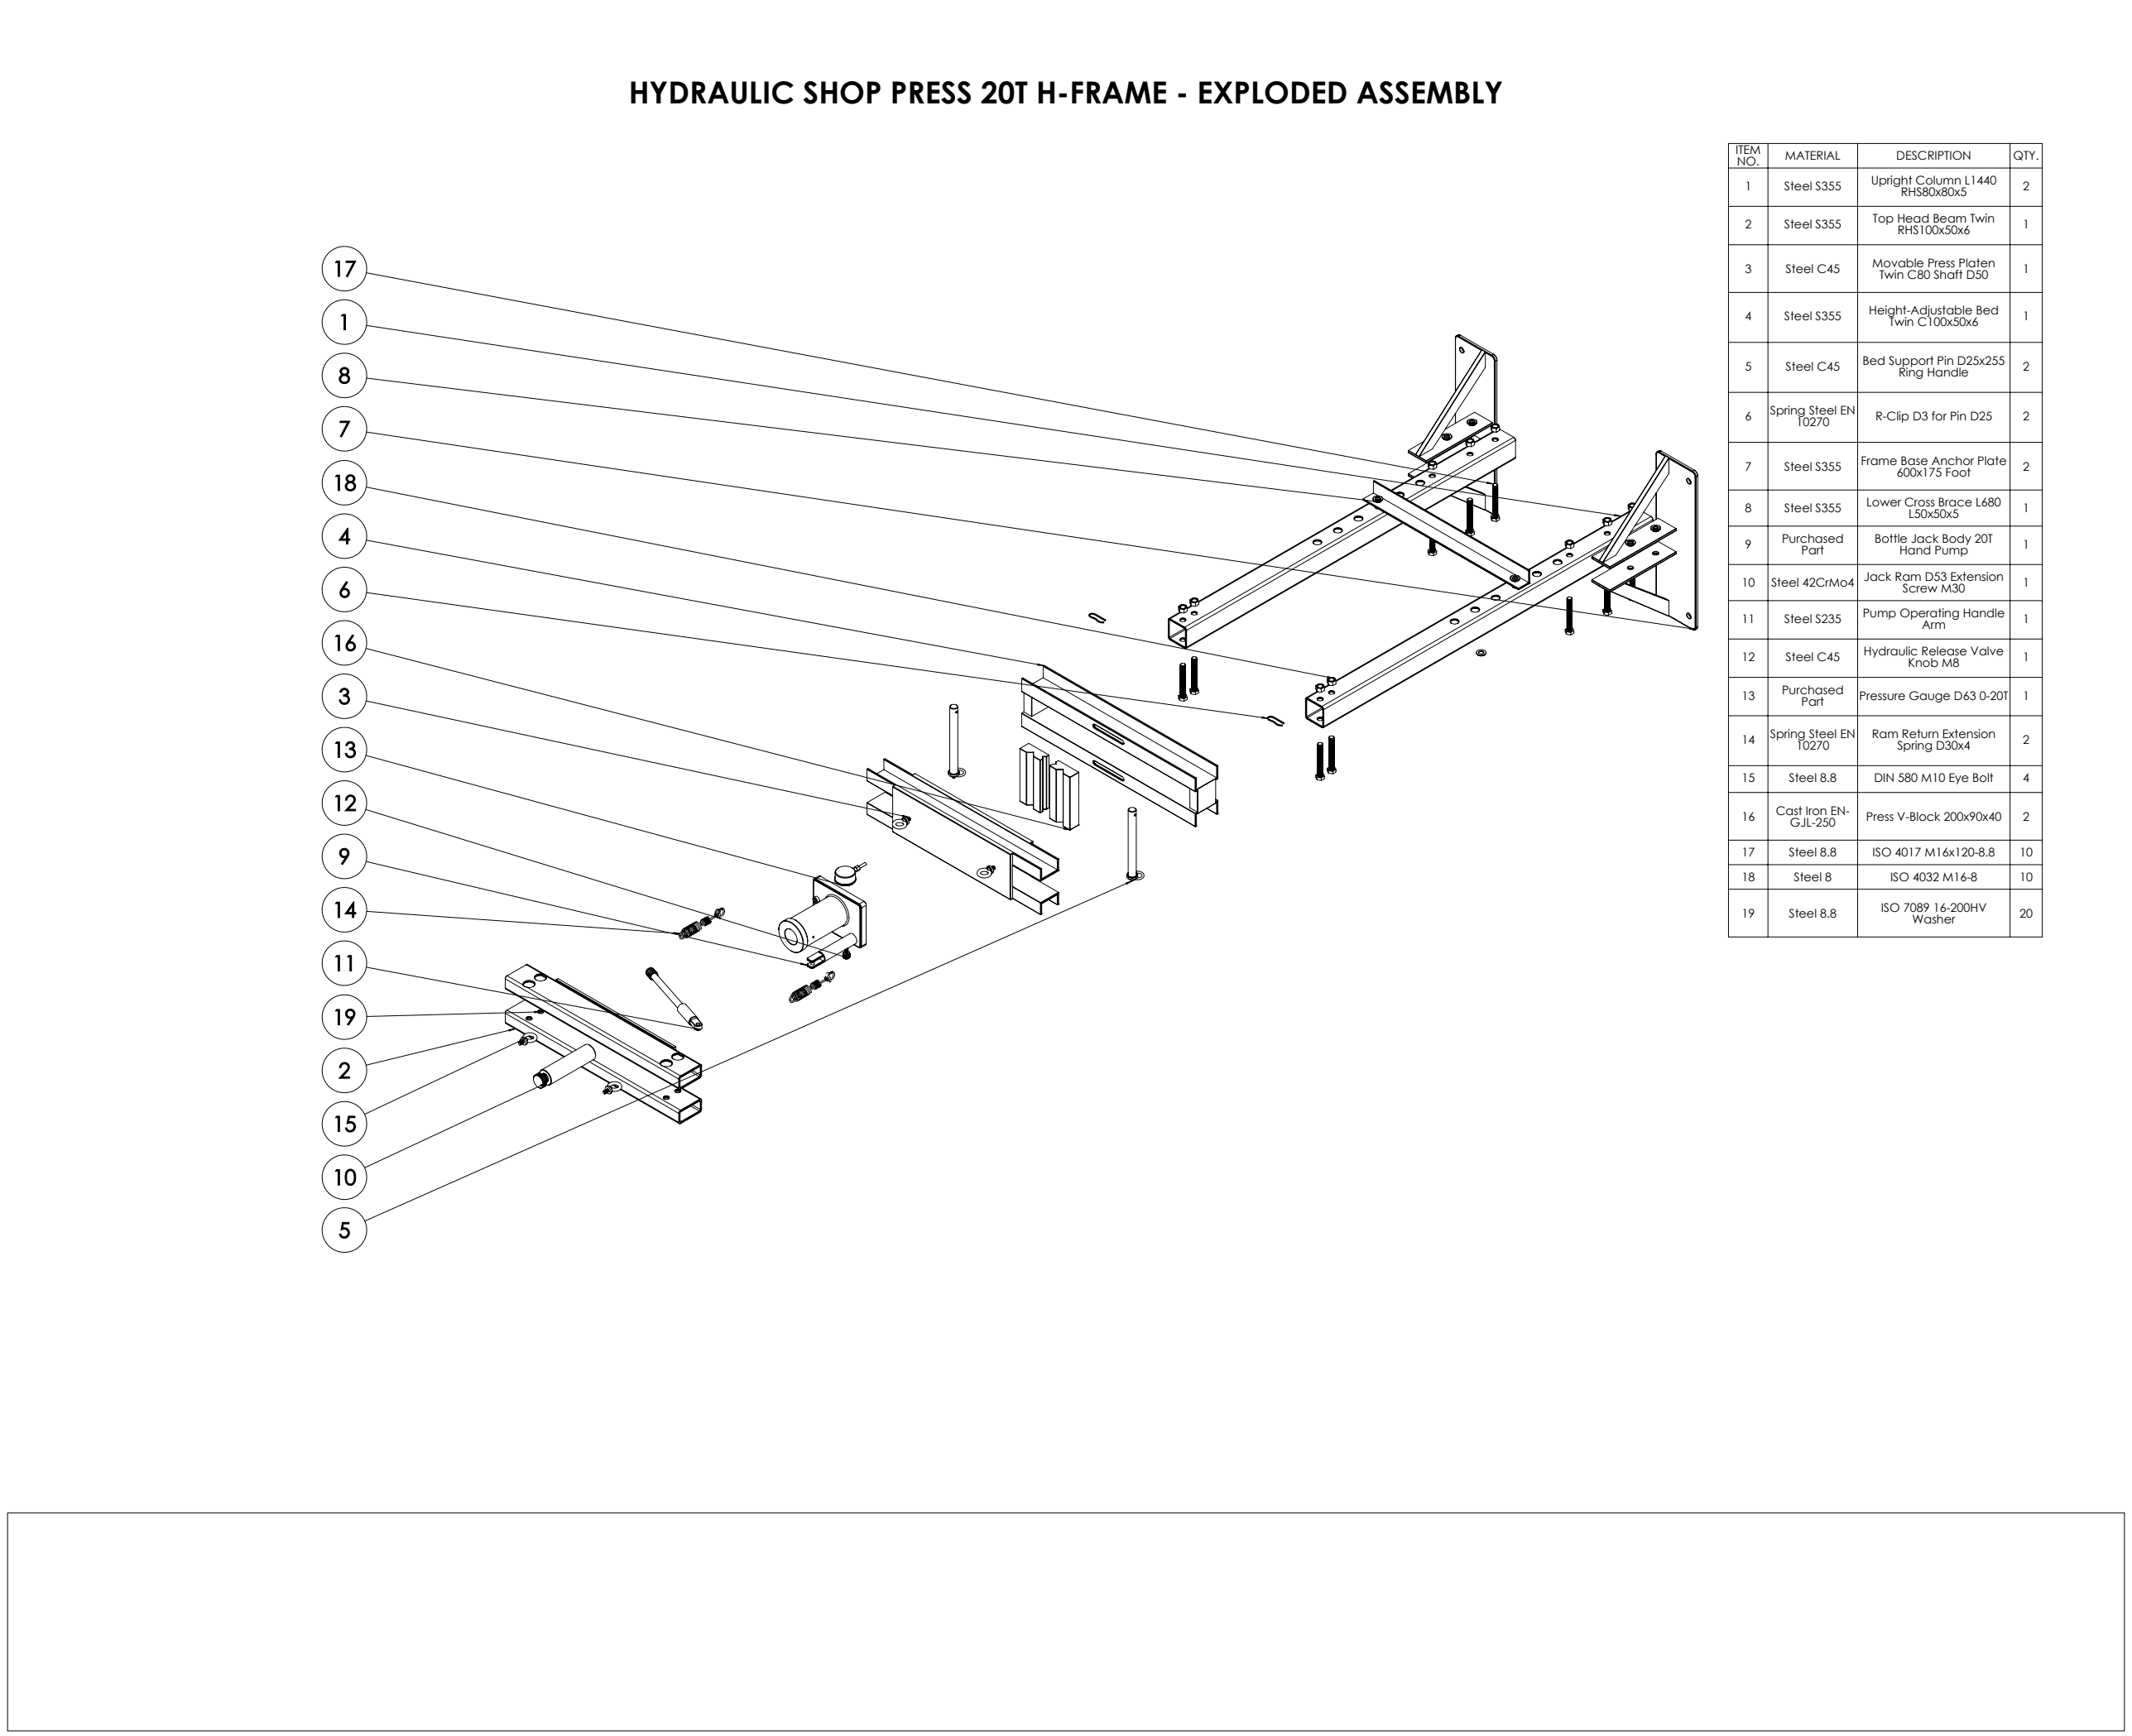
ISO-10303-21;
HEADER;
/* Generated by software containing ST-Developer
 * from STEP Tools, Inc. (www.steptools.com) 
 */

FILE_DESCRIPTION(
/* description */ (''),
/* implementation_level */ '2;1');

FILE_NAME(
/* name */ 'MAS-306',
/* time_stamp */ '2026-10-20T10:03:03-07:00',
/* author */ (''),
/* organization */ (''),
/* preprocessor_version */ 'ST-DEVELOPER v20.2',
/* originating_system */ 'Autodesk Translation Framework v15.15.0.0',
/* authorisation */ '');

FILE_SCHEMA (('AUTOMOTIVE_DESIGN { 1 0 10303 214 3 1 1 }'));
ENDSEC;

DATA;
#10=MECHANICAL_DESIGN_GEOMETRIC_PRESENTATION_REPRESENTATION('',(#439,#440,
#441,#442,#443,#444,#445,#446,#447,#448,#449,#450,#451,#452,#453,#454,#455,
#456,#457,#458,#459,#460,#461,#462,#463,#464,#465,#466,#467,#468,#469,#470,
#471,#472,#473,#474,#475,#476,#477,#478,#479,#480,#481,#482,#483,#484,#485,
#486,#487,#488,#489,#490,#491,#492,#493,#494,#495,#496,#497,#498,#499,#500,
#501,#502,#503,#504,#505,#506,#507,#508,#509,#510,#511,#512,#513,#514,#515,
#516,#517,#518,#519,#520,#521,#522,#523,#524,#525,#526,#527,#528,#529,#530,
#531,#532,#533,#534,#535,#536,#537,#538,#539,#540,#541,#542,#543,#544,#545,
#546,#547,#548,#549,#550),#71492);
#11=ITEM_DEFINED_TRANSFORMATION($,$,#30553,#30790);
#12=ITEM_DEFINED_TRANSFORMATION($,$,#28689,#30791);
#13=ITEM_DEFINED_TRANSFORMATION($,$,#29045,#30792);
#14=ITEM_DEFINED_TRANSFORMATION($,$,#29181,#30793);
#15=ITEM_DEFINED_TRANSFORMATION($,$,#29982,#30794);
#16=ITEM_DEFINED_TRANSFORMATION($,$,#30008,#30795);
#17=ITEM_DEFINED_TRANSFORMATION($,$,#30013,#30796);
#18=ITEM_DEFINED_TRANSFORMATION($,$,#29306,#30797);
#19=ITEM_DEFINED_TRANSFORMATION($,$,#29346,#30798);
#20=ITEM_DEFINED_TRANSFORMATION($,$,#29535,#30799);
#21=ITEM_DEFINED_TRANSFORMATION($,$,#29736,#30800);
#22=ITEM_DEFINED_TRANSFORMATION($,$,#29878,#30801);
#23=ITEM_DEFINED_TRANSFORMATION($,$,#30164,#30802);
#24=ITEM_DEFINED_TRANSFORMATION($,$,#30184,#30803);
#25=ITEM_DEFINED_TRANSFORMATION($,$,#30238,#30804);
#26=ITEM_DEFINED_TRANSFORMATION($,$,#30284,#30805);
#27=ITEM_DEFINED_TRANSFORMATION($,$,#30444,#30806);
#28=ITEM_DEFINED_TRANSFORMATION($,$,#30464,#30807);
#29=ITEM_DEFINED_TRANSFORMATION($,$,#29982,#30808);
#30=ITEM_DEFINED_TRANSFORMATION($,$,#30008,#30809);
#31=ITEM_DEFINED_TRANSFORMATION($,$,#30013,#30810);
#32=ITEM_DEFINED_TRANSFORMATION($,$,#30164,#30811);
#33=ITEM_DEFINED_TRANSFORMATION($,$,#30184,#30812);
#34=ITEM_DEFINED_TRANSFORMATION($,$,#30184,#30813);
#35=ITEM_DEFINED_TRANSFORMATION($,$,#30184,#30814);
#36=ITEM_DEFINED_TRANSFORMATION($,$,#30238,#30815);
#37=ITEM_DEFINED_TRANSFORMATION($,$,#30284,#30816);
#38=ITEM_DEFINED_TRANSFORMATION($,$,#30284,#30817);
#39=ITEM_DEFINED_TRANSFORMATION($,$,#30284,#30818);
#40=ITEM_DEFINED_TRANSFORMATION($,$,#30284,#30819);
#41=ITEM_DEFINED_TRANSFORMATION($,$,#30284,#30820);
#42=ITEM_DEFINED_TRANSFORMATION($,$,#30284,#30821);
#43=ITEM_DEFINED_TRANSFORMATION($,$,#30284,#30822);
#44=ITEM_DEFINED_TRANSFORMATION($,$,#30284,#30823);
#45=ITEM_DEFINED_TRANSFORMATION($,$,#30284,#30824);
#46=ITEM_DEFINED_TRANSFORMATION($,$,#30444,#30825);
#47=ITEM_DEFINED_TRANSFORMATION($,$,#30444,#30826);
#48=ITEM_DEFINED_TRANSFORMATION($,$,#30444,#30827);
#49=ITEM_DEFINED_TRANSFORMATION($,$,#30444,#30828);
#50=ITEM_DEFINED_TRANSFORMATION($,$,#30444,#30829);
#51=ITEM_DEFINED_TRANSFORMATION($,$,#30444,#30830);
#52=ITEM_DEFINED_TRANSFORMATION($,$,#30444,#30831);
#53=ITEM_DEFINED_TRANSFORMATION($,$,#30444,#30832);
#54=ITEM_DEFINED_TRANSFORMATION($,$,#30444,#30833);
#55=ITEM_DEFINED_TRANSFORMATION($,$,#30464,#30834);
#56=ITEM_DEFINED_TRANSFORMATION($,$,#30464,#30835);
#57=ITEM_DEFINED_TRANSFORMATION($,$,#30464,#30836);
#58=ITEM_DEFINED_TRANSFORMATION($,$,#30464,#30837);
#59=ITEM_DEFINED_TRANSFORMATION($,$,#30464,#30838);
#60=ITEM_DEFINED_TRANSFORMATION($,$,#30464,#30839);
#61=ITEM_DEFINED_TRANSFORMATION($,$,#30464,#30840);
#62=ITEM_DEFINED_TRANSFORMATION($,$,#30464,#30841);
#63=ITEM_DEFINED_TRANSFORMATION($,$,#30464,#30842);
#64=ITEM_DEFINED_TRANSFORMATION($,$,#30464,#30843);
#65=ITEM_DEFINED_TRANSFORMATION($,$,#30464,#30844);
#66=ITEM_DEFINED_TRANSFORMATION($,$,#30464,#30845);
#67=ITEM_DEFINED_TRANSFORMATION($,$,#30464,#30846);
#68=ITEM_DEFINED_TRANSFORMATION($,$,#30464,#30847);
#69=ITEM_DEFINED_TRANSFORMATION($,$,#30464,#30848);
#70=ITEM_DEFINED_TRANSFORMATION($,$,#30464,#30849);
#71=ITEM_DEFINED_TRANSFORMATION($,$,#30464,#30850);
#72=ITEM_DEFINED_TRANSFORMATION($,$,#30464,#30851);
#73=ITEM_DEFINED_TRANSFORMATION($,$,#30464,#30852);
#74=ITEM_DEFINED_TRANSFORMATION($,$,#30477,#30853);
#75=ITEM_DEFINED_TRANSFORMATION($,$,#30553,#30854);
#76=(
REPRESENTATION_RELATIONSHIP($,$,#71621,#71602)
REPRESENTATION_RELATIONSHIP_WITH_TRANSFORMATION(#11)
SHAPE_REPRESENTATION_RELATIONSHIP()
);
#77=(
REPRESENTATION_RELATIONSHIP($,$,#71603,#71602)
REPRESENTATION_RELATIONSHIP_WITH_TRANSFORMATION(#12)
SHAPE_REPRESENTATION_RELATIONSHIP()
);
#78=(
REPRESENTATION_RELATIONSHIP($,$,#71604,#71602)
REPRESENTATION_RELATIONSHIP_WITH_TRANSFORMATION(#13)
SHAPE_REPRESENTATION_RELATIONSHIP()
);
#79=(
REPRESENTATION_RELATIONSHIP($,$,#71605,#71602)
REPRESENTATION_RELATIONSHIP_WITH_TRANSFORMATION(#14)
SHAPE_REPRESENTATION_RELATIONSHIP()
);
#80=(
REPRESENTATION_RELATIONSHIP($,$,#71611,#71602)
REPRESENTATION_RELATIONSHIP_WITH_TRANSFORMATION(#15)
SHAPE_REPRESENTATION_RELATIONSHIP()
);
#81=(
REPRESENTATION_RELATIONSHIP($,$,#71612,#71602)
REPRESENTATION_RELATIONSHIP_WITH_TRANSFORMATION(#16)
SHAPE_REPRESENTATION_RELATIONSHIP()
);
#82=(
REPRESENTATION_RELATIONSHIP($,$,#71613,#71602)
REPRESENTATION_RELATIONSHIP_WITH_TRANSFORMATION(#17)
SHAPE_REPRESENTATION_RELATIONSHIP()
);
#83=(
REPRESENTATION_RELATIONSHIP($,$,#71606,#71602)
REPRESENTATION_RELATIONSHIP_WITH_TRANSFORMATION(#18)
SHAPE_REPRESENTATION_RELATIONSHIP()
);
#84=(
REPRESENTATION_RELATIONSHIP($,$,#71607,#71602)
REPRESENTATION_RELATIONSHIP_WITH_TRANSFORMATION(#19)
SHAPE_REPRESENTATION_RELATIONSHIP()
);
#85=(
REPRESENTATION_RELATIONSHIP($,$,#71608,#71602)
REPRESENTATION_RELATIONSHIP_WITH_TRANSFORMATION(#20)
SHAPE_REPRESENTATION_RELATIONSHIP()
);
#86=(
REPRESENTATION_RELATIONSHIP($,$,#71609,#71602)
REPRESENTATION_RELATIONSHIP_WITH_TRANSFORMATION(#21)
SHAPE_REPRESENTATION_RELATIONSHIP()
);
#87=(
REPRESENTATION_RELATIONSHIP($,$,#71610,#71602)
REPRESENTATION_RELATIONSHIP_WITH_TRANSFORMATION(#22)
SHAPE_REPRESENTATION_RELATIONSHIP()
);
#88=(
REPRESENTATION_RELATIONSHIP($,$,#71614,#71602)
REPRESENTATION_RELATIONSHIP_WITH_TRANSFORMATION(#23)
SHAPE_REPRESENTATION_RELATIONSHIP()
);
#89=(
REPRESENTATION_RELATIONSHIP($,$,#71615,#71602)
REPRESENTATION_RELATIONSHIP_WITH_TRANSFORMATION(#24)
SHAPE_REPRESENTATION_RELATIONSHIP()
);
#90=(
REPRESENTATION_RELATIONSHIP($,$,#71616,#71602)
REPRESENTATION_RELATIONSHIP_WITH_TRANSFORMATION(#25)
SHAPE_REPRESENTATION_RELATIONSHIP()
);
#91=(
REPRESENTATION_RELATIONSHIP($,$,#71617,#71602)
REPRESENTATION_RELATIONSHIP_WITH_TRANSFORMATION(#26)
SHAPE_REPRESENTATION_RELATIONSHIP()
);
#92=(
REPRESENTATION_RELATIONSHIP($,$,#71618,#71602)
REPRESENTATION_RELATIONSHIP_WITH_TRANSFORMATION(#27)
SHAPE_REPRESENTATION_RELATIONSHIP()
);
#93=(
REPRESENTATION_RELATIONSHIP($,$,#71619,#71602)
REPRESENTATION_RELATIONSHIP_WITH_TRANSFORMATION(#28)
SHAPE_REPRESENTATION_RELATIONSHIP()
);
#94=(
REPRESENTATION_RELATIONSHIP($,$,#71611,#71602)
REPRESENTATION_RELATIONSHIP_WITH_TRANSFORMATION(#29)
SHAPE_REPRESENTATION_RELATIONSHIP()
);
#95=(
REPRESENTATION_RELATIONSHIP($,$,#71612,#71602)
REPRESENTATION_RELATIONSHIP_WITH_TRANSFORMATION(#30)
SHAPE_REPRESENTATION_RELATIONSHIP()
);
#96=(
REPRESENTATION_RELATIONSHIP($,$,#71613,#71602)
REPRESENTATION_RELATIONSHIP_WITH_TRANSFORMATION(#31)
SHAPE_REPRESENTATION_RELATIONSHIP()
);
#97=(
REPRESENTATION_RELATIONSHIP($,$,#71614,#71602)
REPRESENTATION_RELATIONSHIP_WITH_TRANSFORMATION(#32)
SHAPE_REPRESENTATION_RELATIONSHIP()
);
#98=(
REPRESENTATION_RELATIONSHIP($,$,#71615,#71602)
REPRESENTATION_RELATIONSHIP_WITH_TRANSFORMATION(#33)
SHAPE_REPRESENTATION_RELATIONSHIP()
);
#99=(
REPRESENTATION_RELATIONSHIP($,$,#71615,#71602)
REPRESENTATION_RELATIONSHIP_WITH_TRANSFORMATION(#34)
SHAPE_REPRESENTATION_RELATIONSHIP()
);
#100=(
REPRESENTATION_RELATIONSHIP($,$,#71615,#71602)
REPRESENTATION_RELATIONSHIP_WITH_TRANSFORMATION(#35)
SHAPE_REPRESENTATION_RELATIONSHIP()
);
#101=(
REPRESENTATION_RELATIONSHIP($,$,#71616,#71602)
REPRESENTATION_RELATIONSHIP_WITH_TRANSFORMATION(#36)
SHAPE_REPRESENTATION_RELATIONSHIP()
);
#102=(
REPRESENTATION_RELATIONSHIP($,$,#71617,#71602)
REPRESENTATION_RELATIONSHIP_WITH_TRANSFORMATION(#37)
SHAPE_REPRESENTATION_RELATIONSHIP()
);
#103=(
REPRESENTATION_RELATIONSHIP($,$,#71617,#71602)
REPRESENTATION_RELATIONSHIP_WITH_TRANSFORMATION(#38)
SHAPE_REPRESENTATION_RELATIONSHIP()
);
#104=(
REPRESENTATION_RELATIONSHIP($,$,#71617,#71602)
REPRESENTATION_RELATIONSHIP_WITH_TRANSFORMATION(#39)
SHAPE_REPRESENTATION_RELATIONSHIP()
);
#105=(
REPRESENTATION_RELATIONSHIP($,$,#71617,#71602)
REPRESENTATION_RELATIONSHIP_WITH_TRANSFORMATION(#40)
SHAPE_REPRESENTATION_RELATIONSHIP()
);
#106=(
REPRESENTATION_RELATIONSHIP($,$,#71617,#71602)
REPRESENTATION_RELATIONSHIP_WITH_TRANSFORMATION(#41)
SHAPE_REPRESENTATION_RELATIONSHIP()
);
#107=(
REPRESENTATION_RELATIONSHIP($,$,#71617,#71602)
REPRESENTATION_RELATIONSHIP_WITH_TRANSFORMATION(#42)
SHAPE_REPRESENTATION_RELATIONSHIP()
);
#108=(
REPRESENTATION_RELATIONSHIP($,$,#71617,#71602)
REPRESENTATION_RELATIONSHIP_WITH_TRANSFORMATION(#43)
SHAPE_REPRESENTATION_RELATIONSHIP()
);
#109=(
REPRESENTATION_RELATIONSHIP($,$,#71617,#71602)
REPRESENTATION_RELATIONSHIP_WITH_TRANSFORMATION(#44)
SHAPE_REPRESENTATION_RELATIONSHIP()
);
#110=(
REPRESENTATION_RELATIONSHIP($,$,#71617,#71602)
REPRESENTATION_RELATIONSHIP_WITH_TRANSFORMATION(#45)
SHAPE_REPRESENTATION_RELATIONSHIP()
);
#111=(
REPRESENTATION_RELATIONSHIP($,$,#71618,#71602)
REPRESENTATION_RELATIONSHIP_WITH_TRANSFORMATION(#46)
SHAPE_REPRESENTATION_RELATIONSHIP()
);
#112=(
REPRESENTATION_RELATIONSHIP($,$,#71618,#71602)
REPRESENTATION_RELATIONSHIP_WITH_TRANSFORMATION(#47)
SHAPE_REPRESENTATION_RELATIONSHIP()
);
#113=(
REPRESENTATION_RELATIONSHIP($,$,#71618,#71602)
REPRESENTATION_RELATIONSHIP_WITH_TRANSFORMATION(#48)
SHAPE_REPRESENTATION_RELATIONSHIP()
);
#114=(
REPRESENTATION_RELATIONSHIP($,$,#71618,#71602)
REPRESENTATION_RELATIONSHIP_WITH_TRANSFORMATION(#49)
SHAPE_REPRESENTATION_RELATIONSHIP()
);
#115=(
REPRESENTATION_RELATIONSHIP($,$,#71618,#71602)
REPRESENTATION_RELATIONSHIP_WITH_TRANSFORMATION(#50)
SHAPE_REPRESENTATION_RELATIONSHIP()
);
#116=(
REPRESENTATION_RELATIONSHIP($,$,#71618,#71602)
REPRESENTATION_RELATIONSHIP_WITH_TRANSFORMATION(#51)
SHAPE_REPRESENTATION_RELATIONSHIP()
);
#117=(
REPRESENTATION_RELATIONSHIP($,$,#71618,#71602)
REPRESENTATION_RELATIONSHIP_WITH_TRANSFORMATION(#52)
SHAPE_REPRESENTATION_RELATIONSHIP()
);
#118=(
REPRESENTATION_RELATIONSHIP($,$,#71618,#71602)
REPRESENTATION_RELATIONSHIP_WITH_TRANSFORMATION(#53)
SHAPE_REPRESENTATION_RELATIONSHIP()
);
#119=(
REPRESENTATION_RELATIONSHIP($,$,#71618,#71602)
REPRESENTATION_RELATIONSHIP_WITH_TRANSFORMATION(#54)
SHAPE_REPRESENTATION_RELATIONSHIP()
);
#120=(
REPRESENTATION_RELATIONSHIP($,$,#71619,#71602)
REPRESENTATION_RELATIONSHIP_WITH_TRANSFORMATION(#55)
SHAPE_REPRESENTATION_RELATIONSHIP()
);
#121=(
REPRESENTATION_RELATIONSHIP($,$,#71619,#71602)
REPRESENTATION_RELATIONSHIP_WITH_TRANSFORMATION(#56)
SHAPE_REPRESENTATION_RELATIONSHIP()
);
#122=(
REPRESENTATION_RELATIONSHIP($,$,#71619,#71602)
REPRESENTATION_RELATIONSHIP_WITH_TRANSFORMATION(#57)
SHAPE_REPRESENTATION_RELATIONSHIP()
);
#123=(
REPRESENTATION_RELATIONSHIP($,$,#71619,#71602)
REPRESENTATION_RELATIONSHIP_WITH_TRANSFORMATION(#58)
SHAPE_REPRESENTATION_RELATIONSHIP()
);
#124=(
REPRESENTATION_RELATIONSHIP($,$,#71619,#71602)
REPRESENTATION_RELATIONSHIP_WITH_TRANSFORMATION(#59)
SHAPE_REPRESENTATION_RELATIONSHIP()
);
#125=(
REPRESENTATION_RELATIONSHIP($,$,#71619,#71602)
REPRESENTATION_RELATIONSHIP_WITH_TRANSFORMATION(#60)
SHAPE_REPRESENTATION_RELATIONSHIP()
);
#126=(
REPRESENTATION_RELATIONSHIP($,$,#71619,#71602)
REPRESENTATION_RELATIONSHIP_WITH_TRANSFORMATION(#61)
SHAPE_REPRESENTATION_RELATIONSHIP()
);
#127=(
REPRESENTATION_RELATIONSHIP($,$,#71619,#71602)
REPRESENTATION_RELATIONSHIP_WITH_TRANSFORMATION(#62)
SHAPE_REPRESENTATION_RELATIONSHIP()
);
#128=(
REPRESENTATION_RELATIONSHIP($,$,#71619,#71602)
REPRESENTATION_RELATIONSHIP_WITH_TRANSFORMATION(#63)
SHAPE_REPRESENTATION_RELATIONSHIP()
);
#129=(
REPRESENTATION_RELATIONSHIP($,$,#71619,#71602)
REPRESENTATION_RELATIONSHIP_WITH_TRANSFORMATION(#64)
SHAPE_REPRESENTATION_RELATIONSHIP()
);
#130=(
REPRESENTATION_RELATIONSHIP($,$,#71619,#71602)
REPRESENTATION_RELATIONSHIP_WITH_TRANSFORMATION(#65)
SHAPE_REPRESENTATION_RELATIONSHIP()
);
#131=(
REPRESENTATION_RELATIONSHIP($,$,#71619,#71602)
REPRESENTATION_RELATIONSHIP_WITH_TRANSFORMATION(#66)
SHAPE_REPRESENTATION_RELATIONSHIP()
);
#132=(
REPRESENTATION_RELATIONSHIP($,$,#71619,#71602)
REPRESENTATION_RELATIONSHIP_WITH_TRANSFORMATION(#67)
SHAPE_REPRESENTATION_RELATIONSHIP()
);
#133=(
REPRESENTATION_RELATIONSHIP($,$,#71619,#71602)
REPRESENTATION_RELATIONSHIP_WITH_TRANSFORMATION(#68)
SHAPE_REPRESENTATION_RELATIONSHIP()
);
#134=(
REPRESENTATION_RELATIONSHIP($,$,#71619,#71602)
REPRESENTATION_RELATIONSHIP_WITH_TRANSFORMATION(#69)
SHAPE_REPRESENTATION_RELATIONSHIP()
);
#135=(
REPRESENTATION_RELATIONSHIP($,$,#71619,#71602)
REPRESENTATION_RELATIONSHIP_WITH_TRANSFORMATION(#70)
SHAPE_REPRESENTATION_RELATIONSHIP()
);
#136=(
REPRESENTATION_RELATIONSHIP($,$,#71619,#71602)
REPRESENTATION_RELATIONSHIP_WITH_TRANSFORMATION(#71)
SHAPE_REPRESENTATION_RELATIONSHIP()
);
#137=(
REPRESENTATION_RELATIONSHIP($,$,#71619,#71602)
REPRESENTATION_RELATIONSHIP_WITH_TRANSFORMATION(#72)
SHAPE_REPRESENTATION_RELATIONSHIP()
);
#138=(
REPRESENTATION_RELATIONSHIP($,$,#71619,#71602)
REPRESENTATION_RELATIONSHIP_WITH_TRANSFORMATION(#73)
SHAPE_REPRESENTATION_RELATIONSHIP()
);
#139=(
REPRESENTATION_RELATIONSHIP($,$,#71620,#71602)
REPRESENTATION_RELATIONSHIP_WITH_TRANSFORMATION(#74)
SHAPE_REPRESENTATION_RELATIONSHIP()
);
#140=(
REPRESENTATION_RELATIONSHIP($,$,#71621,#71602)
REPRESENTATION_RELATIONSHIP_WITH_TRANSFORMATION(#75)
SHAPE_REPRESENTATION_RELATIONSHIP()
);
#141=CONTEXT_DEPENDENT_SHAPE_REPRESENTATION(#76,#71537);
#142=CONTEXT_DEPENDENT_SHAPE_REPRESENTATION(#77,#71538);
#143=CONTEXT_DEPENDENT_SHAPE_REPRESENTATION(#78,#71539);
#144=CONTEXT_DEPENDENT_SHAPE_REPRESENTATION(#79,#71540);
#145=CONTEXT_DEPENDENT_SHAPE_REPRESENTATION(#80,#71541);
#146=CONTEXT_DEPENDENT_SHAPE_REPRESENTATION(#81,#71542);
#147=CONTEXT_DEPENDENT_SHAPE_REPRESENTATION(#82,#71543);
#148=CONTEXT_DEPENDENT_SHAPE_REPRESENTATION(#83,#71544);
#149=CONTEXT_DEPENDENT_SHAPE_REPRESENTATION(#84,#71545);
#150=CONTEXT_DEPENDENT_SHAPE_REPRESENTATION(#85,#71546);
#151=CONTEXT_DEPENDENT_SHAPE_REPRESENTATION(#86,#71547);
#152=CONTEXT_DEPENDENT_SHAPE_REPRESENTATION(#87,#71548);
#153=CONTEXT_DEPENDENT_SHAPE_REPRESENTATION(#88,#71549);
#154=CONTEXT_DEPENDENT_SHAPE_REPRESENTATION(#89,#71550);
#155=CONTEXT_DEPENDENT_SHAPE_REPRESENTATION(#90,#71551);
#156=CONTEXT_DEPENDENT_SHAPE_REPRESENTATION(#91,#71552);
#157=CONTEXT_DEPENDENT_SHAPE_REPRESENTATION(#92,#71553);
#158=CONTEXT_DEPENDENT_SHAPE_REPRESENTATION(#93,#71554);
#159=CONTEXT_DEPENDENT_SHAPE_REPRESENTATION(#94,#71555);
#160=CONTEXT_DEPENDENT_SHAPE_REPRESENTATION(#95,#71556);
#161=CONTEXT_DEPENDENT_SHAPE_REPRESENTATION(#96,#71557);
#162=CONTEXT_DEPENDENT_SHAPE_REPRESENTATION(#97,#71558);
#163=CONTEXT_DEPENDENT_SHAPE_REPRESENTATION(#98,#71559);
#164=CONTEXT_DEPENDENT_SHAPE_REPRESENTATION(#99,#71560);
#165=CONTEXT_DEPENDENT_SHAPE_REPRESENTATION(#100,#71561);
#166=CONTEXT_DEPENDENT_SHAPE_REPRESENTATION(#101,#71562);
#167=CONTEXT_DEPENDENT_SHAPE_REPRESENTATION(#102,#71563);
#168=CONTEXT_DEPENDENT_SHAPE_REPRESENTATION(#103,#71564);
#169=CONTEXT_DEPENDENT_SHAPE_REPRESENTATION(#104,#71565);
#170=CONTEXT_DEPENDENT_SHAPE_REPRESENTATION(#105,#71566);
#171=CONTEXT_DEPENDENT_SHAPE_REPRESENTATION(#106,#71567);
#172=CONTEXT_DEPENDENT_SHAPE_REPRESENTATION(#107,#71568);
#173=CONTEXT_DEPENDENT_SHAPE_REPRESENTATION(#108,#71569);
#174=CONTEXT_DEPENDENT_SHAPE_REPRESENTATION(#109,#71570);
#175=CONTEXT_DEPENDENT_SHAPE_REPRESENTATION(#110,#71571);
#176=CONTEXT_DEPENDENT_SHAPE_REPRESENTATION(#111,#71572);
#177=CONTEXT_DEPENDENT_SHAPE_REPRESENTATION(#112,#71573);
#178=CONTEXT_DEPENDENT_SHAPE_REPRESENTATION(#113,#71574);
#179=CONTEXT_DEPENDENT_SHAPE_REPRESENTATION(#114,#71575);
#180=CONTEXT_DEPENDENT_SHAPE_REPRESENTATION(#115,#71576);
#181=CONTEXT_DEPENDENT_SHAPE_REPRESENTATION(#116,#71577);
#182=CONTEXT_DEPENDENT_SHAPE_REPRESENTATION(#117,#71578);
#183=CONTEXT_DEPENDENT_SHAPE_REPRESENTATION(#118,#71579);
#184=CONTEXT_DEPENDENT_SHAPE_REPRESENTATION(#119,#71580);
#185=CONTEXT_DEPENDENT_SHAPE_REPRESENTATION(#120,#71581);
#186=CONTEXT_DEPENDENT_SHAPE_REPRESENTATION(#121,#71582);
#187=CONTEXT_DEPENDENT_SHAPE_REPRESENTATION(#122,#71583);
#188=CONTEXT_DEPENDENT_SHAPE_REPRESENTATION(#123,#71584);
#189=CONTEXT_DEPENDENT_SHAPE_REPRESENTATION(#124,#71585);
#190=CONTEXT_DEPENDENT_SHAPE_REPRESENTATION(#125,#71586);
#191=CONTEXT_DEPENDENT_SHAPE_REPRESENTATION(#126,#71587);
#192=CONTEXT_DEPENDENT_SHAPE_REPRESENTATION(#127,#71588);
#193=CONTEXT_DEPENDENT_SHAPE_REPRESENTATION(#128,#71589);
#194=CONTEXT_DEPENDENT_SHAPE_REPRESENTATION(#129,#71590);
#195=CONTEXT_DEPENDENT_SHAPE_REPRESENTATION(#130,#71591);
#196=CONTEXT_DEPENDENT_SHAPE_REPRESENTATION(#131,#71592);
#197=CONTEXT_DEPENDENT_SHAPE_REPRESENTATION(#132,#71593);
#198=CONTEXT_DEPENDENT_SHAPE_REPRESENTATION(#133,#71594);
#199=CONTEXT_DEPENDENT_SHAPE_REPRESENTATION(#134,#71595);
#200=CONTEXT_DEPENDENT_SHAPE_REPRESENTATION(#135,#71596);
#201=CONTEXT_DEPENDENT_SHAPE_REPRESENTATION(#136,#71597);
#202=CONTEXT_DEPENDENT_SHAPE_REPRESENTATION(#137,#71598);
#203=CONTEXT_DEPENDENT_SHAPE_REPRESENTATION(#138,#71599);
#204=CONTEXT_DEPENDENT_SHAPE_REPRESENTATION(#139,#71600);
#205=CONTEXT_DEPENDENT_SHAPE_REPRESENTATION(#140,#71601);
#206=NEXT_ASSEMBLY_USAGE_OCCURRENCE(
'01_Upright_Column_L1440_RHS80x80x5:1',
'01_Upright_Column_L1440_RHS80x80x5:1',
'01_Upright_Column_L1440_RHS80x80x5:1',#71623,#71642,
'01_Upright_Column_L1440_RHS80x80x5:1');
#207=NEXT_ASSEMBLY_USAGE_OCCURRENCE(
'02_Top_Head_Beam_Twin_RHS100x50x6:1',
'02_Top_Head_Beam_Twin_RHS100x50x6:1',
'02_Top_Head_Beam_Twin_RHS100x50x6:1',#71623,#71624,
'02_Top_Head_Beam_Twin_RHS100x50x6:1');
#208=NEXT_ASSEMBLY_USAGE_OCCURRENCE(
'03_Movable_Press_Platen_Twin_C80_Shaft_D50:1',
'03_Movable_Press_Platen_Twin_C80_Shaft_D50:1',
'03_Movable_Press_Platen_Twin_C80_Shaft_D50:1',#71623,#71625,
'03_Movable_Press_Platen_Twin_C80_Shaft_D50:1');
#209=NEXT_ASSEMBLY_USAGE_OCCURRENCE(
'04_Height-Adjustable_Bed_Twin_C100x50x6:1',
'04_Height-Adjustable_Bed_Twin_C100x50x6:1',
'04_Height-Adjustable_Bed_Twin_C100x50x6:1',#71623,#71626,
'04_Height-Adjustable_Bed_Twin_C100x50x6:1');
#210=NEXT_ASSEMBLY_USAGE_OCCURRENCE(
'05_Bed_Support_Pin_D25x255_Ring_Handle:1',
'05_Bed_Support_Pin_D25x255_Ring_Handle:1',
'05_Bed_Support_Pin_D25x255_Ring_Handle:1',#71623,#71632,
'05_Bed_Support_Pin_D25x255_Ring_Handle:1');
#211=NEXT_ASSEMBLY_USAGE_OCCURRENCE('06_R-Clip_D3_for_Pin_D25:1',
'06_R-Clip_D3_for_Pin_D25:1','06_R-Clip_D3_for_Pin_D25:1',#71623,#71633,
'06_R-Clip_D3_for_Pin_D25:1');
#212=NEXT_ASSEMBLY_USAGE_OCCURRENCE(
'07_Frame_Base_Anchor_Plate_600x175_Foot:1',
'07_Frame_Base_Anchor_Plate_600x175_Foot:1',
'07_Frame_Base_Anchor_Plate_600x175_Foot:1',#71623,#71634,
'07_Frame_Base_Anchor_Plate_600x175_Foot:1');
#213=NEXT_ASSEMBLY_USAGE_OCCURRENCE(
'08_Lower_Cross_Brace_L680_L50x50x5:1',
'08_Lower_Cross_Brace_L680_L50x50x5:1',
'08_Lower_Cross_Brace_L680_L50x50x5:1',#71623,#71627,
'08_Lower_Cross_Brace_L680_L50x50x5:1');
#214=NEXT_ASSEMBLY_USAGE_OCCURRENCE(
'09_Bottle_Jack_Body_20T_Hand_Pump:1',
'09_Bottle_Jack_Body_20T_Hand_Pump:1',
'09_Bottle_Jack_Body_20T_Hand_Pump:1',#71623,#71628,
'09_Bottle_Jack_Body_20T_Hand_Pump:1');
#215=NEXT_ASSEMBLY_USAGE_OCCURRENCE(
'10_Jack_Ram_D53_Extension_Screw_M30:1',
'10_Jack_Ram_D53_Extension_Screw_M30:1',
'10_Jack_Ram_D53_Extension_Screw_M30:1',#71623,#71629,
'10_Jack_Ram_D53_Extension_Screw_M30:1');
#216=NEXT_ASSEMBLY_USAGE_OCCURRENCE(
'12_Hydraulic_Release_Valve_Knob_M8:1',
'12_Hydraulic_Release_Valve_Knob_M8:1',
'12_Hydraulic_Release_Valve_Knob_M8:1',#71623,#71630,
'12_Hydraulic_Release_Valve_Knob_M8:1');
#217=NEXT_ASSEMBLY_USAGE_OCCURRENCE('13_Pressure_Gauge_D63_0-20T:1',
'13_Pressure_Gauge_D63_0-20T:1','13_Pressure_Gauge_D63_0-20T:1',#71623,
#71631,'13_Pressure_Gauge_D63_0-20T:1');
#218=NEXT_ASSEMBLY_USAGE_OCCURRENCE(
'14_Ram_Return_Extension_Spring_D30x4:1',
'14_Ram_Return_Extension_Spring_D30x4:1',
'14_Ram_Return_Extension_Spring_D30x4:1',#71623,#71635,
'14_Ram_Return_Extension_Spring_D30x4:1');
#219=NEXT_ASSEMBLY_USAGE_OCCURRENCE('15_DIN_580_M10_Eye_Bolt:1',
'15_DIN_580_M10_Eye_Bolt:1','15_DIN_580_M10_Eye_Bolt:1',#71623,#71636,
'15_DIN_580_M10_Eye_Bolt:1');
#220=NEXT_ASSEMBLY_USAGE_OCCURRENCE('16_Press_V-Block_200x90x40:1',
'16_Press_V-Block_200x90x40:1','16_Press_V-Block_200x90x40:1',#71623,#71637,
'16_Press_V-Block_200x90x40:1');
#221=NEXT_ASSEMBLY_USAGE_OCCURRENCE('17_ISO_4017_M16x120-8.8:1',
'17_ISO_4017_M16x120-8.8:1','17_ISO_4017_M16x120-8.8:1',#71623,#71638,
'17_ISO_4017_M16x120-8.8:1');
#222=NEXT_ASSEMBLY_USAGE_OCCURRENCE('18_ISO_4032_M16-8:1',
'18_ISO_4032_M16-8:1','18_ISO_4032_M16-8:1',#71623,#71639,
'18_ISO_4032_M16-8:1');
#223=NEXT_ASSEMBLY_USAGE_OCCURRENCE('19_ISO_7089_16-200HV_Washer:1',
'19_ISO_7089_16-200HV_Washer:1','19_ISO_7089_16-200HV_Washer:1',#71623,
#71640,'19_ISO_7089_16-200HV_Washer:1');
#224=NEXT_ASSEMBLY_USAGE_OCCURRENCE(
'05_Bed_Support_Pin_D25x255_Ring_Handle:2',
'05_Bed_Support_Pin_D25x255_Ring_Handle:2',
'05_Bed_Support_Pin_D25x255_Ring_Handle:2',#71623,#71632,
'05_Bed_Support_Pin_D25x255_Ring_Handle:2');
#225=NEXT_ASSEMBLY_USAGE_OCCURRENCE('06_R-Clip_D3_for_Pin_D25:2',
'06_R-Clip_D3_for_Pin_D25:2','06_R-Clip_D3_for_Pin_D25:2',#71623,#71633,
'06_R-Clip_D3_for_Pin_D25:2');
#226=NEXT_ASSEMBLY_USAGE_OCCURRENCE(
'07_Frame_Base_Anchor_Plate_600x175_Foot:2',
'07_Frame_Base_Anchor_Plate_600x175_Foot:2',
'07_Frame_Base_Anchor_Plate_600x175_Foot:2',#71623,#71634,
'07_Frame_Base_Anchor_Plate_600x175_Foot:2');
#227=NEXT_ASSEMBLY_USAGE_OCCURRENCE(
'14_Ram_Return_Extension_Spring_D30x4:2',
'14_Ram_Return_Extension_Spring_D30x4:2',
'14_Ram_Return_Extension_Spring_D30x4:2',#71623,#71635,
'14_Ram_Return_Extension_Spring_D30x4:2');
#228=NEXT_ASSEMBLY_USAGE_OCCURRENCE('15_DIN_580_M10_Eye_Bolt:2',
'15_DIN_580_M10_Eye_Bolt:2','15_DIN_580_M10_Eye_Bolt:2',#71623,#71636,
'15_DIN_580_M10_Eye_Bolt:2');
#229=NEXT_ASSEMBLY_USAGE_OCCURRENCE('15_DIN_580_M10_Eye_Bolt:3',
'15_DIN_580_M10_Eye_Bolt:3','15_DIN_580_M10_Eye_Bolt:3',#71623,#71636,
'15_DIN_580_M10_Eye_Bolt:3');
#230=NEXT_ASSEMBLY_USAGE_OCCURRENCE('15_DIN_580_M10_Eye_Bolt:4',
'15_DIN_580_M10_Eye_Bolt:4','15_DIN_580_M10_Eye_Bolt:4',#71623,#71636,
'15_DIN_580_M10_Eye_Bolt:4');
#231=NEXT_ASSEMBLY_USAGE_OCCURRENCE('16_Press_V-Block_200x90x40:2',
'16_Press_V-Block_200x90x40:2','16_Press_V-Block_200x90x40:2',#71623,#71637,
'16_Press_V-Block_200x90x40:2');
#232=NEXT_ASSEMBLY_USAGE_OCCURRENCE('17_ISO_4017_M16x120-8.8:2',
'17_ISO_4017_M16x120-8.8:2','17_ISO_4017_M16x120-8.8:2',#71623,#71638,
'17_ISO_4017_M16x120-8.8:2');
#233=NEXT_ASSEMBLY_USAGE_OCCURRENCE('17_ISO_4017_M16x120-8.8:3',
'17_ISO_4017_M16x120-8.8:3','17_ISO_4017_M16x120-8.8:3',#71623,#71638,
'17_ISO_4017_M16x120-8.8:3');
#234=NEXT_ASSEMBLY_USAGE_OCCURRENCE('17_ISO_4017_M16x120-8.8:4',
'17_ISO_4017_M16x120-8.8:4','17_ISO_4017_M16x120-8.8:4',#71623,#71638,
'17_ISO_4017_M16x120-8.8:4');
#235=NEXT_ASSEMBLY_USAGE_OCCURRENCE('17_ISO_4017_M16x120-8.8:5',
'17_ISO_4017_M16x120-8.8:5','17_ISO_4017_M16x120-8.8:5',#71623,#71638,
'17_ISO_4017_M16x120-8.8:5');
#236=NEXT_ASSEMBLY_USAGE_OCCURRENCE('17_ISO_4017_M16x120-8.8:6',
'17_ISO_4017_M16x120-8.8:6','17_ISO_4017_M16x120-8.8:6',#71623,#71638,
'17_ISO_4017_M16x120-8.8:6');
#237=NEXT_ASSEMBLY_USAGE_OCCURRENCE('17_ISO_4017_M16x120-8.8:7',
'17_ISO_4017_M16x120-8.8:7','17_ISO_4017_M16x120-8.8:7',#71623,#71638,
'17_ISO_4017_M16x120-8.8:7');
#238=NEXT_ASSEMBLY_USAGE_OCCURRENCE('17_ISO_4017_M16x120-8.8:8',
'17_ISO_4017_M16x120-8.8:8','17_ISO_4017_M16x120-8.8:8',#71623,#71638,
'17_ISO_4017_M16x120-8.8:8');
#239=NEXT_ASSEMBLY_USAGE_OCCURRENCE('17_ISO_4017_M16x120-8.8:9',
'17_ISO_4017_M16x120-8.8:9','17_ISO_4017_M16x120-8.8:9',#71623,#71638,
'17_ISO_4017_M16x120-8.8:9');
#240=NEXT_ASSEMBLY_USAGE_OCCURRENCE('17_ISO_4017_M16x120-8.8:10',
'17_ISO_4017_M16x120-8.8:10','17_ISO_4017_M16x120-8.8:10',#71623,#71638,
'17_ISO_4017_M16x120-8.8:10');
#241=NEXT_ASSEMBLY_USAGE_OCCURRENCE('18_ISO_4032_M16-8:2',
'18_ISO_4032_M16-8:2','18_ISO_4032_M16-8:2',#71623,#71639,
'18_ISO_4032_M16-8:2');
#242=NEXT_ASSEMBLY_USAGE_OCCURRENCE('18_ISO_4032_M16-8:3',
'18_ISO_4032_M16-8:3','18_ISO_4032_M16-8:3',#71623,#71639,
'18_ISO_4032_M16-8:3');
#243=NEXT_ASSEMBLY_USAGE_OCCURRENCE('18_ISO_4032_M16-8:4',
'18_ISO_4032_M16-8:4','18_ISO_4032_M16-8:4',#71623,#71639,
'18_ISO_4032_M16-8:4');
#244=NEXT_ASSEMBLY_USAGE_OCCURRENCE('18_ISO_4032_M16-8:5',
'18_ISO_4032_M16-8:5','18_ISO_4032_M16-8:5',#71623,#71639,
'18_ISO_4032_M16-8:5');
#245=NEXT_ASSEMBLY_USAGE_OCCURRENCE('18_ISO_4032_M16-8:6',
'18_ISO_4032_M16-8:6','18_ISO_4032_M16-8:6',#71623,#71639,
'18_ISO_4032_M16-8:6');
#246=NEXT_ASSEMBLY_USAGE_OCCURRENCE('18_ISO_4032_M16-8:7',
'18_ISO_4032_M16-8:7','18_ISO_4032_M16-8:7',#71623,#71639,
'18_ISO_4032_M16-8:7');
#247=NEXT_ASSEMBLY_USAGE_OCCURRENCE('18_ISO_4032_M16-8:8',
'18_ISO_4032_M16-8:8','18_ISO_4032_M16-8:8',#71623,#71639,
'18_ISO_4032_M16-8:8');
#248=NEXT_ASSEMBLY_USAGE_OCCURRENCE('18_ISO_4032_M16-8:9',
'18_ISO_4032_M16-8:9','18_ISO_4032_M16-8:9',#71623,#71639,
'18_ISO_4032_M16-8:9');
#249=NEXT_ASSEMBLY_USAGE_OCCURRENCE('18_ISO_4032_M16-8:10',
'18_ISO_4032_M16-8:10','18_ISO_4032_M16-8:10',#71623,#71639,
'18_ISO_4032_M16-8:10');
#250=NEXT_ASSEMBLY_USAGE_OCCURRENCE('19_ISO_7089_16-200HV_Washer:2',
'19_ISO_7089_16-200HV_Washer:2','19_ISO_7089_16-200HV_Washer:2',#71623,
#71640,'19_ISO_7089_16-200HV_Washer:2');
#251=NEXT_ASSEMBLY_USAGE_OCCURRENCE('19_ISO_7089_16-200HV_Washer:3',
'19_ISO_7089_16-200HV_Washer:3','19_ISO_7089_16-200HV_Washer:3',#71623,
#71640,'19_ISO_7089_16-200HV_Washer:3');
#252=NEXT_ASSEMBLY_USAGE_OCCURRENCE('19_ISO_7089_16-200HV_Washer:4',
'19_ISO_7089_16-200HV_Washer:4','19_ISO_7089_16-200HV_Washer:4',#71623,
#71640,'19_ISO_7089_16-200HV_Washer:4');
#253=NEXT_ASSEMBLY_USAGE_OCCURRENCE('19_ISO_7089_16-200HV_Washer:5',
'19_ISO_7089_16-200HV_Washer:5','19_ISO_7089_16-200HV_Washer:5',#71623,
#71640,'19_ISO_7089_16-200HV_Washer:5');
#254=NEXT_ASSEMBLY_USAGE_OCCURRENCE('19_ISO_7089_16-200HV_Washer:6',
'19_ISO_7089_16-200HV_Washer:6','19_ISO_7089_16-200HV_Washer:6',#71623,
#71640,'19_ISO_7089_16-200HV_Washer:6');
#255=NEXT_ASSEMBLY_USAGE_OCCURRENCE('19_ISO_7089_16-200HV_Washer:7',
'19_ISO_7089_16-200HV_Washer:7','19_ISO_7089_16-200HV_Washer:7',#71623,
#71640,'19_ISO_7089_16-200HV_Washer:7');
#256=NEXT_ASSEMBLY_USAGE_OCCURRENCE('19_ISO_7089_16-200HV_Washer:8',
'19_ISO_7089_16-200HV_Washer:8','19_ISO_7089_16-200HV_Washer:8',#71623,
#71640,'19_ISO_7089_16-200HV_Washer:8');
#257=NEXT_ASSEMBLY_USAGE_OCCURRENCE('19_ISO_7089_16-200HV_Washer:9',
'19_ISO_7089_16-200HV_Washer:9','19_ISO_7089_16-200HV_Washer:9',#71623,
#71640,'19_ISO_7089_16-200HV_Washer:9');
#258=NEXT_ASSEMBLY_USAGE_OCCURRENCE('19_ISO_7089_16-200HV_Washer:10',
'19_ISO_7089_16-200HV_Washer:10','19_ISO_7089_16-200HV_Washer:10',#71623,
#71640,'19_ISO_7089_16-200HV_Washer:10');
#259=NEXT_ASSEMBLY_USAGE_OCCURRENCE('19_ISO_7089_16-200HV_Washer:11',
'19_ISO_7089_16-200HV_Washer:11','19_ISO_7089_16-200HV_Washer:11',#71623,
#71640,'19_ISO_7089_16-200HV_Washer:11');
#260=NEXT_ASSEMBLY_USAGE_OCCURRENCE('19_ISO_7089_16-200HV_Washer:12',
'19_ISO_7089_16-200HV_Washer:12','19_ISO_7089_16-200HV_Washer:12',#71623,
#71640,'19_ISO_7089_16-200HV_Washer:12');
#261=NEXT_ASSEMBLY_USAGE_OCCURRENCE('19_ISO_7089_16-200HV_Washer:13',
'19_ISO_7089_16-200HV_Washer:13','19_ISO_7089_16-200HV_Washer:13',#71623,
#71640,'19_ISO_7089_16-200HV_Washer:13');
#262=NEXT_ASSEMBLY_USAGE_OCCURRENCE('19_ISO_7089_16-200HV_Washer:14',
'19_ISO_7089_16-200HV_Washer:14','19_ISO_7089_16-200HV_Washer:14',#71623,
#71640,'19_ISO_7089_16-200HV_Washer:14');
#263=NEXT_ASSEMBLY_USAGE_OCCURRENCE('19_ISO_7089_16-200HV_Washer:15',
'19_ISO_7089_16-200HV_Washer:15','19_ISO_7089_16-200HV_Washer:15',#71623,
#71640,'19_ISO_7089_16-200HV_Washer:15');
#264=NEXT_ASSEMBLY_USAGE_OCCURRENCE('19_ISO_7089_16-200HV_Washer:16',
'19_ISO_7089_16-200HV_Washer:16','19_ISO_7089_16-200HV_Washer:16',#71623,
#71640,'19_ISO_7089_16-200HV_Washer:16');
#265=NEXT_ASSEMBLY_USAGE_OCCURRENCE('19_ISO_7089_16-200HV_Washer:17',
'19_ISO_7089_16-200HV_Washer:17','19_ISO_7089_16-200HV_Washer:17',#71623,
#71640,'19_ISO_7089_16-200HV_Washer:17');
#266=NEXT_ASSEMBLY_USAGE_OCCURRENCE('19_ISO_7089_16-200HV_Washer:18',
'19_ISO_7089_16-200HV_Washer:18','19_ISO_7089_16-200HV_Washer:18',#71623,
#71640,'19_ISO_7089_16-200HV_Washer:18');
#267=NEXT_ASSEMBLY_USAGE_OCCURRENCE('19_ISO_7089_16-200HV_Washer:19',
'19_ISO_7089_16-200HV_Washer:19','19_ISO_7089_16-200HV_Washer:19',#71623,
#71640,'19_ISO_7089_16-200HV_Washer:19');
#268=NEXT_ASSEMBLY_USAGE_OCCURRENCE('19_ISO_7089_16-200HV_Washer:20',
'19_ISO_7089_16-200HV_Washer:20','19_ISO_7089_16-200HV_Washer:20',#71623,
#71640,'19_ISO_7089_16-200HV_Washer:20');
#269=NEXT_ASSEMBLY_USAGE_OCCURRENCE('11_Pump_Operating_Handle_Arm:1',
'11_Pump_Operating_Handle_Arm:1','11_Pump_Operating_Handle_Arm:1',#71623,
#71641,'11_Pump_Operating_Handle_Arm:1');
#270=NEXT_ASSEMBLY_USAGE_OCCURRENCE(
'01_Upright_Column_L1440_RHS80x80x5:3',
'01_Upright_Column_L1440_RHS80x80x5:3',
'01_Upright_Column_L1440_RHS80x80x5:3',#71623,#71642,
'01_Upright_Column_L1440_RHS80x80x5:3');
#271=(
BOUNDED_CURVE()
B_SPLINE_CURVE(2,(#44561,#44562,#44563),.UNSPECIFIED.,.F.,.F.)
B_SPLINE_CURVE_WITH_KNOTS((3,3),(0.,0.186897942309885),.UNSPECIFIED.)
CURVE()
GEOMETRIC_REPRESENTATION_ITEM()
RATIONAL_B_SPLINE_CURVE((1.,1.00104922243968,1.00074449035823))
REPRESENTATION_ITEM('')
);
#272=(
BOUNDED_CURVE()
B_SPLINE_CURVE(2,(#44566,#44567,#44568),.UNSPECIFIED.,.F.,.F.)
B_SPLINE_CURVE_WITH_KNOTS((3,3),(0.102768382432289,0.289666324741965),
 .UNSPECIFIED.)
CURVE()
GEOMETRIC_REPRESENTATION_ITEM()
RATIONAL_B_SPLINE_CURVE((1.00074449035274,1.00104922243194,1.))
REPRESENTATION_ITEM('')
);
#273=(
BOUNDED_CURVE()
B_SPLINE_CURVE(2,(#44582,#44583,#44584),.UNSPECIFIED.,.F.,.F.)
B_SPLINE_CURVE_WITH_KNOTS((3,3),(0.,0.186897942309674),.UNSPECIFIED.)
CURVE()
GEOMETRIC_REPRESENTATION_ITEM()
RATIONAL_B_SPLINE_CURVE((1.,1.00104922243196,1.00074449035276))
REPRESENTATION_ITEM('')
);
#274=(
BOUNDED_CURVE()
B_SPLINE_CURVE(2,(#44587,#44588,#44589),.UNSPECIFIED.,.F.,.F.)
B_SPLINE_CURVE_WITH_KNOTS((3,3),(0.102768382432294,0.289666324741965),
 .UNSPECIFIED.)
CURVE()
GEOMETRIC_REPRESENTATION_ITEM()
RATIONAL_B_SPLINE_CURVE((1.00074449035267,1.00104922243184,1.))
REPRESENTATION_ITEM('')
);
#275=(
BOUNDED_CURVE()
B_SPLINE_CURVE(2,(#44603,#44604,#44605),.UNSPECIFIED.,.F.,.F.)
B_SPLINE_CURVE_WITH_KNOTS((3,3),(0.,0.186897942309901),.UNSPECIFIED.)
CURVE()
GEOMETRIC_REPRESENTATION_ITEM()
RATIONAL_B_SPLINE_CURVE((1.,1.00104922243998,1.00074449035845))
REPRESENTATION_ITEM('')
);
#276=(
BOUNDED_CURVE()
B_SPLINE_CURVE(2,(#44608,#44609,#44610),.UNSPECIFIED.,.F.,.F.)
B_SPLINE_CURVE_WITH_KNOTS((3,3),(0.102768382432298,0.289666324741965),
 .UNSPECIFIED.)
CURVE()
GEOMETRIC_REPRESENTATION_ITEM()
RATIONAL_B_SPLINE_CURVE((1.00074449035256,1.00104922243169,1.))
REPRESENTATION_ITEM('')
);
#277=(
BOUNDED_CURVE()
B_SPLINE_CURVE(2,(#44624,#44625,#44626),.UNSPECIFIED.,.F.,.F.)
B_SPLINE_CURVE_WITH_KNOTS((3,3),(0.,0.186897942309885),.UNSPECIFIED.)
CURVE()
GEOMETRIC_REPRESENTATION_ITEM()
RATIONAL_B_SPLINE_CURVE((1.,1.00104922243968,1.00074449035823))
REPRESENTATION_ITEM('')
);
#278=(
BOUNDED_CURVE()
B_SPLINE_CURVE(2,(#44629,#44630,#44631),.UNSPECIFIED.,.F.,.F.)
B_SPLINE_CURVE_WITH_KNOTS((3,3),(0.102768382432289,0.289666324741965),
 .UNSPECIFIED.)
CURVE()
GEOMETRIC_REPRESENTATION_ITEM()
RATIONAL_B_SPLINE_CURVE((1.00074449035274,1.00104922243194,1.))
REPRESENTATION_ITEM('')
);
#279=(
BOUNDED_CURVE()
B_SPLINE_CURVE(2,(#44645,#44646,#44647),.UNSPECIFIED.,.F.,.F.)
B_SPLINE_CURVE_WITH_KNOTS((3,3),(0.,0.186897942309671),.UNSPECIFIED.)
CURVE()
GEOMETRIC_REPRESENTATION_ITEM()
RATIONAL_B_SPLINE_CURVE((1.,1.00104922243187,1.00074449035269))
REPRESENTATION_ITEM('')
);
#280=(
BOUNDED_CURVE()
B_SPLINE_CURVE(2,(#44650,#44651,#44652),.UNSPECIFIED.,.F.,.F.)
B_SPLINE_CURVE_WITH_KNOTS((3,3),(0.102768382432295,0.289666324741964),
 .UNSPECIFIED.)
CURVE()
GEOMETRIC_REPRESENTATION_ITEM()
RATIONAL_B_SPLINE_CURVE((1.00074449035266,1.00104922243182,1.))
REPRESENTATION_ITEM('')
);
#281=(
BOUNDED_CURVE()
B_SPLINE_CURVE(2,(#44666,#44667,#44668),.UNSPECIFIED.,.F.,.F.)
B_SPLINE_CURVE_WITH_KNOTS((3,3),(0.,0.186897942309672),.UNSPECIFIED.)
CURVE()
GEOMETRIC_REPRESENTATION_ITEM()
RATIONAL_B_SPLINE_CURVE((1.,1.00104922243174,1.0007444903526))
REPRESENTATION_ITEM('')
);
#282=(
BOUNDED_CURVE()
B_SPLINE_CURVE(2,(#44671,#44672,#44673),.UNSPECIFIED.,.F.,.F.)
B_SPLINE_CURVE_WITH_KNOTS((3,3),(0.102768382432307,0.289666324741965),
 .UNSPECIFIED.)
CURVE()
GEOMETRIC_REPRESENTATION_ITEM()
RATIONAL_B_SPLINE_CURVE((1.00074449035222,1.00104922243121,1.))
REPRESENTATION_ITEM('')
);
#283=(
BOUNDED_CURVE()
B_SPLINE_CURVE(2,(#44689,#44690,#44691),.UNSPECIFIED.,.F.,.F.)
B_SPLINE_CURVE_WITH_KNOTS((3,3),(0.,0.186897942309665),.UNSPECIFIED.)
CURVE()
GEOMETRIC_REPRESENTATION_ITEM()
RATIONAL_B_SPLINE_CURVE((1.,1.00104922243153,1.00074449035245))
REPRESENTATION_ITEM('')
);
#284=(
BOUNDED_CURVE()
B_SPLINE_CURVE(2,(#44694,#44695,#44696),.UNSPECIFIED.,.F.,.F.)
B_SPLINE_CURVE_WITH_KNOTS((3,3),(0.102768382432301,0.289666324741966),
 .UNSPECIFIED.)
CURVE()
GEOMETRIC_REPRESENTATION_ITEM()
RATIONAL_B_SPLINE_CURVE((1.00074449035228,1.00104922243129,1.))
REPRESENTATION_ITEM('')
);
#285=(
BOUNDED_CURVE()
B_SPLINE_CURVE(2,(#44710,#44711,#44712),.UNSPECIFIED.,.F.,.F.)
B_SPLINE_CURVE_WITH_KNOTS((3,3),(0.,0.18689794230967),.UNSPECIFIED.)
CURVE()
GEOMETRIC_REPRESENTATION_ITEM()
RATIONAL_B_SPLINE_CURVE((1.,1.00104922243168,1.00074449035256))
REPRESENTATION_ITEM('')
);
#286=(
BOUNDED_CURVE()
B_SPLINE_CURVE(2,(#44715,#44716,#44717),.UNSPECIFIED.,.F.,.F.)
B_SPLINE_CURVE_WITH_KNOTS((3,3),(0.10276838243214,0.289666324741965),
 .UNSPECIFIED.)
CURVE()
GEOMETRIC_REPRESENTATION_ITEM()
RATIONAL_B_SPLINE_CURVE((1.00074449035625,1.00104922243688,1.))
REPRESENTATION_ITEM('')
);
#287=(
BOUNDED_CURVE()
B_SPLINE_CURVE(2,(#44731,#44732,#44733),.UNSPECIFIED.,.F.,.F.)
B_SPLINE_CURVE_WITH_KNOTS((3,3),(0.,0.186897942309663),.UNSPECIFIED.)
CURVE()
GEOMETRIC_REPRESENTATION_ITEM()
RATIONAL_B_SPLINE_CURVE((1.,1.00104922243133,1.00074449035231))
REPRESENTATION_ITEM('')
);
#288=(
BOUNDED_CURVE()
B_SPLINE_CURVE(2,(#44736,#44737,#44738),.UNSPECIFIED.,.F.,.F.)
B_SPLINE_CURVE_WITH_KNOTS((3,3),(0.102768382432299,0.289666324741965),
 .UNSPECIFIED.)
CURVE()
GEOMETRIC_REPRESENTATION_ITEM()
RATIONAL_B_SPLINE_CURVE((1.00074449035251,1.00104922243162,1.))
REPRESENTATION_ITEM('')
);
#289=(
BOUNDED_CURVE()
B_SPLINE_CURVE(2,(#44752,#44753,#44754),.UNSPECIFIED.,.F.,.F.)
B_SPLINE_CURVE_WITH_KNOTS((3,3),(0.,0.186897942309671),.UNSPECIFIED.)
CURVE()
GEOMETRIC_REPRESENTATION_ITEM()
RATIONAL_B_SPLINE_CURVE((1.,1.00104922243163,1.00074449035252))
REPRESENTATION_ITEM('')
);
#290=(
BOUNDED_CURVE()
B_SPLINE_CURVE(2,(#44757,#44758,#44759),.UNSPECIFIED.,.F.,.F.)
B_SPLINE_CURVE_WITH_KNOTS((3,3),(0.102768382432291,0.289666324741964),
 .UNSPECIFIED.)
CURVE()
GEOMETRIC_REPRESENTATION_ITEM()
RATIONAL_B_SPLINE_CURVE((1.00074449035272,1.00104922243191,1.))
REPRESENTATION_ITEM('')
);
#291=(
BOUNDED_CURVE()
B_SPLINE_CURVE(2,(#44773,#44774,#44775),.UNSPECIFIED.,.F.,.F.)
B_SPLINE_CURVE_WITH_KNOTS((3,3),(0.,0.186897942309668),.UNSPECIFIED.)
CURVE()
GEOMETRIC_REPRESENTATION_ITEM()
RATIONAL_B_SPLINE_CURVE((1.,1.00104922243145,1.00074449035239))
REPRESENTATION_ITEM('')
);
#292=(
BOUNDED_CURVE()
B_SPLINE_CURVE(2,(#44778,#44779,#44780),.UNSPECIFIED.,.F.,.F.)
B_SPLINE_CURVE_WITH_KNOTS((3,3),(0.102768382432079,0.289666324741965),
 .UNSPECIFIED.)
CURVE()
GEOMETRIC_REPRESENTATION_ITEM()
RATIONAL_B_SPLINE_CURVE((1.00074449035827,1.00104922243974,1.))
REPRESENTATION_ITEM('')
);
#293=(
BOUNDED_CURVE()
B_SPLINE_CURVE(2,(#44794,#44795,#44796),.UNSPECIFIED.,.F.,.F.)
B_SPLINE_CURVE_WITH_KNOTS((3,3),(0.,0.186897942309668),.UNSPECIFIED.)
CURVE()
GEOMETRIC_REPRESENTATION_ITEM()
RATIONAL_B_SPLINE_CURVE((1.,1.00104922243171,1.00074449035258))
REPRESENTATION_ITEM('')
);
#294=(
BOUNDED_CURVE()
B_SPLINE_CURVE(2,(#44799,#44800,#44801),.UNSPECIFIED.,.F.,.F.)
B_SPLINE_CURVE_WITH_KNOTS((3,3),(0.102768382432086,0.289666324741965),
 .UNSPECIFIED.)
CURVE()
GEOMETRIC_REPRESENTATION_ITEM()
RATIONAL_B_SPLINE_CURVE((1.00074449035837,1.00104922243988,1.))
REPRESENTATION_ITEM('')
);
#295=(
BOUNDED_CURVE()
B_SPLINE_CURVE(2,(#44815,#44816,#44817),.UNSPECIFIED.,.F.,.F.)
B_SPLINE_CURVE_WITH_KNOTS((3,3),(0.,0.186897942309671),.UNSPECIFIED.)
CURVE()
GEOMETRIC_REPRESENTATION_ITEM()
RATIONAL_B_SPLINE_CURVE((1.,1.00104922243187,1.00074449035269))
REPRESENTATION_ITEM('')
);
#296=(
BOUNDED_CURVE()
B_SPLINE_CURVE(2,(#44820,#44821,#44822),.UNSPECIFIED.,.F.,.F.)
B_SPLINE_CURVE_WITH_KNOTS((3,3),(0.102768382432293,0.289666324741965),
 .UNSPECIFIED.)
CURVE()
GEOMETRIC_REPRESENTATION_ITEM()
RATIONAL_B_SPLINE_CURVE((1.0007444903527,1.00104922243188,1.))
REPRESENTATION_ITEM('')
);
#297=(
BOUNDED_CURVE()
B_SPLINE_CURVE(2,(#44836,#44837,#44838),.UNSPECIFIED.,.F.,.F.)
B_SPLINE_CURVE_WITH_KNOTS((3,3),(0.,0.186897942309669),.UNSPECIFIED.)
CURVE()
GEOMETRIC_REPRESENTATION_ITEM()
RATIONAL_B_SPLINE_CURVE((1.,1.00104922243157,1.00074449035248))
REPRESENTATION_ITEM('')
);
#298=(
BOUNDED_CURVE()
B_SPLINE_CURVE(2,(#44841,#44842,#44843),.UNSPECIFIED.,.F.,.F.)
B_SPLINE_CURVE_WITH_KNOTS((3,3),(0.102768382432292,0.289666324741965),
 .UNSPECIFIED.)
CURVE()
GEOMETRIC_REPRESENTATION_ITEM()
RATIONAL_B_SPLINE_CURVE((1.00074449035271,1.00104922243189,1.))
REPRESENTATION_ITEM('')
);
#299=(
BOUNDED_CURVE()
B_SPLINE_CURVE(2,(#44857,#44858,#44859),.UNSPECIFIED.,.F.,.F.)
B_SPLINE_CURVE_WITH_KNOTS((3,3),(0.,0.186897942309658),.UNSPECIFIED.)
CURVE()
GEOMETRIC_REPRESENTATION_ITEM()
RATIONAL_B_SPLINE_CURVE((1.,1.00104922243123,1.00074449035224))
REPRESENTATION_ITEM('')
);
#300=(
BOUNDED_CURVE()
B_SPLINE_CURVE(2,(#44862,#44863,#44864),.UNSPECIFIED.,.F.,.F.)
B_SPLINE_CURVE_WITH_KNOTS((3,3),(0.102768382432307,0.289666324741965),
 .UNSPECIFIED.)
CURVE()
GEOMETRIC_REPRESENTATION_ITEM()
RATIONAL_B_SPLINE_CURVE((1.00074449035222,1.00104922243121,1.))
REPRESENTATION_ITEM('')
);
#301=(
BOUNDED_CURVE()
B_SPLINE_CURVE(2,(#44878,#44879,#44880),.UNSPECIFIED.,.F.,.F.)
B_SPLINE_CURVE_WITH_KNOTS((3,3),(0.,0.186897942309668),.UNSPECIFIED.)
CURVE()
GEOMETRIC_REPRESENTATION_ITEM()
RATIONAL_B_SPLINE_CURVE((1.,1.00104922243153,1.00074449035245))
REPRESENTATION_ITEM('')
);
#302=(
BOUNDED_CURVE()
B_SPLINE_CURVE(2,(#44883,#44884,#44885),.UNSPECIFIED.,.F.,.F.)
B_SPLINE_CURVE_WITH_KNOTS((3,3),(0.102768382432315,0.289666324741965),
 .UNSPECIFIED.)
CURVE()
GEOMETRIC_REPRESENTATION_ITEM()
RATIONAL_B_SPLINE_CURVE((1.00074449035217,1.00104922243113,1.))
REPRESENTATION_ITEM('')
);
#303=(
BOUNDED_CURVE()
B_SPLINE_CURVE(2,(#44899,#44900,#44901),.UNSPECIFIED.,.F.,.F.)
B_SPLINE_CURVE_WITH_KNOTS((3,3),(0.,0.186897942309684),.UNSPECIFIED.)
CURVE()
GEOMETRIC_REPRESENTATION_ITEM()
RATIONAL_B_SPLINE_CURVE((1.,1.00104922243195,1.00074449035275))
REPRESENTATION_ITEM('')
);
#304=(
BOUNDED_CURVE()
B_SPLINE_CURVE(2,(#44904,#44905,#44906),.UNSPECIFIED.,.F.,.F.)
B_SPLINE_CURVE_WITH_KNOTS((3,3),(0.102768382432288,0.289666324741966),
 .UNSPECIFIED.)
CURVE()
GEOMETRIC_REPRESENTATION_ITEM()
RATIONAL_B_SPLINE_CURVE((1.00074449035274,1.00104922243194,1.))
REPRESENTATION_ITEM('')
);
#305=(
BOUNDED_CURVE()
B_SPLINE_CURVE(2,(#44920,#44921,#44922),.UNSPECIFIED.,.F.,.F.)
B_SPLINE_CURVE_WITH_KNOTS((3,3),(0.,0.186897942309664),.UNSPECIFIED.)
CURVE()
GEOMETRIC_REPRESENTATION_ITEM()
RATIONAL_B_SPLINE_CURVE((1.,1.00104922243129,1.00074449035228))
REPRESENTATION_ITEM('')
);
#306=(
BOUNDED_CURVE()
B_SPLINE_CURVE(2,(#44925,#44926,#44927),.UNSPECIFIED.,.F.,.F.)
B_SPLINE_CURVE_WITH_KNOTS((3,3),(0.102768382432294,0.289666324741965),
 .UNSPECIFIED.)
CURVE()
GEOMETRIC_REPRESENTATION_ITEM()
RATIONAL_B_SPLINE_CURVE((1.00074449035262,1.00104922243177,1.))
REPRESENTATION_ITEM('')
);
#307=(
BOUNDED_CURVE()
B_SPLINE_CURVE(2,(#44941,#44942,#44943),.UNSPECIFIED.,.F.,.F.)
B_SPLINE_CURVE_WITH_KNOTS((3,3),(0.,0.186897942309668),.UNSPECIFIED.)
CURVE()
GEOMETRIC_REPRESENTATION_ITEM()
RATIONAL_B_SPLINE_CURVE((1.,1.00104922243147,1.00074449035241))
REPRESENTATION_ITEM('')
);
#308=(
BOUNDED_CURVE()
B_SPLINE_CURVE(2,(#44946,#44947,#44948),.UNSPECIFIED.,.F.,.F.)
B_SPLINE_CURVE_WITH_KNOTS((3,3),(0.102768382432086,0.289666324741965),
 .UNSPECIFIED.)
CURVE()
GEOMETRIC_REPRESENTATION_ITEM()
RATIONAL_B_SPLINE_CURVE((1.00074449035837,1.00104922243988,1.))
REPRESENTATION_ITEM('')
);
#309=(
BOUNDED_CURVE()
B_SPLINE_CURVE(2,(#44962,#44963,#44964),.UNSPECIFIED.,.F.,.F.)
B_SPLINE_CURVE_WITH_KNOTS((3,3),(0.,0.186897942309669),.UNSPECIFIED.)
CURVE()
GEOMETRIC_REPRESENTATION_ITEM()
RATIONAL_B_SPLINE_CURVE((1.,1.00104922243168,1.00074449035256))
REPRESENTATION_ITEM('')
);
#310=(
BOUNDED_CURVE()
B_SPLINE_CURVE(2,(#44967,#44968,#44969),.UNSPECIFIED.,.F.,.F.)
B_SPLINE_CURVE_WITH_KNOTS((3,3),(0.102768382432305,0.289666324741966),
 .UNSPECIFIED.)
CURVE()
GEOMETRIC_REPRESENTATION_ITEM()
RATIONAL_B_SPLINE_CURVE((1.0007444903522,1.00104922243117,1.))
REPRESENTATION_ITEM('')
);
#311=(
BOUNDED_CURVE()
B_SPLINE_CURVE(2,(#44983,#44984,#44985),.UNSPECIFIED.,.F.,.F.)
B_SPLINE_CURVE_WITH_KNOTS((3,3),(0.,0.186897942309671),.UNSPECIFIED.)
CURVE()
GEOMETRIC_REPRESENTATION_ITEM()
RATIONAL_B_SPLINE_CURVE((1.,1.00104922243178,1.00074449035262))
REPRESENTATION_ITEM('')
);
#312=(
BOUNDED_CURVE()
B_SPLINE_CURVE(2,(#44988,#44989,#44990),.UNSPECIFIED.,.F.,.F.)
B_SPLINE_CURVE_WITH_KNOTS((3,3),(0.102768382432293,0.289666324741965),
 .UNSPECIFIED.)
CURVE()
GEOMETRIC_REPRESENTATION_ITEM()
RATIONAL_B_SPLINE_CURVE((1.00074449035232,1.00104922243135,1.))
REPRESENTATION_ITEM('')
);
#313=(
BOUNDED_CURVE()
B_SPLINE_CURVE(2,(#45004,#45005,#45006),.UNSPECIFIED.,.F.,.F.)
B_SPLINE_CURVE_WITH_KNOTS((3,3),(0.,0.186897942309666),.UNSPECIFIED.)
CURVE()
GEOMETRIC_REPRESENTATION_ITEM()
RATIONAL_B_SPLINE_CURVE((1.,1.00104922243158,1.00074449035248))
REPRESENTATION_ITEM('')
);
#314=(
BOUNDED_CURVE()
B_SPLINE_CURVE(2,(#45009,#45010,#45011),.UNSPECIFIED.,.F.,.F.)
B_SPLINE_CURVE_WITH_KNOTS((3,3),(0.102768382432303,0.289666324741966),
 .UNSPECIFIED.)
CURVE()
GEOMETRIC_REPRESENTATION_ITEM()
RATIONAL_B_SPLINE_CURVE((1.00074449035238,1.00104922243143,1.))
REPRESENTATION_ITEM('')
);
#315=(
BOUNDED_CURVE()
B_SPLINE_CURVE(2,(#45025,#45026,#45027),.UNSPECIFIED.,.F.,.F.)
B_SPLINE_CURVE_WITH_KNOTS((3,3),(0.,0.186897942309666),.UNSPECIFIED.)
CURVE()
GEOMETRIC_REPRESENTATION_ITEM()
RATIONAL_B_SPLINE_CURVE((1.,1.00104922243159,1.00074449035249))
REPRESENTATION_ITEM('')
);
#316=(
BOUNDED_CURVE()
B_SPLINE_CURVE(2,(#45030,#45031,#45032),.UNSPECIFIED.,.F.,.F.)
B_SPLINE_CURVE_WITH_KNOTS((3,3),(0.102768382432302,0.289666324741967),
 .UNSPECIFIED.)
CURVE()
GEOMETRIC_REPRESENTATION_ITEM()
RATIONAL_B_SPLINE_CURVE((1.00074449035229,1.0010492224313,1.))
REPRESENTATION_ITEM('')
);
#317=(
BOUNDED_CURVE()
B_SPLINE_CURVE(2,(#45046,#45047,#45048),.UNSPECIFIED.,.F.,.F.)
B_SPLINE_CURVE_WITH_KNOTS((3,3),(0.,0.186897942309671),.UNSPECIFIED.)
CURVE()
GEOMETRIC_REPRESENTATION_ITEM()
RATIONAL_B_SPLINE_CURVE((1.,1.00104922243168,1.00074449035256))
REPRESENTATION_ITEM('')
);
#318=(
BOUNDED_CURVE()
B_SPLINE_CURVE(2,(#45051,#45052,#45053),.UNSPECIFIED.,.F.,.F.)
B_SPLINE_CURVE_WITH_KNOTS((3,3),(0.102768382432289,0.289666324741963),
 .UNSPECIFIED.)
CURVE()
GEOMETRIC_REPRESENTATION_ITEM()
RATIONAL_B_SPLINE_CURVE((1.00074449035275,1.00104922243195,1.))
REPRESENTATION_ITEM('')
);
#319=(
BOUNDED_CURVE()
B_SPLINE_CURVE(2,(#47148,#47149,#47150),.UNSPECIFIED.,.F.,.F.)
B_SPLINE_CURVE_WITH_KNOTS((3,3),(0.0512618960218088,0.239747982802954),
 .UNSPECIFIED.)
CURVE()
GEOMETRIC_REPRESENTATION_ITEM()
RATIONAL_B_SPLINE_CURVE((1.0006680999084,1.00156232618943,1.))
REPRESENTATION_ITEM('')
);
#320=(
BOUNDED_CURVE()
B_SPLINE_CURVE(2,(#47162,#47163,#47164),.UNSPECIFIED.,.F.,.F.)
B_SPLINE_CURVE_WITH_KNOTS((3,3),(0.,0.18848608678106),.UNSPECIFIED.)
CURVE()
GEOMETRIC_REPRESENTATION_ITEM()
RATIONAL_B_SPLINE_CURVE((1.,1.0015623261938,1.00066809991027))
REPRESENTATION_ITEM('')
);
#321=(
BOUNDED_CURVE()
B_SPLINE_CURVE(2,(#47169,#47170,#47171),.UNSPECIFIED.,.F.,.F.)
B_SPLINE_CURVE_WITH_KNOTS((3,3),(0.0512618960217405,0.239747982802953),
 .UNSPECIFIED.)
CURVE()
GEOMETRIC_REPRESENTATION_ITEM()
RATIONAL_B_SPLINE_CURVE((1.00066809990968,1.00156232619242,1.))
REPRESENTATION_ITEM('')
);
#322=(
BOUNDED_CURVE()
B_SPLINE_CURVE(2,(#47183,#47184,#47185),.UNSPECIFIED.,.F.,.F.)
B_SPLINE_CURVE_WITH_KNOTS((3,3),(0.,0.188486086781626),.UNSPECIFIED.)
CURVE()
GEOMETRIC_REPRESENTATION_ITEM()
RATIONAL_B_SPLINE_CURVE((1.,1.00156232620375,1.00066809991451))
REPRESENTATION_ITEM('')
);
#323=(
BOUNDED_CURVE()
B_SPLINE_CURVE(2,(#47190,#47191,#47192),.UNSPECIFIED.,.F.,.F.)
B_SPLINE_CURVE_WITH_KNOTS((3,3),(0.051261896021783,0.239747982802949),
 .UNSPECIFIED.)
CURVE()
GEOMETRIC_REPRESENTATION_ITEM()
RATIONAL_B_SPLINE_CURVE((1.0006680999091,1.00156232619108,1.))
REPRESENTATION_ITEM('')
);
#324=(
BOUNDED_CURVE()
B_SPLINE_CURVE(2,(#47204,#47205,#47206),.UNSPECIFIED.,.F.,.F.)
B_SPLINE_CURVE_WITH_KNOTS((3,3),(0.,0.188486086780641),.UNSPECIFIED.)
CURVE()
GEOMETRIC_REPRESENTATION_ITEM()
RATIONAL_B_SPLINE_CURVE((1.,1.00156232617076,1.00066809990042))
REPRESENTATION_ITEM('')
);
#325=(
BOUNDED_CURVE()
B_SPLINE_CURVE(2,(#47211,#47212,#47213),.UNSPECIFIED.,.F.,.F.)
B_SPLINE_CURVE_WITH_KNOTS((3,3),(0.0512618960212928,0.239747982802966),
 .UNSPECIFIED.)
CURVE()
GEOMETRIC_REPRESENTATION_ITEM()
RATIONAL_B_SPLINE_CURVE((1.00066809991313,1.0015623262005,1.))
REPRESENTATION_ITEM('')
);
#326=(
BOUNDED_CURVE()
B_SPLINE_CURVE(2,(#47225,#47226,#47227),.UNSPECIFIED.,.F.,.F.)
B_SPLINE_CURVE_WITH_KNOTS((3,3),(0.,0.18848608678103),.UNSPECIFIED.)
CURVE()
GEOMETRIC_REPRESENTATION_ITEM()
RATIONAL_B_SPLINE_CURVE((1.,1.00156232618489,1.00066809990646))
REPRESENTATION_ITEM('')
);
#327=(
BOUNDED_CURVE()
B_SPLINE_CURVE(2,(#47232,#47233,#47234),.UNSPECIFIED.,.F.,.F.)
B_SPLINE_CURVE_WITH_KNOTS((3,3),(0.0512618960214512,0.239747982802948),
 .UNSPECIFIED.)
CURVE()
GEOMETRIC_REPRESENTATION_ITEM()
RATIONAL_B_SPLINE_CURVE((1.00066809991422,1.00156232620306,1.))
REPRESENTATION_ITEM('')
);
#328=(
BOUNDED_CURVE()
B_SPLINE_CURVE(2,(#47246,#47247,#47248),.UNSPECIFIED.,.F.,.F.)
B_SPLINE_CURVE_WITH_KNOTS((3,3),(0.,0.188486086781497),.UNSPECIFIED.)
CURVE()
GEOMETRIC_REPRESENTATION_ITEM()
RATIONAL_B_SPLINE_CURVE((1.,1.00156232620306,1.00066809991422))
REPRESENTATION_ITEM('')
);
#329=(
BOUNDED_CURVE()
B_SPLINE_CURVE(2,(#47253,#47254,#47255),.UNSPECIFIED.,.F.,.F.)
B_SPLINE_CURVE_WITH_KNOTS((3,3),(0.0512618960218087,0.239747982802954),
 .UNSPECIFIED.)
CURVE()
GEOMETRIC_REPRESENTATION_ITEM()
RATIONAL_B_SPLINE_CURVE((1.0006680999084,1.00156232618943,1.))
REPRESENTATION_ITEM('')
);
#330=(
BOUNDED_CURVE()
B_SPLINE_CURVE(2,(#47267,#47268,#47269),.UNSPECIFIED.,.F.,.F.)
B_SPLINE_CURVE_WITH_KNOTS((3,3),(0.,0.188486086780909),.UNSPECIFIED.)
CURVE()
GEOMETRIC_REPRESENTATION_ITEM()
RATIONAL_B_SPLINE_CURVE((1.,1.00156232618876,1.00066809990812))
REPRESENTATION_ITEM('')
);
#331=(
BOUNDED_CURVE()
B_SPLINE_CURVE(2,(#47274,#47275,#47276),.UNSPECIFIED.,.F.,.F.)
B_SPLINE_CURVE_WITH_KNOTS((3,3),(0.0512618960214397,0.239747982802953),
 .UNSPECIFIED.)
CURVE()
GEOMETRIC_REPRESENTATION_ITEM()
RATIONAL_B_SPLINE_CURVE((1.00066809991433,1.00156232620331,1.))
REPRESENTATION_ITEM('')
);
#332=(
BOUNDED_CURVE()
B_SPLINE_CURVE(2,(#47288,#47289,#47290),.UNSPECIFIED.,.F.,.F.)
B_SPLINE_CURVE_WITH_KNOTS((3,3),(0.,0.188486086781649),.UNSPECIFIED.)
CURVE()
GEOMETRIC_REPRESENTATION_ITEM()
RATIONAL_B_SPLINE_CURVE((1.,1.00156232620001,1.00066809991291))
REPRESENTATION_ITEM('')
);
#333=(
BOUNDED_CURVE()
B_SPLINE_CURVE(2,(#47295,#47296,#47297),.UNSPECIFIED.,.F.,.F.)
B_SPLINE_CURVE_WITH_KNOTS((3,3),(0.0512618960219227,0.239747982802949),
 .UNSPECIFIED.)
CURVE()
GEOMETRIC_REPRESENTATION_ITEM()
RATIONAL_B_SPLINE_CURVE((1.00066809990695,1.00156232618604,1.))
REPRESENTATION_ITEM('')
);
#334=(
BOUNDED_CURVE()
B_SPLINE_CURVE(2,(#47309,#47310,#47311),.UNSPECIFIED.,.F.,.F.)
B_SPLINE_CURVE_WITH_KNOTS((3,3),(0.,0.188486086780641),.UNSPECIFIED.)
CURVE()
GEOMETRIC_REPRESENTATION_ITEM()
RATIONAL_B_SPLINE_CURVE((1.,1.00156232617076,1.00066809990042))
REPRESENTATION_ITEM('')
);
#335=(
BOUNDED_CURVE()
B_SPLINE_CURVE(2,(#47316,#47317,#47318),.UNSPECIFIED.,.F.,.F.)
B_SPLINE_CURVE_WITH_KNOTS((3,3),(0.0512618960215005,0.239747982802966),
 .UNSPECIFIED.)
CURVE()
GEOMETRIC_REPRESENTATION_ITEM()
RATIONAL_B_SPLINE_CURVE((1.00066809990987,1.00156232619288,1.))
REPRESENTATION_ITEM('')
);
#336=(
BOUNDED_CURVE()
B_SPLINE_CURVE(2,(#47330,#47331,#47332),.UNSPECIFIED.,.F.,.F.)
B_SPLINE_CURVE_WITH_KNOTS((3,3),(0.,0.188486086781019),.UNSPECIFIED.)
CURVE()
GEOMETRIC_REPRESENTATION_ITEM()
RATIONAL_B_SPLINE_CURVE((1.,1.00156232618454,1.00066809990631))
REPRESENTATION_ITEM('')
);
#337=(
BOUNDED_CURVE()
B_SPLINE_CURVE(2,(#47337,#47338,#47339),.UNSPECIFIED.,.F.,.F.)
B_SPLINE_CURVE_WITH_KNOTS((3,3),(0.0512618960218745,0.239747982802939),
 .UNSPECIFIED.)
CURVE()
GEOMETRIC_REPRESENTATION_ITEM()
RATIONAL_B_SPLINE_CURVE((1.00066809991027,1.0015623261938,1.))
REPRESENTATION_ITEM('')
);
#338=(
BOUNDED_CURVE()
B_SPLINE_CURVE(2,(#47351,#47352,#47353),.UNSPECIFIED.,.F.,.F.)
B_SPLINE_CURVE_WITH_KNOTS((3,3),(0.,0.188486086781156),.UNSPECIFIED.)
CURVE()
GEOMETRIC_REPRESENTATION_ITEM()
RATIONAL_B_SPLINE_CURVE((1.,1.00156232618832,1.00066809990792))
REPRESENTATION_ITEM('')
);
#339=(
BOUNDED_CURVE()
B_SPLINE_CURVE(2,(#47358,#47359,#47360),.UNSPECIFIED.,.F.,.F.)
B_SPLINE_CURVE_WITH_KNOTS((3,3),(0.0512618960213807,0.239747982802952),
 .UNSPECIFIED.)
CURVE()
GEOMETRIC_REPRESENTATION_ITEM()
RATIONAL_B_SPLINE_CURVE((1.00066809991545,1.00156232620592,1.))
REPRESENTATION_ITEM('')
);
#340=(
BOUNDED_CURVE()
B_SPLINE_CURVE(2,(#47372,#47373,#47374),.UNSPECIFIED.,.F.,.F.)
B_SPLINE_CURVE_WITH_KNOTS((3,3),(0.,0.188486086781477),.UNSPECIFIED.)
CURVE()
GEOMETRIC_REPRESENTATION_ITEM()
RATIONAL_B_SPLINE_CURVE((1.,1.0015623262088,1.00066809991668))
REPRESENTATION_ITEM('')
);
#341=(
BOUNDED_CURVE()
B_SPLINE_CURVE(2,(#47379,#47380,#47381),.UNSPECIFIED.,.F.,.F.)
B_SPLINE_CURVE_WITH_KNOTS((3,3),(0.0512618960223282,0.239747982802951),
 .UNSPECIFIED.)
CURVE()
GEOMETRIC_REPRESENTATION_ITEM()
RATIONAL_B_SPLINE_CURVE((1.00066809990016,1.00156232617014,1.))
REPRESENTATION_ITEM('')
);
#342=(
BOUNDED_CURVE()
B_SPLINE_CURVE(2,(#47393,#47394,#47395),.UNSPECIFIED.,.F.,.F.)
B_SPLINE_CURVE_WITH_KNOTS((3,3),(0.,0.188486086781308),.UNSPECIFIED.)
CURVE()
GEOMETRIC_REPRESENTATION_ITEM()
RATIONAL_B_SPLINE_CURVE((1.,1.00156232619586,1.00066809991115))
REPRESENTATION_ITEM('')
);
#343=(
BOUNDED_CURVE()
B_SPLINE_CURVE(2,(#47400,#47401,#47402),.UNSPECIFIED.,.F.,.F.)
B_SPLINE_CURVE_WITH_KNOTS((3,3),(0.051261896021939,0.239747982802949),
 .UNSPECIFIED.)
CURVE()
GEOMETRIC_REPRESENTATION_ITEM()
RATIONAL_B_SPLINE_CURVE((1.00066809990618,1.00156232618425,1.))
REPRESENTATION_ITEM('')
);
#344=(
BOUNDED_CURVE()
B_SPLINE_CURVE(2,(#47414,#47415,#47416),.UNSPECIFIED.,.F.,.F.)
B_SPLINE_CURVE_WITH_KNOTS((3,3),(0.,0.188486086781416),.UNSPECIFIED.)
CURVE()
GEOMETRIC_REPRESENTATION_ITEM()
RATIONAL_B_SPLINE_CURVE((1.,1.0015623261913,1.0006680999092))
REPRESENTATION_ITEM('')
);
#345=(
BOUNDED_CURVE()
B_SPLINE_CURVE(2,(#47421,#47422,#47423),.UNSPECIFIED.,.F.,.F.)
B_SPLINE_CURVE_WITH_KNOTS((3,3),(0.0512618960214561,0.239747982802948),
 .UNSPECIFIED.)
CURVE()
GEOMETRIC_REPRESENTATION_ITEM()
RATIONAL_B_SPLINE_CURVE((1.00066809991424,1.00156232620311,1.))
REPRESENTATION_ITEM('')
);
#346=(
BOUNDED_CURVE()
B_SPLINE_CURVE(2,(#47437,#47438,#47439),.UNSPECIFIED.,.F.,.F.)
B_SPLINE_CURVE_WITH_KNOTS((3,3),(0.,0.188486086781106),.UNSPECIFIED.)
CURVE()
GEOMETRIC_REPRESENTATION_ITEM()
RATIONAL_B_SPLINE_CURVE((1.,1.00156232618923,1.00066809990831))
REPRESENTATION_ITEM('')
);
#347=(
BOUNDED_CURVE()
B_SPLINE_CURVE(2,(#47444,#47445,#47446),.UNSPECIFIED.,.F.,.F.)
B_SPLINE_CURVE_WITH_KNOTS((3,3),(0.0512618960218789,0.239747982802938),
 .UNSPECIFIED.)
CURVE()
GEOMETRIC_REPRESENTATION_ITEM()
RATIONAL_B_SPLINE_CURVE((1.00066809991027,1.0015623261938,1.))
REPRESENTATION_ITEM('')
);
#348=(
BOUNDED_CURVE()
B_SPLINE_CURVE(2,(#47458,#47459,#47460),.UNSPECIFIED.,.F.,.F.)
B_SPLINE_CURVE_WITH_KNOTS((3,3),(0.,0.188486086781156),.UNSPECIFIED.)
CURVE()
GEOMETRIC_REPRESENTATION_ITEM()
RATIONAL_B_SPLINE_CURVE((1.,1.00156232618832,1.00066809990792))
REPRESENTATION_ITEM('')
);
#349=(
BOUNDED_CURVE()
B_SPLINE_CURVE(2,(#47465,#47466,#47467),.UNSPECIFIED.,.F.,.F.)
B_SPLINE_CURVE_WITH_KNOTS((3,3),(0.0512618960211266,0.239747982802957),
 .UNSPECIFIED.)
CURVE()
GEOMETRIC_REPRESENTATION_ITEM()
RATIONAL_B_SPLINE_CURVE((1.00066809991756,1.00156232621087,1.))
REPRESENTATION_ITEM('')
);
#350=(
BOUNDED_CURVE()
B_SPLINE_CURVE(2,(#47479,#47480,#47481),.UNSPECIFIED.,.F.,.F.)
B_SPLINE_CURVE_WITH_KNOTS((3,3),(0.,0.188486086781475),.UNSPECIFIED.)
CURVE()
GEOMETRIC_REPRESENTATION_ITEM()
RATIONAL_B_SPLINE_CURVE((1.,1.0015623262088,1.00066809991668))
REPRESENTATION_ITEM('')
);
#351=(
BOUNDED_CURVE()
B_SPLINE_CURVE(2,(#47486,#47487,#47488),.UNSPECIFIED.,.F.,.F.)
B_SPLINE_CURVE_WITH_KNOTS((3,3),(0.0512618960222505,0.239747982802951),
 .UNSPECIFIED.)
CURVE()
GEOMETRIC_REPRESENTATION_ITEM()
RATIONAL_B_SPLINE_CURVE((1.00066809990131,1.00156232617284,1.))
REPRESENTATION_ITEM('')
);
#352=(
BOUNDED_CURVE()
B_SPLINE_CURVE(2,(#47500,#47501,#47502),.UNSPECIFIED.,.F.,.F.)
B_SPLINE_CURVE_WITH_KNOTS((3,3),(0.,0.188486086781171),.UNSPECIFIED.)
CURVE()
GEOMETRIC_REPRESENTATION_ITEM()
RATIONAL_B_SPLINE_CURVE((1.,1.00156232619143,1.00066809990925))
REPRESENTATION_ITEM('')
);
#353=(
BOUNDED_CURVE()
B_SPLINE_CURVE(2,(#47507,#47508,#47509),.UNSPECIFIED.,.F.,.F.)
B_SPLINE_CURVE_WITH_KNOTS((3,3),(0.0512618960219306,0.239747982802949),
 .UNSPECIFIED.)
CURVE()
GEOMETRIC_REPRESENTATION_ITEM()
RATIONAL_B_SPLINE_CURVE((1.00066809990631,1.00156232618454,1.))
REPRESENTATION_ITEM('')
);
#354=(
BOUNDED_CURVE()
B_SPLINE_CURVE(2,(#47521,#47522,#47523),.UNSPECIFIED.,.F.,.F.)
B_SPLINE_CURVE_WITH_KNOTS((3,3),(0.,0.188486086781674),.UNSPECIFIED.)
CURVE()
GEOMETRIC_REPRESENTATION_ITEM()
RATIONAL_B_SPLINE_CURVE((1.,1.0015623262005,1.00066809991312))
REPRESENTATION_ITEM('')
);
#355=(
BOUNDED_CURVE()
B_SPLINE_CURVE(2,(#70524,#70525,#70526),.UNSPECIFIED.,.F.,.F.)
B_SPLINE_CURVE_WITH_KNOTS((3,3),(0.0830692064483412,1.5163968327409),
 .UNSPECIFIED.)
CURVE()
GEOMETRIC_REPRESENTATION_ITEM()
RATIONAL_B_SPLINE_CURVE((1.01933756729741,1.17702963774851,1.01933756729741))
REPRESENTATION_ITEM('')
);
#356=(
BOUNDED_CURVE()
B_SPLINE_CURVE(2,(#70528,#70529,#70530),.UNSPECIFIED.,.F.,.F.)
B_SPLINE_CURVE_WITH_KNOTS((3,3),(0.0830692064483407,1.5163968327409),
 .UNSPECIFIED.)
CURVE()
GEOMETRIC_REPRESENTATION_ITEM()
RATIONAL_B_SPLINE_CURVE((1.01933756729741,1.17702963774851,1.01933756729741))
REPRESENTATION_ITEM('')
);
#357=(
BOUNDED_CURVE()
B_SPLINE_CURVE(2,(#70532,#70533,#70534),.UNSPECIFIED.,.F.,.F.)
B_SPLINE_CURVE_WITH_KNOTS((3,3),(0.0830692064483414,1.5163968327409),
 .UNSPECIFIED.)
CURVE()
GEOMETRIC_REPRESENTATION_ITEM()
RATIONAL_B_SPLINE_CURVE((1.01933756729741,1.17702963774851,1.01933756729741))
REPRESENTATION_ITEM('')
);
#358=(
BOUNDED_CURVE()
B_SPLINE_CURVE(2,(#70536,#70537,#70538),.UNSPECIFIED.,.F.,.F.)
B_SPLINE_CURVE_WITH_KNOTS((3,3),(0.0830692064483412,1.5163968327409),
 .UNSPECIFIED.)
CURVE()
GEOMETRIC_REPRESENTATION_ITEM()
RATIONAL_B_SPLINE_CURVE((1.01933756729741,1.17702963774851,1.01933756729741))
REPRESENTATION_ITEM('')
);
#359=(
BOUNDED_CURVE()
B_SPLINE_CURVE(2,(#70540,#70541,#70542),.UNSPECIFIED.,.F.,.F.)
B_SPLINE_CURVE_WITH_KNOTS((3,3),(0.799733019594622,1.5163968327409),
 .UNSPECIFIED.)
CURVE()
GEOMETRIC_REPRESENTATION_ITEM()
RATIONAL_B_SPLINE_CURVE((1.09818360252296,1.09818360252296,1.01933756729741))
REPRESENTATION_ITEM('')
);
#360=(
BOUNDED_CURVE()
B_SPLINE_CURVE(2,(#70547,#70548,#70549),.UNSPECIFIED.,.F.,.F.)
B_SPLINE_CURVE_WITH_KNOTS((3,3),(0.083069206448341,0.799733019594622),
 .UNSPECIFIED.)
CURVE()
GEOMETRIC_REPRESENTATION_ITEM()
RATIONAL_B_SPLINE_CURVE((1.01933756729741,1.09818360252296,1.09818360252296))
REPRESENTATION_ITEM('')
);
#361=(
BOUNDED_CURVE()
B_SPLINE_CURVE(2,(#70550,#70551,#70552),.UNSPECIFIED.,.F.,.F.)
B_SPLINE_CURVE_WITH_KNOTS((3,3),(0.0830692064483408,1.5163968327409),
 .UNSPECIFIED.)
CURVE()
GEOMETRIC_REPRESENTATION_ITEM()
RATIONAL_B_SPLINE_CURVE((1.01933756729741,1.17702963774851,1.01933756729741))
REPRESENTATION_ITEM('')
);
#362=(
BOUNDED_CURVE()
B_SPLINE_CURVE(2,(#70596,#70597,#70598),.UNSPECIFIED.,.F.,.F.)
B_SPLINE_CURVE_WITH_KNOTS((3,3),(0.083069206448341,0.799733019594622),
 .UNSPECIFIED.)
CURVE()
GEOMETRIC_REPRESENTATION_ITEM()
RATIONAL_B_SPLINE_CURVE((1.01933756729741,1.09818360252296,1.09818360252296))
REPRESENTATION_ITEM('')
);
#363=(
BOUNDED_CURVE()
B_SPLINE_CURVE(2,(#70600,#70601,#70602),.UNSPECIFIED.,.F.,.F.)
B_SPLINE_CURVE_WITH_KNOTS((3,3),(0.0830692064483412,1.5163968327409),
 .UNSPECIFIED.)
CURVE()
GEOMETRIC_REPRESENTATION_ITEM()
RATIONAL_B_SPLINE_CURVE((1.01933756729741,1.17702963774851,1.01933756729741))
REPRESENTATION_ITEM('')
);
#364=(
BOUNDED_CURVE()
B_SPLINE_CURVE(2,(#70604,#70605,#70606),.UNSPECIFIED.,.F.,.F.)
B_SPLINE_CURVE_WITH_KNOTS((3,3),(0.0830692064483411,1.5163968327409),
 .UNSPECIFIED.)
CURVE()
GEOMETRIC_REPRESENTATION_ITEM()
RATIONAL_B_SPLINE_CURVE((1.01933756729741,1.17702963774851,1.01933756729741))
REPRESENTATION_ITEM('')
);
#365=(
BOUNDED_CURVE()
B_SPLINE_CURVE(2,(#70608,#70609,#70610),.UNSPECIFIED.,.F.,.F.)
B_SPLINE_CURVE_WITH_KNOTS((3,3),(0.0830692064483411,1.5163968327409),
 .UNSPECIFIED.)
CURVE()
GEOMETRIC_REPRESENTATION_ITEM()
RATIONAL_B_SPLINE_CURVE((1.01933756729741,1.17702963774851,1.01933756729741))
REPRESENTATION_ITEM('')
);
#366=(
BOUNDED_CURVE()
B_SPLINE_CURVE(2,(#70612,#70613,#70614),.UNSPECIFIED.,.F.,.F.)
B_SPLINE_CURVE_WITH_KNOTS((3,3),(0.083069206448341,1.5163968327409),
 .UNSPECIFIED.)
CURVE()
GEOMETRIC_REPRESENTATION_ITEM()
RATIONAL_B_SPLINE_CURVE((1.01933756729741,1.17702963774852,1.01933756729741))
REPRESENTATION_ITEM('')
);
#367=(
BOUNDED_CURVE()
B_SPLINE_CURVE(2,(#70616,#70617,#70618),.UNSPECIFIED.,.F.,.F.)
B_SPLINE_CURVE_WITH_KNOTS((3,3),(0.0830692064483414,1.5163968327409),
 .UNSPECIFIED.)
CURVE()
GEOMETRIC_REPRESENTATION_ITEM()
RATIONAL_B_SPLINE_CURVE((1.01933756729741,1.17702963774851,1.01933756729741))
REPRESENTATION_ITEM('')
);
#368=(
BOUNDED_CURVE()
B_SPLINE_CURVE(2,(#70619,#70620,#70621),.UNSPECIFIED.,.F.,.F.)
B_SPLINE_CURVE_WITH_KNOTS((3,3),(0.799733019594622,1.5163968327409),
 .UNSPECIFIED.)
CURVE()
GEOMETRIC_REPRESENTATION_ITEM()
RATIONAL_B_SPLINE_CURVE((1.09818360252296,1.09818360252296,1.01933756729741))
REPRESENTATION_ITEM('')
);
#369=(
BOUNDED_CURVE()
B_SPLINE_CURVE(2,(#70626,#70627,#70628),.UNSPECIFIED.,.F.,.F.)
B_SPLINE_CURVE_WITH_KNOTS((3,3),(0.0830692064483413,1.5163968327409),
 .UNSPECIFIED.)
CURVE()
GEOMETRIC_REPRESENTATION_ITEM()
RATIONAL_B_SPLINE_CURVE((1.01933756729741,1.17702963774851,1.01933756729741))
REPRESENTATION_ITEM('')
);
#370=(
BOUNDED_CURVE()
B_SPLINE_CURVE(2,(#70633,#70634,#70635),.UNSPECIFIED.,.F.,.F.)
B_SPLINE_CURVE_WITH_KNOTS((3,3),(0.0830692064483417,1.5163968327409),
 .UNSPECIFIED.)
CURVE()
GEOMETRIC_REPRESENTATION_ITEM()
RATIONAL_B_SPLINE_CURVE((1.01933756729741,1.17702963774851,1.01933756729741))
REPRESENTATION_ITEM('')
);
#371=(
BOUNDED_CURVE()
B_SPLINE_CURVE(2,(#70639,#70640,#70641),.UNSPECIFIED.,.F.,.F.)
B_SPLINE_CURVE_WITH_KNOTS((3,3),(0.0830692064483414,1.5163968327409),
 .UNSPECIFIED.)
CURVE()
GEOMETRIC_REPRESENTATION_ITEM()
RATIONAL_B_SPLINE_CURVE((1.01933756729741,1.17702963774851,1.01933756729741))
REPRESENTATION_ITEM('')
);
#372=(
BOUNDED_CURVE()
B_SPLINE_CURVE(2,(#70644,#70645,#70646),.UNSPECIFIED.,.F.,.F.)
B_SPLINE_CURVE_WITH_KNOTS((3,3),(0.0830692064483411,1.5163968327409),
 .UNSPECIFIED.)
CURVE()
GEOMETRIC_REPRESENTATION_ITEM()
RATIONAL_B_SPLINE_CURVE((1.01933756729741,1.17702963774851,1.01933756729741))
REPRESENTATION_ITEM('')
);
#373=(
BOUNDED_CURVE()
B_SPLINE_CURVE(2,(#70648,#70649,#70650),.UNSPECIFIED.,.F.,.F.)
B_SPLINE_CURVE_WITH_KNOTS((3,3),(0.799733019594622,1.5163968327409),
 .UNSPECIFIED.)
CURVE()
GEOMETRIC_REPRESENTATION_ITEM()
RATIONAL_B_SPLINE_CURVE((1.09818360252296,1.09818360252296,1.01933756729741))
REPRESENTATION_ITEM('')
);
#374=(
BOUNDED_CURVE()
B_SPLINE_CURVE(2,(#70653,#70654,#70655),.UNSPECIFIED.,.F.,.F.)
B_SPLINE_CURVE_WITH_KNOTS((3,3),(0.0830692064483414,0.799733019594622),
 .UNSPECIFIED.)
CURVE()
GEOMETRIC_REPRESENTATION_ITEM()
RATIONAL_B_SPLINE_CURVE((1.01933756729741,1.09818360252296,1.09818360252296))
REPRESENTATION_ITEM('')
);
#375=(
BOUNDED_CURVE()
B_SPLINE_CURVE(2,(#70656,#70657,#70658),.UNSPECIFIED.,.F.,.F.)
B_SPLINE_CURVE_WITH_KNOTS((3,3),(0.0830692064483413,1.5163968327409),
 .UNSPECIFIED.)
CURVE()
GEOMETRIC_REPRESENTATION_ITEM()
RATIONAL_B_SPLINE_CURVE((1.01933756729741,1.17702963774851,1.01933756729741))
REPRESENTATION_ITEM('')
);
#376=TOROIDAL_SURFACE('',#29501,5.4,0.4);
#377=TOROIDAL_SURFACE('',#29987,1.8,0.299999999999997);
#378=TOROIDAL_SURFACE('',#30165,1.30000000000001,0.199999999999999);
#379=TOROIDAL_SURFACE('',#30175,1.29999999999998,0.199999999999999);
#380=TOROIDAL_SURFACE('',#30209,1.75,0.5);
#381=TOROIDAL_SURFACE('',#30426,0.8511,0.06);
#382=SHAPE_REPRESENTATION_RELATIONSHIP('SRR','None',#71603,#401);
#383=SHAPE_REPRESENTATION_RELATIONSHIP('SRR','None',#71604,#402);
#384=SHAPE_REPRESENTATION_RELATIONSHIP('SRR','None',#71605,#403);
#385=SHAPE_REPRESENTATION_RELATIONSHIP('SRR','None',#71606,#404);
#386=SHAPE_REPRESENTATION_RELATIONSHIP('SRR','None',#71607,#405);
#387=SHAPE_REPRESENTATION_RELATIONSHIP('SRR','None',#71608,#406);
#388=SHAPE_REPRESENTATION_RELATIONSHIP('SRR','None',#71609,#407);
#389=SHAPE_REPRESENTATION_RELATIONSHIP('SRR','None',#71610,#408);
#390=SHAPE_REPRESENTATION_RELATIONSHIP('SRR','None',#71611,#409);
#391=SHAPE_REPRESENTATION_RELATIONSHIP('SRR','None',#71612,#410);
#392=SHAPE_REPRESENTATION_RELATIONSHIP('SRR','None',#71613,#411);
#393=SHAPE_REPRESENTATION_RELATIONSHIP('SRR','None',#71614,#412);
#394=SHAPE_REPRESENTATION_RELATIONSHIP('SRR','None',#71615,#413);
#395=SHAPE_REPRESENTATION_RELATIONSHIP('SRR','None',#71616,#414);
#396=SHAPE_REPRESENTATION_RELATIONSHIP('SRR','None',#71617,#415);
#397=SHAPE_REPRESENTATION_RELATIONSHIP('SRR','None',#71618,#416);
#398=SHAPE_REPRESENTATION_RELATIONSHIP('SRR','None',#71619,#417);
#399=SHAPE_REPRESENTATION_RELATIONSHIP('SRR','None',#71620,#418);
#400=SHAPE_REPRESENTATION_RELATIONSHIP('SRR','None',#71621,#419);
#401=ADVANCED_BREP_SHAPE_REPRESENTATION('',(#420),#71473);
#402=ADVANCED_BREP_SHAPE_REPRESENTATION('',(#421),#71474);
#403=ADVANCED_BREP_SHAPE_REPRESENTATION('',(#422),#71475);
#404=ADVANCED_BREP_SHAPE_REPRESENTATION('',(#423),#71476);
#405=ADVANCED_BREP_SHAPE_REPRESENTATION('',(#424),#71477);
#406=ADVANCED_BREP_SHAPE_REPRESENTATION('',(#425),#71478);
#407=ADVANCED_BREP_SHAPE_REPRESENTATION('',(#426),#71479);
#408=ADVANCED_BREP_SHAPE_REPRESENTATION('',(#427),#71480);
#409=ADVANCED_BREP_SHAPE_REPRESENTATION('',(#428),#71481);
#410=ADVANCED_BREP_SHAPE_REPRESENTATION('',(#429),#71482);
#411=ADVANCED_BREP_SHAPE_REPRESENTATION('',(#430),#71483);
#412=ADVANCED_BREP_SHAPE_REPRESENTATION('',(#431),#71484);
#413=ADVANCED_BREP_SHAPE_REPRESENTATION('',(#432),#71485);
#414=ADVANCED_BREP_SHAPE_REPRESENTATION('',(#433),#71486);
#415=ADVANCED_BREP_SHAPE_REPRESENTATION('',(#434),#71487);
#416=ADVANCED_BREP_SHAPE_REPRESENTATION('',(#435),#71488);
#417=ADVANCED_BREP_SHAPE_REPRESENTATION('',(#436),#71489);
#418=ADVANCED_BREP_SHAPE_REPRESENTATION('',(#437),#71490);
#419=ADVANCED_BREP_SHAPE_REPRESENTATION('',(#438),#71491);
#420=MANIFOLD_SOLID_BREP('Top beam',#28459);
#421=MANIFOLD_SOLID_BREP('Platen',#28460);
#422=MANIFOLD_SOLID_BREP('Bed',#28461);
#423=MANIFOLD_SOLID_BREP('Brace',#28462);
#424=MANIFOLD_SOLID_BREP('Jack body',#28463);
#425=MANIFOLD_SOLID_BREP('Ram',#28464);
#426=MANIFOLD_SOLID_BREP('Release knob',#28465);
#427=MANIFOLD_SOLID_BREP('Gauge',#28466);
#428=MANIFOLD_SOLID_BREP('Pin',#28467);
#429=MANIFOLD_SOLID_BREP('R-clip',#28468);
#430=MANIFOLD_SOLID_BREP('Foot',#28469);
#431=MANIFOLD_SOLID_BREP('Spring',#28470);
#432=MANIFOLD_SOLID_BREP('Eye bolt',#28471);
#433=MANIFOLD_SOLID_BREP('V-block',#28472);
#434=MANIFOLD_SOLID_BREP('Bolt',#28473);
#435=MANIFOLD_SOLID_BREP('Nut',#28474);
#436=MANIFOLD_SOLID_BREP('Washer',#28475);
#437=MANIFOLD_SOLID_BREP('Handle',#28476);
#438=MANIFOLD_SOLID_BREP('Upright',#28477);
#439=STYLED_ITEM('',(#71873),#27095);
#440=STYLED_ITEM('',(#71873),#27096);
#441=STYLED_ITEM('',(#71873),#27097);
#442=STYLED_ITEM('',(#71873),#27098);
#443=STYLED_ITEM('',(#71873),#27099);
#444=STYLED_ITEM('',(#71873),#27100);
#445=STYLED_ITEM('',(#71873),#27101);
#446=STYLED_ITEM('',(#71873),#27102);
#447=STYLED_ITEM('',(#71873),#27103);
#448=STYLED_ITEM('',(#71873),#27104);
#449=STYLED_ITEM('',(#71873),#27105);
#450=STYLED_ITEM('',(#71873),#27106);
#451=STYLED_ITEM('',(#71873),#27107);
#452=STYLED_ITEM('',(#71873),#27108);
#453=STYLED_ITEM('',(#71873),#27109);
#454=STYLED_ITEM('',(#71873),#27110);
#455=STYLED_ITEM('',(#71873),#27111);
#456=STYLED_ITEM('',(#71873),#27112);
#457=STYLED_ITEM('',(#71873),#27113);
#458=STYLED_ITEM('',(#71873),#27114);
#459=STYLED_ITEM('',(#71873),#27115);
#460=STYLED_ITEM('',(#71873),#27116);
#461=STYLED_ITEM('',(#71873),#27117);
#462=STYLED_ITEM('',(#71873),#27118);
#463=STYLED_ITEM('',(#71873),#27119);
#464=STYLED_ITEM('',(#71873),#27120);
#465=STYLED_ITEM('',(#71873),#27121);
#466=STYLED_ITEM('',(#71873),#27122);
#467=STYLED_ITEM('',(#71873),#27123);
#468=STYLED_ITEM('',(#71873),#27124);
#469=STYLED_ITEM('',(#71873),#27125);
#470=STYLED_ITEM('',(#71873),#27126);
#471=STYLED_ITEM('',(#71873),#27127);
#472=STYLED_ITEM('',(#71873),#27128);
#473=STYLED_ITEM('',(#71873),#27129);
#474=STYLED_ITEM('',(#71873),#27130);
#475=STYLED_ITEM('',(#71873),#27131);
#476=STYLED_ITEM('',(#71873),#27132);
#477=STYLED_ITEM('',(#71873),#27133);
#478=STYLED_ITEM('',(#71873),#27134);
#479=STYLED_ITEM('',(#71873),#27135);
#480=STYLED_ITEM('',(#71873),#27136);
#481=STYLED_ITEM('',(#71873),#27137);
#482=STYLED_ITEM('',(#71873),#27138);
#483=STYLED_ITEM('',(#71873),#27139);
#484=STYLED_ITEM('',(#71873),#27140);
#485=STYLED_ITEM('',(#71873),#27141);
#486=STYLED_ITEM('',(#71873),#27142);
#487=STYLED_ITEM('',(#71873),#27143);
#488=STYLED_ITEM('',(#71873),#27144);
#489=STYLED_ITEM('',(#71873),#27145);
#490=STYLED_ITEM('',(#71873),#27146);
#491=STYLED_ITEM('',(#71873),#27147);
#492=STYLED_ITEM('',(#71873),#27148);
#493=STYLED_ITEM('',(#71873),#27149);
#494=STYLED_ITEM('',(#71873),#27150);
#495=STYLED_ITEM('',(#71873),#27151);
#496=STYLED_ITEM('',(#71873),#27152);
#497=STYLED_ITEM('',(#71873),#27153);
#498=STYLED_ITEM('',(#71873),#27154);
#499=STYLED_ITEM('',(#71873),#27155);
#500=STYLED_ITEM('',(#71873),#27156);
#501=STYLED_ITEM('',(#71873),#27157);
#502=STYLED_ITEM('',(#71873),#27158);
#503=STYLED_ITEM('',(#71873),#27159);
#504=STYLED_ITEM('',(#71873),#27160);
#505=STYLED_ITEM('',(#71873),#27161);
#506=STYLED_ITEM('',(#71873),#27162);
#507=STYLED_ITEM('',(#71873),#27163);
#508=STYLED_ITEM('',(#71873),#27164);
#509=STYLED_ITEM('',(#71873),#27165);
#510=STYLED_ITEM('',(#71873),#27166);
#511=STYLED_ITEM('',(#71873),#27167);
#512=STYLED_ITEM('',(#71873),#27168);
#513=STYLED_ITEM('',(#71873),#27169);
#514=STYLED_ITEM('',(#71873),#27170);
#515=STYLED_ITEM('',(#71873),#27171);
#516=STYLED_ITEM('',(#71873),#27172);
#517=STYLED_ITEM('',(#71873),#27173);
#518=STYLED_ITEM('',(#71873),#27174);
#519=STYLED_ITEM('',(#71873),#27175);
#520=STYLED_ITEM('',(#71873),#27176);
#521=STYLED_ITEM('',(#71873),#27177);
#522=STYLED_ITEM('',(#71873),#27178);
#523=STYLED_ITEM('',(#71873),#27179);
#524=STYLED_ITEM('',(#71873),#420);
#525=STYLED_ITEM('',(#71887),#421);
#526=STYLED_ITEM('',(#71901),#422);
#527=STYLED_ITEM('',(#71873),#423);
#528=STYLED_ITEM('',(#71866),#424);
#529=STYLED_ITEM('',(#71894),#425);
#530=STYLED_ITEM('',(#71873),#426);
#531=STYLED_ITEM('',(#71901),#27845);
#532=STYLED_ITEM('',(#71901),#427);
#533=STYLED_ITEM('',(#71887),#428);
#534=STYLED_ITEM('',(#71887),#429);
#535=STYLED_ITEM('',(#71866),#430);
#536=STYLED_ITEM('',(#71887),#431);
#537=STYLED_ITEM('',(#71894),#432);
#538=STYLED_ITEM('',(#71866),#433);
#539=STYLED_ITEM('',(#71894),#434);
#540=STYLED_ITEM('',(#71894),#435);
#541=STYLED_ITEM('',(#71894),#436);
#542=STYLED_ITEM('',(#71880),#28308);
#543=STYLED_ITEM('',(#71880),#28315);
#544=STYLED_ITEM('',(#71880),#28318);
#545=STYLED_ITEM('',(#71880),#28320);
#546=STYLED_ITEM('',(#71880),#28322);
#547=STYLED_ITEM('',(#71880),#28324);
#548=STYLED_ITEM('',(#71880),#28326);
#549=STYLED_ITEM('',(#71880),#437);
#550=STYLED_ITEM('',(#71873),#438);
#551=B_SPLINE_CURVE_WITH_KNOTS('',3,(#37939,#37940,#37941,#37942,#37943,
#37944,#37945,#37946,#37947),.UNSPECIFIED.,.F.,.F.,(4,2,1,1,1,4),(-2.76222327472562,
-2.70245118401238,-2.26839934091757,-2.05137341937016,-1.83434749782276,
-1.61732157627536),.UNSPECIFIED.);
#552=B_SPLINE_CURVE_WITH_KNOTS('',3,(#37950,#37951,#37952,#37953,#37954,
#37955,#37956,#37957,#37958),.UNSPECIFIED.,.F.,.F.,(4,1,1,1,2,4),(1.61732157627536,
1.83434749782276,2.05137341937016,2.26839934091757,2.70245118401238,2.76222327472562),
 .UNSPECIFIED.);
#553=B_SPLINE_CURVE_WITH_KNOTS('',3,(#37975,#37976,#37977,#37978),
 .UNSPECIFIED.,.F.,.F.,(4,4),(1.90569248523429,2.03375105473527),
 .UNSPECIFIED.);
#554=B_SPLINE_CURVE_WITH_KNOTS('',3,(#37979,#37980,#37981,#37982),
 .UNSPECIFIED.,.F.,.F.,(4,4),(-2.03375105473527,-1.90569248523429),
 .UNSPECIFIED.);
#555=B_SPLINE_CURVE_WITH_KNOTS('',3,(#37999,#38000,#38001,#38002),
 .UNSPECIFIED.,.F.,.F.,(4,4),(1.10784159885376,1.2359001683555),
 .UNSPECIFIED.);
#556=B_SPLINE_CURVE_WITH_KNOTS('',3,(#38003,#38004,#38005,#38006),
 .UNSPECIFIED.,.F.,.F.,(4,4),(-1.2359001683555,-1.10784159885376),
 .UNSPECIFIED.);
#557=B_SPLINE_CURVE_WITH_KNOTS('',3,(#38019,#38020,#38021,#38022),
 .UNSPECIFIED.,.F.,.F.,(4,4),(1.90569248523429,2.03375105473527),
 .UNSPECIFIED.);
#558=B_SPLINE_CURVE_WITH_KNOTS('',3,(#38024,#38025,#38026,#38027,#38028,
#38029,#38030,#38031,#38032,#38033),.UNSPECIFIED.,.F.,.F.,(4,2,1,1,1,1,
4),(-2.76222327472564,-2.70245118401238,-2.48542526246498,-2.26839934091757,
-2.05137341937017,-1.83434749782276,-1.61732157627536),.UNSPECIFIED.);
#559=B_SPLINE_CURVE_WITH_KNOTS('',3,(#38035,#38036,#38037,#38038),
 .UNSPECIFIED.,.F.,.F.,(4,4),(1.10784159885378,1.2359001683555),
 .UNSPECIFIED.);
#560=B_SPLINE_CURVE_WITH_KNOTS('',3,(#38046,#38047,#38048,#38049),
 .UNSPECIFIED.,.F.,.F.,(4,4),(2.15648187025205,2.23164162261786),
 .UNSPECIFIED.);
#561=B_SPLINE_CURVE_WITH_KNOTS('',3,(#38051,#38052,#38053,#38054,#38055,
#38056,#38057,#38058,#38059,#38060,#38061,#38062,#38063,#38064,#38065,#38066,
#38067,#38068,#38069,#38070,#38071,#38072,#38073,#38074,#38075,#38076,#38077,
#38078,#38079,#38080,#38081,#38082,#38083,#38084,#38085,#38086,#38087),
 .UNSPECIFIED.,.F.,.F.,(4,3,3,3,3,3,3,3,3,3,3,3,4),(0.754355313185428,0.781440569694549,
0.818270933113804,1.2600819055102,1.70189287790659,1.71022064144053,1.73520393204235,
1.80478675064372,1.8743695692451,1.92549026456033,1.97661095987556,2.5752615771494,
2.77481178290734),.UNSPECIFIED.);
#562=B_SPLINE_CURVE_WITH_KNOTS('',3,(#38089,#38090,#38091,#38092),
 .UNSPECIFIED.,.F.,.F.,(4,4),(0.90995103097194,0.98511078333776),
 .UNSPECIFIED.);
#563=B_SPLINE_CURVE_WITH_KNOTS('',3,(#38174,#38175,#38176,#38177),
 .UNSPECIFIED.,.F.,.F.,(4,4),(-1.2359001683555,-1.10784159885453),
 .UNSPECIFIED.);
#564=B_SPLINE_CURVE_WITH_KNOTS('',3,(#38179,#38180,#38181,#38182,#38183,
#38184,#38185,#38186,#38187,#38188),.UNSPECIFIED.,.F.,.F.,(4,2,1,1,2,4),
(-2.76222327472564,-2.70245118401238,-2.29230817720287,-2.08723667379812,
-1.67709366698862,-1.61732157627537),.UNSPECIFIED.);
#565=B_SPLINE_CURVE_WITH_KNOTS('',3,(#38190,#38191,#38192,#38193),
 .UNSPECIFIED.,.F.,.F.,(4,4),(-2.03375105473602,-1.9056924852343),
 .UNSPECIFIED.);
#566=B_SPLINE_CURVE_WITH_KNOTS('',3,(#38197,#38198,#38199,#38200),
 .UNSPECIFIED.,.F.,.F.,(4,4),(-1.2359001683555,-1.10784159885453),
 .UNSPECIFIED.);
#567=B_SPLINE_CURVE_WITH_KNOTS('',3,(#38202,#38203,#38204,#38205,#38206,
#38207,#38208,#38209,#38210,#38211,#38212),.UNSPECIFIED.,.F.,.F.,(4,2,1,
1,1,2,4),(-2.76222327472563,-2.70245118401238,-2.49737968060763,-2.39484392890525,
-2.08723667379813,-1.67709366698862,-1.61732157627537),.UNSPECIFIED.);
#568=B_SPLINE_CURVE_WITH_KNOTS('',3,(#38214,#38215,#38216,#38217),
 .UNSPECIFIED.,.F.,.F.,(4,4),(-2.03375105473601,-1.9056924852343),
 .UNSPECIFIED.);
#569=B_SPLINE_CURVE_WITH_KNOTS('',2,(#38285,#38286,#38287),
 .UNSPECIFIED.,.F.,.F.,(3,3),(0.,1.),.UNSPECIFIED.);
#570=B_SPLINE_CURVE_WITH_KNOTS('',2,(#38289,#38290,#38291),
 .UNSPECIFIED.,.F.,.F.,(3,3),(0.,1.),.UNSPECIFIED.);
#571=B_SPLINE_CURVE_WITH_KNOTS('',2,(#38293,#38294,#38295),
 .UNSPECIFIED.,.F.,.F.,(3,3),(0.,1.),.UNSPECIFIED.);
#572=B_SPLINE_CURVE_WITH_KNOTS('',2,(#38297,#38298,#38299),
 .UNSPECIFIED.,.F.,.F.,(3,3),(0.,1.),.UNSPECIFIED.);
#573=B_SPLINE_CURVE_WITH_KNOTS('',2,(#38301,#38302,#38303),
 .UNSPECIFIED.,.F.,.F.,(3,3),(0.,1.),.UNSPECIFIED.);
#574=B_SPLINE_CURVE_WITH_KNOTS('',2,(#38305,#38306,#38307),
 .UNSPECIFIED.,.F.,.F.,(3,3),(0.,1.),.UNSPECIFIED.);
#575=B_SPLINE_CURVE_WITH_KNOTS('',2,(#38309,#38310,#38311),
 .UNSPECIFIED.,.F.,.F.,(3,3),(0.,1.),.UNSPECIFIED.);
#576=B_SPLINE_CURVE_WITH_KNOTS('',2,(#38313,#38314,#38315),
 .UNSPECIFIED.,.F.,.F.,(3,3),(0.,1.),.UNSPECIFIED.);
#577=B_SPLINE_CURVE_WITH_KNOTS('',2,(#38317,#38318,#38319),
 .UNSPECIFIED.,.F.,.F.,(3,3),(0.,1.),.UNSPECIFIED.);
#578=B_SPLINE_CURVE_WITH_KNOTS('',2,(#38320,#38321,#38322),
 .UNSPECIFIED.,.F.,.F.,(3,3),(0.,1.),.UNSPECIFIED.);
#579=B_SPLINE_CURVE_WITH_KNOTS('',2,(#38341,#38342,#38343),
 .UNSPECIFIED.,.F.,.F.,(3,3),(0.,1.),.UNSPECIFIED.);
#580=B_SPLINE_CURVE_WITH_KNOTS('',2,(#38345,#38346,#38347),
 .UNSPECIFIED.,.F.,.F.,(3,3),(0.,1.),.UNSPECIFIED.);
#581=B_SPLINE_CURVE_WITH_KNOTS('',2,(#38349,#38350,#38351),
 .UNSPECIFIED.,.F.,.F.,(3,3),(0.,1.),.UNSPECIFIED.);
#582=B_SPLINE_CURVE_WITH_KNOTS('',2,(#38353,#38354,#38355),
 .UNSPECIFIED.,.F.,.F.,(3,3),(0.,1.),.UNSPECIFIED.);
#583=B_SPLINE_CURVE_WITH_KNOTS('',2,(#38357,#38358,#38359),
 .UNSPECIFIED.,.F.,.F.,(3,3),(0.,1.),.UNSPECIFIED.);
#584=B_SPLINE_CURVE_WITH_KNOTS('',2,(#38361,#38362,#38363),
 .UNSPECIFIED.,.F.,.F.,(3,3),(0.,1.),.UNSPECIFIED.);
#585=B_SPLINE_CURVE_WITH_KNOTS('',2,(#38365,#38366,#38367),
 .UNSPECIFIED.,.F.,.F.,(3,3),(0.,1.),.UNSPECIFIED.);
#586=B_SPLINE_CURVE_WITH_KNOTS('',2,(#38369,#38370,#38371),
 .UNSPECIFIED.,.F.,.F.,(3,3),(0.,1.),.UNSPECIFIED.);
#587=B_SPLINE_CURVE_WITH_KNOTS('',2,(#38373,#38374,#38375),
 .UNSPECIFIED.,.F.,.F.,(3,3),(0.,1.),.UNSPECIFIED.);
#588=B_SPLINE_CURVE_WITH_KNOTS('',2,(#38377,#38378,#38379),
 .UNSPECIFIED.,.F.,.F.,(3,3),(0.,1.),.UNSPECIFIED.);
#589=B_SPLINE_CURVE_WITH_KNOTS('',2,(#38381,#38382,#38383),
 .UNSPECIFIED.,.F.,.F.,(3,3),(0.,1.),.UNSPECIFIED.);
#590=B_SPLINE_CURVE_WITH_KNOTS('',2,(#38385,#38386,#38387),
 .UNSPECIFIED.,.F.,.F.,(3,3),(0.,1.),.UNSPECIFIED.);
#591=B_SPLINE_CURVE_WITH_KNOTS('',2,(#38388,#38389,#38390),
 .UNSPECIFIED.,.F.,.F.,(3,3),(0.,1.),.UNSPECIFIED.);
#592=B_SPLINE_CURVE_WITH_KNOTS('',2,(#38399,#38400,#38401),
 .UNSPECIFIED.,.F.,.F.,(3,3),(0.,1.),.UNSPECIFIED.);
#593=B_SPLINE_CURVE_WITH_KNOTS('',2,(#38403,#38404,#38405),
 .UNSPECIFIED.,.F.,.F.,(3,3),(0.,1.),.UNSPECIFIED.);
#594=B_SPLINE_CURVE_WITH_KNOTS('',2,(#38407,#38408,#38409),
 .UNSPECIFIED.,.F.,.F.,(3,3),(0.,1.),.UNSPECIFIED.);
#595=B_SPLINE_CURVE_WITH_KNOTS('',2,(#38411,#38412,#38413),
 .UNSPECIFIED.,.F.,.F.,(3,3),(0.,1.),.UNSPECIFIED.);
#596=B_SPLINE_CURVE_WITH_KNOTS('',2,(#38415,#38416,#38417),
 .UNSPECIFIED.,.F.,.F.,(3,3),(0.,1.),.UNSPECIFIED.);
#597=B_SPLINE_CURVE_WITH_KNOTS('',2,(#38419,#38420,#38421),
 .UNSPECIFIED.,.F.,.F.,(3,3),(0.,1.),.UNSPECIFIED.);
#598=B_SPLINE_CURVE_WITH_KNOTS('',2,(#38423,#38424,#38425),
 .UNSPECIFIED.,.F.,.F.,(3,3),(0.,1.),.UNSPECIFIED.);
#599=B_SPLINE_CURVE_WITH_KNOTS('',2,(#38427,#38428,#38429),
 .UNSPECIFIED.,.F.,.F.,(3,3),(0.,1.),.UNSPECIFIED.);
#600=B_SPLINE_CURVE_WITH_KNOTS('',2,(#38433,#38434,#38435),
 .UNSPECIFIED.,.F.,.F.,(3,3),(0.,1.),.UNSPECIFIED.);
#601=B_SPLINE_CURVE_WITH_KNOTS('',2,(#38437,#38438,#38439),
 .UNSPECIFIED.,.F.,.F.,(3,3),(0.,1.),.UNSPECIFIED.);
#602=B_SPLINE_CURVE_WITH_KNOTS('',2,(#38441,#38442,#38443),
 .UNSPECIFIED.,.F.,.F.,(3,3),(0.,1.),.UNSPECIFIED.);
#603=B_SPLINE_CURVE_WITH_KNOTS('',2,(#38445,#38446,#38447),
 .UNSPECIFIED.,.F.,.F.,(3,3),(0.,1.),.UNSPECIFIED.);
#604=B_SPLINE_CURVE_WITH_KNOTS('',2,(#38449,#38450,#38451),
 .UNSPECIFIED.,.F.,.F.,(3,3),(0.,1.),.UNSPECIFIED.);
#605=B_SPLINE_CURVE_WITH_KNOTS('',2,(#38453,#38454,#38455),
 .UNSPECIFIED.,.F.,.F.,(3,3),(0.,1.),.UNSPECIFIED.);
#606=B_SPLINE_CURVE_WITH_KNOTS('',2,(#38457,#38458,#38459),
 .UNSPECIFIED.,.F.,.F.,(3,3),(0.,1.),.UNSPECIFIED.);
#607=B_SPLINE_CURVE_WITH_KNOTS('',2,(#38461,#38462,#38463),
 .UNSPECIFIED.,.F.,.F.,(3,3),(0.,1.),.UNSPECIFIED.);
#608=B_SPLINE_CURVE_WITH_KNOTS('',2,(#38465,#38466,#38467),
 .UNSPECIFIED.,.F.,.F.,(3,3),(0.,1.),.UNSPECIFIED.);
#609=B_SPLINE_CURVE_WITH_KNOTS('',2,(#38468,#38469,#38470),
 .UNSPECIFIED.,.F.,.F.,(3,3),(0.,1.),.UNSPECIFIED.);
#610=B_SPLINE_CURVE_WITH_KNOTS('',3,(#38564,#38565,#38566,#38567,#38568,
#38569,#38570,#38571,#38572,#38573,#38574),.UNSPECIFIED.,.F.,.F.,(4,2,1,
1,1,2,4),(1.61732157627537,1.67709366698862,2.08723667379813,2.39484392890525,
2.49737968060763,2.70245118401238,2.76222327472563),.UNSPECIFIED.);
#611=B_SPLINE_CURVE_WITH_KNOTS('',3,(#38591,#38592,#38593,#38594),
 .UNSPECIFIED.,.F.,.F.,(4,4),(1.10784159885453,1.2359001683555),
 .UNSPECIFIED.);
#612=B_SPLINE_CURVE_WITH_KNOTS('',3,(#38611,#38612,#38613,#38614),
 .UNSPECIFIED.,.F.,.F.,(4,4),(1.9056924852343,2.03375105473601),
 .UNSPECIFIED.);
#613=B_SPLINE_CURVE_WITH_KNOTS('',3,(#38621,#38622,#38623,#38624),
 .UNSPECIFIED.,.F.,.F.,(4,4),(-0.985110783337743,-0.909951030971934),
 .UNSPECIFIED.);
#614=B_SPLINE_CURVE_WITH_KNOTS('',3,(#38626,#38627,#38628,#38629,#38630,
#38631,#38632,#38633,#38634,#38635,#38636,#38637,#38638,#38639,#38640,#38641,
#38642,#38643,#38644,#38645,#38646,#38647,#38648,#38649,#38650,#38651,#38652,
#38653,#38654,#38655,#38656),.UNSPECIFIED.,.F.,.F.,(4,3,3,3,3,3,3,3,3,3,
4),(0.754355313185451,0.781440569694569,0.818270933113807,1.42914691644436,
1.63277224422121,1.70189287790658,1.73520393204232,1.87436956924877,1.97661095987549,
2.57526157714938,2.77481178290734),.UNSPECIFIED.);
#615=B_SPLINE_CURVE_WITH_KNOTS('',3,(#38658,#38659,#38660,#38661),
 .UNSPECIFIED.,.F.,.F.,(4,4),(-2.23164162261785,-2.15648187025204),
 .UNSPECIFIED.);
#616=B_SPLINE_CURVE_WITH_KNOTS('',3,(#38715,#38716,#38717,#38718,#38719,
#38720,#38721,#38722,#38723,#38724),.UNSPECIFIED.,.F.,.F.,(4,1,1,1,1,2,
4),(1.61732157627536,1.83434749782276,2.05137341937017,2.26839934091757,
2.48542526246498,2.70245118401238,2.76222327472564),.UNSPECIFIED.);
#617=B_SPLINE_CURVE_WITH_KNOTS('',3,(#38741,#38742,#38743,#38744),
 .UNSPECIFIED.,.F.,.F.,(4,4),(-2.03375105473527,-1.90569248523429),
 .UNSPECIFIED.);
#618=B_SPLINE_CURVE_WITH_KNOTS('',3,(#38761,#38762,#38763,#38764),
 .UNSPECIFIED.,.F.,.F.,(4,4),(-1.2359001683555,-1.10784159885378),
 .UNSPECIFIED.);
#619=B_SPLINE_CURVE_WITH_KNOTS('',3,(#38771,#38772,#38773,#38774),
 .UNSPECIFIED.,.F.,.F.,(4,4),(2.15648187025205,2.23164162261786),
 .UNSPECIFIED.);
#620=B_SPLINE_CURVE_WITH_KNOTS('',3,(#38776,#38777,#38778,#38779,#38780,
#38781,#38782,#38783,#38784,#38785,#38786,#38787,#38788,#38789,#38790,#38791,
#38792,#38793,#38794,#38795,#38796,#38797,#38798,#38799,#38800,#38801,#38802,
#38803,#38804,#38805,#38806,#38807,#38808,#38809,#38810,#38811,#38812),
 .UNSPECIFIED.,.F.,.F.,(4,3,3,3,3,3,3,3,3,3,3,3,4),(0.75435531318544,0.781440569694525,
0.818270933113715,1.47797557423085,1.63277224422101,1.70189287790658,1.73520393204241,
1.87436956924587,1.97661095987572,2.10085602838433,2.43783390564597,2.60632284427679,
2.77481178290761),.UNSPECIFIED.);
#621=B_SPLINE_CURVE_WITH_KNOTS('',3,(#38814,#38815,#38816,#38817),
 .UNSPECIFIED.,.F.,.F.,(4,4),(0.90995103097194,0.985110783337756),
 .UNSPECIFIED.);
#622=B_SPLINE_CURVE_WITH_KNOTS('',3,(#38860,#38861,#38862,#38863),
 .UNSPECIFIED.,.F.,.F.,(4,4),(2.15648187025204,2.23164162261785),
 .UNSPECIFIED.);
#623=B_SPLINE_CURVE_WITH_KNOTS('',3,(#38865,#38866,#38867,#38868,#38869,
#38870,#38871,#38872,#38873,#38874),.UNSPECIFIED.,.F.,.F.,(4,3,3,4),(-1.16153810946438,
-0.819783369909235,-0.782081488746963,-0.754355313185429),.UNSPECIFIED.);
#624=B_SPLINE_CURVE_WITH_KNOTS('',3,(#38876,#38877,#38878,#38879,#38880,
#38881,#38882,#38883,#38884,#38885,#38886,#38887,#38888,#38889,#38890),
 .UNSPECIFIED.,.F.,.F.,(4,2,2,2,2,2,1,4),(-2.39250890756734,-2.0015894299973,
-1.89936032175267,-1.76021140268278,-1.72690435024433,-1.6577920201044,
-1.45419115408482,-1.17754443036118),.UNSPECIFIED.);
#625=B_SPLINE_CURVE_WITH_KNOTS('',3,(#38892,#38893,#38894,#38895,#38896),
 .UNSPECIFIED.,.F.,.F.,(4,1,4),(-2.79969436419745,-2.60016813064741,-2.39250890756734),
 .UNSPECIFIED.);
#626=B_SPLINE_CURVE_WITH_KNOTS('',3,(#38898,#38899,#38900,#38901),
 .UNSPECIFIED.,.F.,.F.,(4,4),(0.969091106047996,0.985110783337743),
 .UNSPECIFIED.);
#627=B_SPLINE_CURVE_WITH_KNOTS('',3,(#38903,#38904,#38905,#38906),
 .UNSPECIFIED.,.F.,.F.,(4,4),(0.909951030971922,0.969091106047996),
 .UNSPECIFIED.);
#628=B_SPLINE_CURVE_WITH_KNOTS('',3,(#38910,#38911,#38912,#38913),
 .UNSPECIFIED.,.F.,.F.,(4,4),(2.15648187025204,2.23164162261785),
 .UNSPECIFIED.);
#629=B_SPLINE_CURVE_WITH_KNOTS('',3,(#38915,#38916,#38917,#38918,#38919,
#38920,#38921,#38922,#38923,#38924),.UNSPECIFIED.,.F.,.F.,(4,3,3,4),(-1.16153810946442,
-0.8197833699093,-0.782081488746932,-0.754355313185416),.UNSPECIFIED.);
#630=B_SPLINE_CURVE_WITH_KNOTS('',3,(#38926,#38927,#38928,#38929,#38930,
#38931,#38932,#38933,#38934,#38935,#38936,#38937),.UNSPECIFIED.,.F.,.F.,
(4,2,2,2,1,1,4),(-2.39249743427155,-1.89936032175298,-1.76021140268327,
-1.72690435024575,-1.50602540169085,-1.28514645313595,-1.17750891267616),
 .UNSPECIFIED.);
#631=B_SPLINE_CURVE_WITH_KNOTS('',3,(#38939,#38940,#38941,#38942,#38943,
#38944),.UNSPECIFIED.,.F.,.F.,(4,1,1,4),(-2.79969436419745,-2.68715260889189,
-2.57461085358633,-2.39249743427155),.UNSPECIFIED.);
#632=B_SPLINE_CURVE_WITH_KNOTS('',3,(#38946,#38947,#38948,#38949),
 .UNSPECIFIED.,.F.,.F.,(4,4),(0.969091106053859,0.985110783337744),
 .UNSPECIFIED.);
#633=B_SPLINE_CURVE_WITH_KNOTS('',3,(#38951,#38952,#38953,#38954),
 .UNSPECIFIED.,.F.,.F.,(4,4),(0.909951030971929,0.969091106053859),
 .UNSPECIFIED.);
#634=B_SPLINE_CURVE_WITH_KNOTS('',3,(#39116,#39117,#39118,#39119),
 .UNSPECIFIED.,.F.,.F.,(4,4),(-0.98511078333776,-0.90995103097194),
 .UNSPECIFIED.);
#635=B_SPLINE_CURVE_WITH_KNOTS('',3,(#39121,#39122,#39123,#39124,#39125,
#39126,#39127,#39128,#39129,#39130),.UNSPECIFIED.,.F.,.F.,(4,3,3,4),(-1.16153810946441,
-0.819783369909218,-0.782081488746928,-0.754355313185416),.UNSPECIFIED.);
#636=B_SPLINE_CURVE_WITH_KNOTS('',3,(#39132,#39133,#39134,#39135,#39136,
#39137,#39138,#39139,#39140,#39141,#39142,#39143,#39144,#39145,#39146,#39147),
 .UNSPECIFIED.,.F.,.F.,(4,2,1,2,1,2,1,2,1,4),(-2.39254555505919,-2.00158942999727,
-1.95047487587308,-1.89936032174889,-1.82978586221579,-1.76021140268269,
-1.73523111335382,-1.7269043502442,-1.28514645313502,-1.17757064087985),
 .UNSPECIFIED.);
#637=B_SPLINE_CURVE_WITH_KNOTS('',3,(#39149,#39150,#39151,#39152,#39153),
 .UNSPECIFIED.,.F.,.F.,(4,1,4),(-2.79969436419745,-2.60016813064741,-2.39254555505919),
 .UNSPECIFIED.);
#638=B_SPLINE_CURVE_WITH_KNOTS('',3,(#39155,#39156,#39157,#39158),
 .UNSPECIFIED.,.F.,.F.,(4,4),(-2.17250154754389,-2.15648187025205),
 .UNSPECIFIED.);
#639=B_SPLINE_CURVE_WITH_KNOTS('',3,(#39159,#39160,#39161,#39162),
 .UNSPECIFIED.,.F.,.F.,(4,4),(-2.23164162261787,-2.17250154754389),
 .UNSPECIFIED.);
#640=B_SPLINE_CURVE_WITH_KNOTS('',3,(#39164,#39165,#39166,#39167),
 .UNSPECIFIED.,.F.,.F.,(4,4),(-0.985110783337756,-0.90995103097194),
 .UNSPECIFIED.);
#641=B_SPLINE_CURVE_WITH_KNOTS('',3,(#39169,#39170,#39171,#39172,#39173,
#39174,#39175,#39176,#39177,#39178),.UNSPECIFIED.,.F.,.F.,(4,3,3,4),(-1.16153810946433,
-0.819783369909133,-0.782081488746918,-0.754355313185436),.UNSPECIFIED.);
#642=B_SPLINE_CURVE_WITH_KNOTS('',3,(#39180,#39181,#39182,#39183,#39184,
#39185,#39186,#39187,#39188,#39189,#39190,#39191,#39192,#39193,#39194,#39195,
#39196,#39197),.UNSPECIFIED.,.F.,.F.,(4,2,2,2,2,2,2,2,4),(-2.39280165059179,
-2.12581957279538,-2.00158942999736,-1.89936032174962,-1.76021140268274,
-1.72690435024419,-1.65779202010408,-1.50301394602541,-1.17741711999687),
 .UNSPECIFIED.);
#643=B_SPLINE_CURVE_WITH_KNOTS('',3,(#39199,#39200,#39201,#39202,#39203,
#39204),.UNSPECIFIED.,.F.,.F.,(4,1,1,4),(-2.79969436419745,-2.63122566634693,
-2.46275696849641,-2.39280165059179),.UNSPECIFIED.);
#644=B_SPLINE_CURVE_WITH_KNOTS('',3,(#39206,#39207,#39208,#39209),
 .UNSPECIFIED.,.F.,.F.,(4,4),(-2.17250154754018,-2.15648187025205),
 .UNSPECIFIED.);
#645=B_SPLINE_CURVE_WITH_KNOTS('',3,(#39210,#39211,#39212,#39213),
 .UNSPECIFIED.,.F.,.F.,(4,4),(-2.23164162261787,-2.17250154754018),
 .UNSPECIFIED.);
#646=B_SPLINE_CURVE_WITH_KNOTS('',3,(#39520,#39521,#39522,#39523,#39524,
#39525,#39526,#39527,#39528,#39529),.UNSPECIFIED.,.F.,.F.,(4,2,1,1,2,4),
(1.61732157627537,1.67709366698862,2.08723667379812,2.29230817720287,2.70245118401238,
2.76222327472564),.UNSPECIFIED.);
#647=B_SPLINE_CURVE_WITH_KNOTS('',3,(#39546,#39547,#39548,#39549),
 .UNSPECIFIED.,.F.,.F.,(4,4),(1.10784159885453,1.2359001683555),
 .UNSPECIFIED.);
#648=B_SPLINE_CURVE_WITH_KNOTS('',3,(#39566,#39567,#39568,#39569),
 .UNSPECIFIED.,.F.,.F.,(4,4),(1.9056924852343,2.03375105473602),
 .UNSPECIFIED.);
#649=B_SPLINE_CURVE_WITH_KNOTS('',3,(#39576,#39577,#39578,#39579),
 .UNSPECIFIED.,.F.,.F.,(4,4),(-0.985110783337744,-0.909951030971936),
 .UNSPECIFIED.);
#650=B_SPLINE_CURVE_WITH_KNOTS('',3,(#39581,#39582,#39583,#39584,#39585,
#39586,#39587,#39588,#39589,#39590,#39591,#39592,#39593,#39594,#39595,#39596,
#39597,#39598,#39599,#39600,#39601,#39602,#39603,#39604,#39605,#39606,#39607,
#39608,#39609,#39610,#39611),.UNSPECIFIED.,.F.,.F.,(4,3,3,3,3,3,3,3,3,3,
4),(0.754355313185423,0.781440569694544,0.818270933113877,1.26008190551097,
1.48098739170952,1.70189287790806,1.73520393204287,1.87436956924915,2.5497012294929,
2.66225650620019,2.77481178290748),.UNSPECIFIED.);
#651=B_SPLINE_CURVE_WITH_KNOTS('',3,(#39613,#39614,#39615,#39616),
 .UNSPECIFIED.,.F.,.F.,(4,4),(-2.23164162261785,-2.15648187025204),
 .UNSPECIFIED.);
#652=B_SPLINE_CURVE_WITH_KNOTS('',3,(#39787,#39788,#39789,#39790),
 .UNSPECIFIED.,.F.,.F.,(4,4),(1.90569248523429,2.03375105473527),
 .UNSPECIFIED.);
#653=B_SPLINE_CURVE_WITH_KNOTS('',3,(#39792,#39793,#39794,#39795,#39796,
#39797,#39798,#39799,#39800,#39801),.UNSPECIFIED.,.F.,.F.,(4,2,1,1,2,4),
(-2.76222327472563,-2.70245118401238,-2.29230817720288,-2.08723667379812,
-1.67709366698862,-1.61732157627537),.UNSPECIFIED.);
#654=B_SPLINE_CURVE_WITH_KNOTS('',3,(#39803,#39804,#39805,#39806),
 .UNSPECIFIED.,.F.,.F.,(4,4),(1.10784159885378,1.2359001683555),
 .UNSPECIFIED.);
#655=B_SPLINE_CURVE_WITH_KNOTS('',3,(#39810,#39811,#39812,#39813),
 .UNSPECIFIED.,.F.,.F.,(4,4),(1.90569248523429,2.03375105473527),
 .UNSPECIFIED.);
#656=B_SPLINE_CURVE_WITH_KNOTS('',3,(#39815,#39816,#39817,#39818,#39819,
#39820,#39821,#39822,#39823,#39824),.UNSPECIFIED.,.F.,.F.,(4,2,1,1,2,4),
(-2.76222327472562,-2.70245118401238,-2.29230817720287,-2.08723667379812,
-1.67709366698862,-1.61732157627537),.UNSPECIFIED.);
#657=B_SPLINE_CURVE_WITH_KNOTS('',3,(#39826,#39827,#39828,#39829),
 .UNSPECIFIED.,.F.,.F.,(4,4),(1.10784159885377,1.23590016835549),
 .UNSPECIFIED.);
#658=B_SPLINE_CURVE_WITH_KNOTS('',3,(#39900,#39901,#39902,#39903),
 .UNSPECIFIED.,.F.,.F.,(4,4),(-1.23590016835551,-1.10784159885453),
 .UNSPECIFIED.);
#659=B_SPLINE_CURVE_WITH_KNOTS('',3,(#39905,#39906,#39907,#39908,#39909,
#39910,#39911,#39912,#39913,#39914),.UNSPECIFIED.,.F.,.F.,(4,2,1,1,2,4),
(-2.76222327472564,-2.70245118401238,-2.29230817720287,-2.08723667379812,
-1.67709366698862,-1.61732157627537),.UNSPECIFIED.);
#660=B_SPLINE_CURVE_WITH_KNOTS('',3,(#39916,#39917,#39918,#39919),
 .UNSPECIFIED.,.F.,.F.,(4,4),(-2.03375105473599,-1.9056924852343),
 .UNSPECIFIED.);
#661=B_SPLINE_CURVE_WITH_KNOTS('',3,(#39923,#39924,#39925,#39926),
 .UNSPECIFIED.,.F.,.F.,(4,4),(-1.2359001683555,-1.10784159885453),
 .UNSPECIFIED.);
#662=B_SPLINE_CURVE_WITH_KNOTS('',3,(#39928,#39929,#39930,#39931,#39932,
#39933,#39934,#39935,#39936,#39937,#39938),.UNSPECIFIED.,.F.,.F.,(4,2,1,
1,1,2,4),(-2.76222327472563,-2.70245118401238,-2.49737968060763,-2.39484392890525,
-2.08723667379813,-1.67709366698862,-1.61732157627537),.UNSPECIFIED.);
#663=B_SPLINE_CURVE_WITH_KNOTS('',3,(#39940,#39941,#39942,#39943),
 .UNSPECIFIED.,.F.,.F.,(4,4),(-2.03375105473601,-1.9056924852343),
 .UNSPECIFIED.);
#664=B_SPLINE_CURVE_WITH_KNOTS('',3,(#40011,#40012,#40013,#40014,#40015,
#40016,#40017,#40018,#40019,#40020),.UNSPECIFIED.,.F.,.F.,(4,2,1,1,2,4),
(1.61732157627537,1.67709366698862,2.08723667379812,2.29230817720287,2.70245118401238,
2.76222327472564),.UNSPECIFIED.);
#665=B_SPLINE_CURVE_WITH_KNOTS('',3,(#40045,#40046,#40047,#40048),
 .UNSPECIFIED.,.F.,.F.,(4,4),(1.9056924852343,2.03375105473599),
 .UNSPECIFIED.);
#666=B_SPLINE_CURVE_WITH_KNOTS('',3,(#40065,#40066,#40067,#40068),
 .UNSPECIFIED.,.F.,.F.,(4,4),(1.10784159885453,1.23590016835551),
 .UNSPECIFIED.);
#667=B_SPLINE_CURVE_WITH_KNOTS('',3,(#40075,#40076,#40077,#40078),
 .UNSPECIFIED.,.F.,.F.,(4,4),(-0.985110783337744,-0.909951030971936),
 .UNSPECIFIED.);
#668=B_SPLINE_CURVE_WITH_KNOTS('',3,(#40080,#40081,#40082,#40083,#40084,
#40085,#40086,#40087,#40088,#40089,#40090,#40091,#40092,#40093,#40094,#40095,
#40096,#40097,#40098,#40099,#40100,#40101,#40102,#40103,#40104,#40105,#40106,
#40107,#40108,#40109,#40110,#40111,#40112,#40113),.UNSPECIFIED.,.F.,.F.,
(4,3,3,3,3,3,3,3,3,3,3,4),(0.754355313185457,0.781440569694525,0.818270933113784,
1.26008190551044,1.48098739170876,1.70189287790709,1.73520393204254,1.80044174678674,
1.87436956924505,2.54970122949192,2.66225650619973,2.77481178290754),
 .UNSPECIFIED.);
#669=B_SPLINE_CURVE_WITH_KNOTS('',3,(#40115,#40116,#40117,#40118),
 .UNSPECIFIED.,.F.,.F.,(4,4),(-2.23164162261785,-2.15648187025204),
 .UNSPECIFIED.);
#670=B_SPLINE_CURVE_WITH_KNOTS('',3,(#40161,#40162,#40163,#40164),
 .UNSPECIFIED.,.F.,.F.,(4,4),(-0.985110783337753,-0.90995103097194),
 .UNSPECIFIED.);
#671=B_SPLINE_CURVE_WITH_KNOTS('',3,(#40166,#40167,#40168,#40169,#40170,
#40171,#40172,#40173,#40174,#40175),.UNSPECIFIED.,.F.,.F.,(4,3,3,4),(-1.16153810946444,
-0.819783369909333,-0.782081488746978,-0.754355313185483),.UNSPECIFIED.);
#672=B_SPLINE_CURVE_WITH_KNOTS('',3,(#40177,#40178,#40179,#40180,#40181,
#40182,#40183,#40184,#40185,#40186,#40187,#40188,#40189,#40190),
 .UNSPECIFIED.,.F.,.F.,(4,2,2,2,2,2,4),(-2.39249786125564,-1.89936032174935,
-1.8254413803293,-1.76021140268281,-1.72690435024458,-1.65779202010542,
-1.17747397511189),.UNSPECIFIED.);
#673=B_SPLINE_CURVE_WITH_KNOTS('',3,(#40192,#40193,#40194,#40195,#40196,
#40197),.UNSPECIFIED.,.F.,.F.,(4,1,1,4),(-2.79969436419745,-2.68715260889144,
-2.57461085358543,-2.39249786125564),.UNSPECIFIED.);
#674=B_SPLINE_CURVE_WITH_KNOTS('',3,(#40199,#40200,#40201,#40202),
 .UNSPECIFIED.,.F.,.F.,(4,4),(-2.23164162261786,-2.15648187025205),
 .UNSPECIFIED.);
#675=B_SPLINE_CURVE_WITH_KNOTS('',3,(#40206,#40207,#40208,#40209),
 .UNSPECIFIED.,.F.,.F.,(4,4),(-0.985110783337756,-0.90995103097194),
 .UNSPECIFIED.);
#676=B_SPLINE_CURVE_WITH_KNOTS('',3,(#40211,#40212,#40213,#40214,#40215,
#40216,#40217,#40218,#40219,#40220),.UNSPECIFIED.,.F.,.F.,(4,3,3,4),(-1.16153810946435,
-0.819783369909053,-0.782081488746808,-0.754355313185456),.UNSPECIFIED.);
#677=B_SPLINE_CURVE_WITH_KNOTS('',3,(#40222,#40223,#40224,#40225,#40226,
#40227,#40228,#40229,#40230,#40231,#40232,#40233,#40234,#40235,#40236),
 .UNSPECIFIED.,.F.,.F.,(4,2,2,2,2,2,1,4),(-2.39250890756776,-2.00158942999731,
-1.89936032174878,-1.76021140268269,-1.72690435024413,-1.65779202010392,
-1.45419115408438,-1.17754443036329),.UNSPECIFIED.);
#678=B_SPLINE_CURVE_WITH_KNOTS('',3,(#40238,#40239,#40240,#40241,#40242),
 .UNSPECIFIED.,.F.,.F.,(4,1,4),(-2.79969436419747,-2.60016813064743,-2.39250890756776),
 .UNSPECIFIED.);
#679=B_SPLINE_CURVE_WITH_KNOTS('',3,(#40244,#40245,#40246,#40247),
 .UNSPECIFIED.,.F.,.F.,(4,4),(-2.17250154753575,-2.15648187025205),
 .UNSPECIFIED.);
#680=B_SPLINE_CURVE_WITH_KNOTS('',3,(#40249,#40250,#40251,#40252),
 .UNSPECIFIED.,.F.,.F.,(4,4),(-2.23164162261787,-2.17250154753575),
 .UNSPECIFIED.);
#681=B_SPLINE_CURVE_WITH_KNOTS('',3,(#40297,#40298,#40299,#40300),
 .UNSPECIFIED.,.F.,.F.,(4,4),(2.15648187025204,2.23164162261785),
 .UNSPECIFIED.);
#682=B_SPLINE_CURVE_WITH_KNOTS('',3,(#40302,#40303,#40304,#40305,#40306,
#40307,#40308,#40309,#40310,#40311),.UNSPECIFIED.,.F.,.F.,(4,3,3,4),(-1.1615381094643,
-0.819783369909086,-0.782081488746884,-0.754355313185452),.UNSPECIFIED.);
#683=B_SPLINE_CURVE_WITH_KNOTS('',3,(#40313,#40314,#40315,#40316,#40317,
#40318,#40319,#40320,#40321,#40322,#40323,#40324,#40325,#40326,#40327,#40328),
 .UNSPECIFIED.,.F.,.F.,(4,2,2,2,2,2,2,4),(-2.39249643071187,-2.00158942999732,
-1.89936032174887,-1.82544138032896,-1.76021140268264,-1.72690435024399,
-1.65779202010374,-1.1774981323703),.UNSPECIFIED.);
#684=B_SPLINE_CURVE_WITH_KNOTS('',3,(#40330,#40331,#40332,#40333,#40334),
 .UNSPECIFIED.,.F.,.F.,(4,1,4),(-2.79969436419746,-2.60016813064742,-2.39249643071187),
 .UNSPECIFIED.);
#685=B_SPLINE_CURVE_WITH_KNOTS('',3,(#40335,#40336,#40337,#40338),
 .UNSPECIFIED.,.F.,.F.,(4,4),(0.90995103097193,0.985110783337743),
 .UNSPECIFIED.);
#686=B_SPLINE_CURVE_WITH_KNOTS('',3,(#40340,#40341,#40342,#40343),
 .UNSPECIFIED.,.F.,.F.,(4,4),(2.15648187025204,2.23164162261785),
 .UNSPECIFIED.);
#687=B_SPLINE_CURVE_WITH_KNOTS('',3,(#40345,#40346,#40347,#40348,#40349,
#40350,#40351,#40352,#40353,#40354),.UNSPECIFIED.,.F.,.F.,(4,3,3,4),(-1.16153810946437,
-0.819783369909201,-0.782081488746912,-0.754355313185438),.UNSPECIFIED.);
#688=B_SPLINE_CURVE_WITH_KNOTS('',3,(#40356,#40357,#40358,#40359,#40360,
#40361,#40362,#40363,#40364,#40365,#40366,#40367,#40368,#40369),
 .UNSPECIFIED.,.F.,.F.,(4,2,2,2,2,1,1,4),(-2.39247844687041,-1.89936032174889,
-1.82544138032945,-1.76021140268296,-1.7269043502448,-1.50602540169013,
-1.28514645313547,-1.17750545093659),.UNSPECIFIED.);
#689=B_SPLINE_CURVE_WITH_KNOTS('',3,(#40371,#40372,#40373,#40374,#40375,
#40376),.UNSPECIFIED.,.F.,.F.,(4,1,1,4),(-2.79969436419745,-2.68715260889138,
-2.57461085358531,-2.39247844687041),.UNSPECIFIED.);
#690=B_SPLINE_CURVE_WITH_KNOTS('',3,(#40378,#40379,#40380,#40381),
 .UNSPECIFIED.,.F.,.F.,(4,4),(0.969091106047469,0.985110783337744),
 .UNSPECIFIED.);
#691=B_SPLINE_CURVE_WITH_KNOTS('',3,(#40382,#40383,#40384,#40385),
 .UNSPECIFIED.,.F.,.F.,(4,4),(0.909951030971929,0.969091106047469),
 .UNSPECIFIED.);
#692=B_SPLINE_CURVE_WITH_KNOTS('',3,(#40555,#40556,#40557,#40558,#40559,
#40560,#40561,#40562,#40563,#40564),.UNSPECIFIED.,.F.,.F.,(4,2,1,1,2,4),
(1.61732157627537,1.67709366698862,2.08723667379812,2.29230817720288,2.70245118401238,
2.76222327472563),.UNSPECIFIED.);
#693=B_SPLINE_CURVE_WITH_KNOTS('',3,(#40581,#40582,#40583,#40584),
 .UNSPECIFIED.,.F.,.F.,(4,4),(-2.03375105473527,-1.90569248523429),
 .UNSPECIFIED.);
#694=B_SPLINE_CURVE_WITH_KNOTS('',3,(#40601,#40602,#40603,#40604),
 .UNSPECIFIED.,.F.,.F.,(4,4),(-1.2359001683555,-1.10784159885378),
 .UNSPECIFIED.);
#695=B_SPLINE_CURVE_WITH_KNOTS('',3,(#40611,#40612,#40613,#40614),
 .UNSPECIFIED.,.F.,.F.,(4,4),(2.15648187025205,2.23164162261786),
 .UNSPECIFIED.);
#696=B_SPLINE_CURVE_WITH_KNOTS('',3,(#40616,#40617,#40618,#40619,#40620,
#40621,#40622,#40623,#40624,#40625,#40626,#40627,#40628,#40629,#40630,#40631,
#40632,#40633,#40634,#40635,#40636,#40637,#40638,#40639,#40640,#40641,#40642,
#40643,#40644,#40645,#40646),.UNSPECIFIED.,.F.,.F.,(4,3,3,3,3,3,3,3,3,3,
4),(0.754355313185418,0.781440569694357,0.818270933113567,1.4291469164439,
1.63277224422068,1.70189287790631,1.73520393204215,1.87436956924478,1.97661095987539,
2.57526157714918,2.77481178290704),.UNSPECIFIED.);
#697=B_SPLINE_CURVE_WITH_KNOTS('',3,(#40648,#40649,#40650,#40651),
 .UNSPECIFIED.,.F.,.F.,(4,4),(0.90995103097194,0.985110783337756),
 .UNSPECIFIED.);
#698=B_SPLINE_CURVE_WITH_KNOTS('',3,(#40818,#40819,#40820,#40821,#40822,
#40823,#40824,#40825,#40826,#40827,#40828),.UNSPECIFIED.,.F.,.F.,(4,2,1,
1,1,2,4),(1.61732157627537,1.67709366698862,2.08723667379813,2.39484392890525,
2.49737968060763,2.70245118401238,2.76222327472563),.UNSPECIFIED.);
#699=B_SPLINE_CURVE_WITH_KNOTS('',3,(#40853,#40854,#40855,#40856),
 .UNSPECIFIED.,.F.,.F.,(4,4),(1.9056924852343,2.03375105473601),
 .UNSPECIFIED.);
#700=B_SPLINE_CURVE_WITH_KNOTS('',3,(#40873,#40874,#40875,#40876),
 .UNSPECIFIED.,.F.,.F.,(4,4),(1.10784159885453,1.2359001683555),
 .UNSPECIFIED.);
#701=B_SPLINE_CURVE_WITH_KNOTS('',3,(#40883,#40884,#40885,#40886),
 .UNSPECIFIED.,.F.,.F.,(4,4),(-0.985110783337743,-0.909951030971934),
 .UNSPECIFIED.);
#702=B_SPLINE_CURVE_WITH_KNOTS('',3,(#40888,#40889,#40890,#40891,#40892,
#40893,#40894,#40895,#40896,#40897,#40898,#40899,#40900,#40901,#40902,#40903,
#40904,#40905,#40906,#40907,#40908,#40909,#40910,#40911,#40912,#40913,#40914,
#40915,#40916,#40917,#40918),.UNSPECIFIED.,.F.,.F.,(4,3,3,3,3,3,3,3,3,3,
4),(0.754355313185433,0.781440569694449,0.818270933113629,1.63277224422067,
1.70189287790637,1.7352039320423,1.80044174678633,1.87436956924509,1.97661095987564,
2.57526157714951,2.77481178290747),.UNSPECIFIED.);
#703=B_SPLINE_CURVE_WITH_KNOTS('',3,(#40920,#40921,#40922,#40923),
 .UNSPECIFIED.,.F.,.F.,(4,4),(-2.23164162261785,-2.15648187025204),
 .UNSPECIFIED.);
#704=B_SPLINE_CURVE_WITH_KNOTS('',3,(#41098,#41099,#41100,#41101,#41102,
#41103,#41104,#41105,#41106,#41107),.UNSPECIFIED.,.F.,.F.,(4,2,1,1,2,4),
(1.61732157627537,1.67709366698862,2.08723667379812,2.29230817720287,2.70245118401238,
2.76222327472562),.UNSPECIFIED.);
#705=B_SPLINE_CURVE_WITH_KNOTS('',3,(#41124,#41125,#41126,#41127),
 .UNSPECIFIED.,.F.,.F.,(4,4),(-2.03375105473527,-1.90569248523429),
 .UNSPECIFIED.);
#706=B_SPLINE_CURVE_WITH_KNOTS('',3,(#41144,#41145,#41146,#41147),
 .UNSPECIFIED.,.F.,.F.,(4,4),(-1.23590016835549,-1.10784159885377),
 .UNSPECIFIED.);
#707=B_SPLINE_CURVE_WITH_KNOTS('',3,(#41154,#41155,#41156,#41157),
 .UNSPECIFIED.,.F.,.F.,(4,4),(2.15648187025205,2.23164162261786),
 .UNSPECIFIED.);
#708=B_SPLINE_CURVE_WITH_KNOTS('',3,(#41159,#41160,#41161,#41162,#41163,
#41164,#41165,#41166,#41167,#41168,#41169,#41170,#41171,#41172,#41173,#41174,
#41175,#41176,#41177,#41178,#41179,#41180,#41181,#41182,#41183,#41184,#41185,
#41186,#41187,#41188,#41189),.UNSPECIFIED.,.F.,.F.,(4,3,3,3,3,3,3,3,3,3,
4),(0.754355313185446,0.781440569694518,0.818270933113847,1.6327722442224,
1.701892877907,1.73520393204251,1.8004417467867,1.87436956924561,2.54970122949198,
2.6622565061997,2.77481178290743),.UNSPECIFIED.);
#709=B_SPLINE_CURVE_WITH_KNOTS('',3,(#41191,#41192,#41193,#41194),
 .UNSPECIFIED.,.F.,.F.,(4,4),(0.90995103097194,0.985110783337753),
 .UNSPECIFIED.);
#710=B_SPLINE_CURVE_WITH_KNOTS('',2,(#41352,#41353,#41354),
 .UNSPECIFIED.,.F.,.F.,(3,3),(0.,1.),.UNSPECIFIED.);
#711=B_SPLINE_CURVE_WITH_KNOTS('',2,(#41358,#41359,#41360),
 .UNSPECIFIED.,.F.,.F.,(3,3),(0.,1.),.UNSPECIFIED.);
#712=B_SPLINE_CURVE_WITH_KNOTS('',2,(#41369,#41370,#41371),
 .UNSPECIFIED.,.F.,.F.,(3,3),(0.,1.),.UNSPECIFIED.);
#713=B_SPLINE_CURVE_WITH_KNOTS('',2,(#41374,#41375,#41376),
 .UNSPECIFIED.,.F.,.F.,(3,3),(0.,1.),.UNSPECIFIED.);
#714=B_SPLINE_CURVE_WITH_KNOTS('',2,(#41384,#41385,#41386),
 .UNSPECIFIED.,.F.,.F.,(3,3),(0.,1.),.UNSPECIFIED.);
#715=B_SPLINE_CURVE_WITH_KNOTS('',2,(#41389,#41390,#41391),
 .UNSPECIFIED.,.F.,.F.,(3,3),(0.,1.),.UNSPECIFIED.);
#716=B_SPLINE_CURVE_WITH_KNOTS('',2,(#41399,#41400,#41401),
 .UNSPECIFIED.,.F.,.F.,(3,3),(0.,1.),.UNSPECIFIED.);
#717=B_SPLINE_CURVE_WITH_KNOTS('',2,(#41404,#41405,#41406),
 .UNSPECIFIED.,.F.,.F.,(3,3),(0.,1.),.UNSPECIFIED.);
#718=B_SPLINE_CURVE_WITH_KNOTS('',2,(#41414,#41415,#41416),
 .UNSPECIFIED.,.F.,.F.,(3,3),(0.,1.),.UNSPECIFIED.);
#719=B_SPLINE_CURVE_WITH_KNOTS('',2,(#41419,#41420,#41421),
 .UNSPECIFIED.,.F.,.F.,(3,3),(0.,1.),.UNSPECIFIED.);
#720=B_SPLINE_CURVE_WITH_KNOTS('',2,(#41429,#41430,#41431),
 .UNSPECIFIED.,.F.,.F.,(3,3),(0.,1.),.UNSPECIFIED.);
#721=B_SPLINE_CURVE_WITH_KNOTS('',2,(#41434,#41435,#41436),
 .UNSPECIFIED.,.F.,.F.,(3,3),(0.,1.),.UNSPECIFIED.);
#722=B_SPLINE_CURVE_WITH_KNOTS('',2,(#41444,#41445,#41446),
 .UNSPECIFIED.,.F.,.F.,(3,3),(0.,1.),.UNSPECIFIED.);
#723=B_SPLINE_CURVE_WITH_KNOTS('',2,(#41449,#41450,#41451),
 .UNSPECIFIED.,.F.,.F.,(3,3),(0.,1.),.UNSPECIFIED.);
#724=B_SPLINE_CURVE_WITH_KNOTS('',2,(#41458,#41459,#41460),
 .UNSPECIFIED.,.F.,.F.,(3,3),(0.,1.),.UNSPECIFIED.);
#725=B_SPLINE_CURVE_WITH_KNOTS('',2,(#41461,#41462,#41463),
 .UNSPECIFIED.,.F.,.F.,(3,3),(0.,1.),.UNSPECIFIED.);
#726=B_SPLINE_CURVE_WITH_KNOTS('',2,(#41473,#41474,#41475),
 .UNSPECIFIED.,.F.,.F.,(3,3),(0.,1.),.UNSPECIFIED.);
#727=B_SPLINE_CURVE_WITH_KNOTS('',2,(#41485,#41486,#41487),
 .UNSPECIFIED.,.F.,.F.,(3,3),(0.,1.),.UNSPECIFIED.);
#728=B_SPLINE_CURVE_WITH_KNOTS('',2,(#41496,#41497,#41498),
 .UNSPECIFIED.,.F.,.F.,(3,3),(0.,1.),.UNSPECIFIED.);
#729=B_SPLINE_CURVE_WITH_KNOTS('',2,(#41507,#41508,#41509),
 .UNSPECIFIED.,.F.,.F.,(3,3),(0.,1.),.UNSPECIFIED.);
#730=B_SPLINE_CURVE_WITH_KNOTS('',2,(#41518,#41519,#41520),
 .UNSPECIFIED.,.F.,.F.,(3,3),(0.,1.),.UNSPECIFIED.);
#731=B_SPLINE_CURVE_WITH_KNOTS('',2,(#41529,#41530,#41531),
 .UNSPECIFIED.,.F.,.F.,(3,3),(0.,1.),.UNSPECIFIED.);
#732=B_SPLINE_CURVE_WITH_KNOTS('',2,(#41540,#41541,#41542),
 .UNSPECIFIED.,.F.,.F.,(3,3),(0.,1.),.UNSPECIFIED.);
#733=B_SPLINE_CURVE_WITH_KNOTS('',2,(#41551,#41552,#41553),
 .UNSPECIFIED.,.F.,.F.,(3,3),(0.,1.),.UNSPECIFIED.);
#734=B_SPLINE_CURVE_WITH_KNOTS('',2,(#41562,#41563,#41564),
 .UNSPECIFIED.,.F.,.F.,(3,3),(0.,1.),.UNSPECIFIED.);
#735=B_SPLINE_CURVE_WITH_KNOTS('',2,(#41571,#41572,#41573),
 .UNSPECIFIED.,.F.,.F.,(3,3),(0.,1.),.UNSPECIFIED.);
#736=B_SPLINE_CURVE_WITH_KNOTS('',2,(#41616,#41617,#41618),
 .UNSPECIFIED.,.F.,.F.,(3,3),(0.,1.),.UNSPECIFIED.);
#737=B_SPLINE_CURVE_WITH_KNOTS('',2,(#41622,#41623,#41624),
 .UNSPECIFIED.,.F.,.F.,(3,3),(0.,1.),.UNSPECIFIED.);
#738=B_SPLINE_CURVE_WITH_KNOTS('',2,(#41633,#41634,#41635),
 .UNSPECIFIED.,.F.,.F.,(3,3),(0.,1.),.UNSPECIFIED.);
#739=B_SPLINE_CURVE_WITH_KNOTS('',2,(#41638,#41639,#41640),
 .UNSPECIFIED.,.F.,.F.,(3,3),(0.,1.),.UNSPECIFIED.);
#740=B_SPLINE_CURVE_WITH_KNOTS('',2,(#41648,#41649,#41650),
 .UNSPECIFIED.,.F.,.F.,(3,3),(0.,1.),.UNSPECIFIED.);
#741=B_SPLINE_CURVE_WITH_KNOTS('',2,(#41653,#41654,#41655),
 .UNSPECIFIED.,.F.,.F.,(3,3),(0.,1.),.UNSPECIFIED.);
#742=B_SPLINE_CURVE_WITH_KNOTS('',2,(#41663,#41664,#41665),
 .UNSPECIFIED.,.F.,.F.,(3,3),(0.,1.),.UNSPECIFIED.);
#743=B_SPLINE_CURVE_WITH_KNOTS('',2,(#41668,#41669,#41670),
 .UNSPECIFIED.,.F.,.F.,(3,3),(0.,1.),.UNSPECIFIED.);
#744=B_SPLINE_CURVE_WITH_KNOTS('',2,(#41678,#41679,#41680),
 .UNSPECIFIED.,.F.,.F.,(3,3),(0.,1.),.UNSPECIFIED.);
#745=B_SPLINE_CURVE_WITH_KNOTS('',2,(#41683,#41684,#41685),
 .UNSPECIFIED.,.F.,.F.,(3,3),(0.,1.),.UNSPECIFIED.);
#746=B_SPLINE_CURVE_WITH_KNOTS('',2,(#41693,#41694,#41695),
 .UNSPECIFIED.,.F.,.F.,(3,3),(0.,1.),.UNSPECIFIED.);
#747=B_SPLINE_CURVE_WITH_KNOTS('',2,(#41698,#41699,#41700),
 .UNSPECIFIED.,.F.,.F.,(3,3),(0.,1.),.UNSPECIFIED.);
#748=B_SPLINE_CURVE_WITH_KNOTS('',2,(#41708,#41709,#41710),
 .UNSPECIFIED.,.F.,.F.,(3,3),(0.,1.),.UNSPECIFIED.);
#749=B_SPLINE_CURVE_WITH_KNOTS('',2,(#41713,#41714,#41715),
 .UNSPECIFIED.,.F.,.F.,(3,3),(0.,1.),.UNSPECIFIED.);
#750=B_SPLINE_CURVE_WITH_KNOTS('',2,(#41723,#41724,#41725),
 .UNSPECIFIED.,.F.,.F.,(3,3),(0.,1.),.UNSPECIFIED.);
#751=B_SPLINE_CURVE_WITH_KNOTS('',2,(#41728,#41729,#41730),
 .UNSPECIFIED.,.F.,.F.,(3,3),(0.,1.),.UNSPECIFIED.);
#752=B_SPLINE_CURVE_WITH_KNOTS('',2,(#41737,#41738,#41739),
 .UNSPECIFIED.,.F.,.F.,(3,3),(0.,1.),.UNSPECIFIED.);
#753=B_SPLINE_CURVE_WITH_KNOTS('',2,(#41740,#41741,#41742),
 .UNSPECIFIED.,.F.,.F.,(3,3),(0.,1.),.UNSPECIFIED.);
#754=B_SPLINE_CURVE_WITH_KNOTS('',2,(#41752,#41753,#41754),
 .UNSPECIFIED.,.F.,.F.,(3,3),(0.,1.),.UNSPECIFIED.);
#755=B_SPLINE_CURVE_WITH_KNOTS('',2,(#41764,#41765,#41766),
 .UNSPECIFIED.,.F.,.F.,(3,3),(0.,1.),.UNSPECIFIED.);
#756=B_SPLINE_CURVE_WITH_KNOTS('',2,(#41775,#41776,#41777),
 .UNSPECIFIED.,.F.,.F.,(3,3),(0.,1.),.UNSPECIFIED.);
#757=B_SPLINE_CURVE_WITH_KNOTS('',2,(#41786,#41787,#41788),
 .UNSPECIFIED.,.F.,.F.,(3,3),(0.,1.),.UNSPECIFIED.);
#758=B_SPLINE_CURVE_WITH_KNOTS('',2,(#41797,#41798,#41799),
 .UNSPECIFIED.,.F.,.F.,(3,3),(0.,1.),.UNSPECIFIED.);
#759=B_SPLINE_CURVE_WITH_KNOTS('',2,(#41808,#41809,#41810),
 .UNSPECIFIED.,.F.,.F.,(3,3),(0.,1.),.UNSPECIFIED.);
#760=B_SPLINE_CURVE_WITH_KNOTS('',2,(#41819,#41820,#41821),
 .UNSPECIFIED.,.F.,.F.,(3,3),(0.,1.),.UNSPECIFIED.);
#761=B_SPLINE_CURVE_WITH_KNOTS('',2,(#41830,#41831,#41832),
 .UNSPECIFIED.,.F.,.F.,(3,3),(0.,1.),.UNSPECIFIED.);
#762=B_SPLINE_CURVE_WITH_KNOTS('',2,(#41841,#41842,#41843),
 .UNSPECIFIED.,.F.,.F.,(3,3),(0.,1.),.UNSPECIFIED.);
#763=B_SPLINE_CURVE_WITH_KNOTS('',2,(#41852,#41853,#41854),
 .UNSPECIFIED.,.F.,.F.,(3,3),(0.,1.),.UNSPECIFIED.);
#764=B_SPLINE_CURVE_WITH_KNOTS('',2,(#41863,#41864,#41865),
 .UNSPECIFIED.,.F.,.F.,(3,3),(0.,1.),.UNSPECIFIED.);
#765=B_SPLINE_CURVE_WITH_KNOTS('',2,(#41874,#41875,#41876),
 .UNSPECIFIED.,.F.,.F.,(3,3),(0.,1.),.UNSPECIFIED.);
#766=B_SPLINE_CURVE_WITH_KNOTS('',2,(#41883,#41884,#41885),
 .UNSPECIFIED.,.F.,.F.,(3,3),(0.,1.),.UNSPECIFIED.);
#767=B_SPLINE_CURVE_WITH_KNOTS('',2,(#41901,#41902,#41903),
 .UNSPECIFIED.,.F.,.F.,(3,3),(0.,1.),.UNSPECIFIED.);
#768=B_SPLINE_CURVE_WITH_KNOTS('',2,(#41912,#41913,#41914),
 .UNSPECIFIED.,.F.,.F.,(3,3),(0.,1.),.UNSPECIFIED.);
#769=B_SPLINE_CURVE_WITH_KNOTS('',2,(#41923,#41924,#41925),
 .UNSPECIFIED.,.F.,.F.,(3,3),(0.,1.),.UNSPECIFIED.);
#770=B_SPLINE_CURVE_WITH_KNOTS('',2,(#41934,#41935,#41936),
 .UNSPECIFIED.,.F.,.F.,(3,3),(0.,1.),.UNSPECIFIED.);
#771=B_SPLINE_CURVE_WITH_KNOTS('',2,(#41945,#41946,#41947),
 .UNSPECIFIED.,.F.,.F.,(3,3),(0.,1.),.UNSPECIFIED.);
#772=B_SPLINE_CURVE_WITH_KNOTS('',2,(#41956,#41957,#41958),
 .UNSPECIFIED.,.F.,.F.,(3,3),(0.,1.),.UNSPECIFIED.);
#773=B_SPLINE_CURVE_WITH_KNOTS('',2,(#41967,#41968,#41969),
 .UNSPECIFIED.,.F.,.F.,(3,3),(0.,1.),.UNSPECIFIED.);
#774=B_SPLINE_CURVE_WITH_KNOTS('',2,(#41978,#41979,#41980),
 .UNSPECIFIED.,.F.,.F.,(3,3),(0.,1.),.UNSPECIFIED.);
#775=B_SPLINE_CURVE_WITH_KNOTS('',2,(#41989,#41990,#41991),
 .UNSPECIFIED.,.F.,.F.,(3,3),(0.,1.),.UNSPECIFIED.);
#776=B_SPLINE_CURVE_WITH_KNOTS('',2,(#42000,#42001,#42002),
 .UNSPECIFIED.,.F.,.F.,(3,3),(0.,1.),.UNSPECIFIED.);
#777=B_SPLINE_CURVE_WITH_KNOTS('',2,(#42015,#42016,#42017),
 .UNSPECIFIED.,.F.,.F.,(3,3),(0.,1.),.UNSPECIFIED.);
#778=B_SPLINE_CURVE_WITH_KNOTS('',2,(#42026,#42027,#42028),
 .UNSPECIFIED.,.F.,.F.,(3,3),(0.,1.),.UNSPECIFIED.);
#779=B_SPLINE_CURVE_WITH_KNOTS('',2,(#42037,#42038,#42039),
 .UNSPECIFIED.,.F.,.F.,(3,3),(0.,1.),.UNSPECIFIED.);
#780=B_SPLINE_CURVE_WITH_KNOTS('',2,(#42048,#42049,#42050),
 .UNSPECIFIED.,.F.,.F.,(3,3),(0.,1.),.UNSPECIFIED.);
#781=B_SPLINE_CURVE_WITH_KNOTS('',2,(#42059,#42060,#42061),
 .UNSPECIFIED.,.F.,.F.,(3,3),(0.,1.),.UNSPECIFIED.);
#782=B_SPLINE_CURVE_WITH_KNOTS('',2,(#42070,#42071,#42072),
 .UNSPECIFIED.,.F.,.F.,(3,3),(0.,1.),.UNSPECIFIED.);
#783=B_SPLINE_CURVE_WITH_KNOTS('',2,(#42081,#42082,#42083),
 .UNSPECIFIED.,.F.,.F.,(3,3),(0.,1.),.UNSPECIFIED.);
#784=B_SPLINE_CURVE_WITH_KNOTS('',2,(#42092,#42093,#42094),
 .UNSPECIFIED.,.F.,.F.,(3,3),(0.,1.),.UNSPECIFIED.);
#785=B_SPLINE_CURVE_WITH_KNOTS('',3,(#44024,#44025,#44026,#44027,#44028,
#44029,#44030,#44031,#44032,#44033,#44034,#44035,#44036,#44037,#44038,#44039),
 .UNSPECIFIED.,.F.,.F.,(4,3,3,3,3,4),(-4.09305997722772,-3.86695282144916,
-3.38358371876801,-2.90021461608687,-2.41684551340572,-2.07420913009921),
 .UNSPECIFIED.);
#786=B_SPLINE_CURVE_WITH_KNOTS('',3,(#44042,#44043,#44044,#44045,#44046,
#44047,#44048,#44049,#44050,#44051),.UNSPECIFIED.,.F.,.F.,(4,3,3,4),(0.,
0.483369102681141,0.966738205362282,1.12274180646098),.UNSPECIFIED.);
#787=B_SPLINE_CURVE_WITH_KNOTS('',3,(#44056,#44057,#44058,#44059,#44060,
#44061,#44062,#44063,#44064,#44065,#44066,#44067,#44068,#44069,#44070,#44071,
#44072,#44073,#44074,#44075,#44076,#44077,#44078,#44079,#44080,#44081,#44082,
#44083,#44084,#44085,#44086,#44087,#44088,#44089,#44090,#44091,#44092,#44093,
#44094,#44095,#44096,#44097,#44098),.UNSPECIFIED.,.F.,.F.,(4,3,3,3,3,3,
3,3,3,3,3,3,3,3,4),(-10.3762452844077,-10.150751156304,-9.6673820536229,
-9.18401295094176,-8.70064384826061,-8.21727474557946,-7.73390564289832,
-7.25053654021717,-6.76716743753603,-6.28379833485489,-5.80042923217374,
-5.3170601294926,-4.83369102681145,-4.35032192413031,-4.09305997722772),
 .UNSPECIFIED.);
#788=B_SPLINE_CURVE_WITH_KNOTS('',3,(#44099,#44100,#44101,#44102,#44103,
#44104,#44105,#44106,#44107,#44108,#44109,#44110,#44111,#44112,#44113,#44114,
#44115,#44116,#44117,#44118,#44119,#44120,#44121,#44122,#44123,#44124,#44125,
#44126,#44127,#44128,#44129,#44130,#44131,#44132,#44133,#44134,#44135,#44136,
#44137,#44138,#44139,#44140,#44141),.UNSPECIFIED.,.F.,.F.,(4,3,3,3,3,3,
3,3,3,3,3,3,3,3,4),(1.12274180646098,1.45010730804342,1.93347641072457,
2.41684551340571,2.90021461608685,3.38358371876799,3.86695282144913,4.35032192413027,
4.83369102681141,5.31706012949256,5.8004292321737,6.28379833485484,6.76716743753598,
7.25053654021712,7.40592711364047),.UNSPECIFIED.);
#789=B_SPLINE_CURVE_WITH_KNOTS('',3,(#44146,#44147,#44148,#44149,#44150,
#44151,#44152,#44153,#44154,#44155,#44156,#44157,#44158,#44159,#44160,#44161,
#44162,#44163,#44164,#44165,#44166,#44167,#44168,#44169,#44170,#44171,#44172,
#44173,#44174,#44175,#44176,#44177,#44178,#44179,#44180,#44181,#44182,#44183,
#44184,#44185,#44186,#44187,#44188),.UNSPECIFIED.,.F.,.F.,(4,3,3,3,3,3,
3,3,3,3,3,3,3,3,4),(-16.6594305915872,-16.4345494911589,-15.9511803884778,
-15.4678112857966,-14.9844421831155,-14.5010730804343,-14.0177039777532,
-13.5343348750721,-13.0509657723909,-12.5675966697098,-12.0842275670286,
-11.6008584643475,-11.1174893616663,-10.6341202589852,-10.3762452844077),
 .UNSPECIFIED.);
#790=B_SPLINE_CURVE_WITH_KNOTS('',3,(#44189,#44190,#44191,#44192,#44193,
#44194,#44195,#44196,#44197,#44198,#44199,#44200,#44201,#44202,#44203,#44204,
#44205,#44206,#44207,#44208,#44209,#44210,#44211,#44212,#44213,#44214,#44215,
#44216,#44217,#44218,#44219,#44220,#44221,#44222,#44223,#44224,#44225,#44226,
#44227,#44228,#44229,#44230,#44231),.UNSPECIFIED.,.F.,.F.,(4,3,3,3,3,3,
3,3,3,3,3,3,3,3,4),(7.40592711364047,7.73390564289826,8.2172747455794,8.70064384826054,
9.18401295094169,9.66738205362283,10.150751156304,10.6341202589851,11.1174893616663,
11.6008584643474,12.0842275670285,12.5675966697097,13.0509657723908,13.534334875072,
13.6891124208199),.UNSPECIFIED.);
#791=B_SPLINE_CURVE_WITH_KNOTS('',3,(#44236,#44237,#44238,#44239,#44240,
#44241,#44242,#44243,#44244,#44245,#44246,#44247,#44248,#44249,#44250,#44251,
#44252,#44253,#44254,#44255,#44256,#44257,#44258,#44259,#44260,#44261,#44262,
#44263,#44264,#44265,#44266,#44267,#44268,#44269,#44270,#44271,#44272,#44273,
#44274,#44275,#44276,#44277,#44278),.UNSPECIFIED.,.F.,.F.,(4,3,3,3,3,3,
3,3,3,3,3,3,3,3,4),(-22.9426158987667,-22.7183478260138,-22.2349787233327,
-21.7516096206515,-21.2682405179704,-20.7848714152892,-20.3015023126081,
-19.8181332099269,-19.3347641072458,-18.8513950045647,-18.3680259018835,
-17.8846567992024,-17.4012876965212,-16.9179185938401,-16.6594305915872),
 .UNSPECIFIED.);
#792=B_SPLINE_CURVE_WITH_KNOTS('',3,(#44279,#44280,#44281,#44282,#44283,
#44284,#44285,#44286,#44287,#44288,#44289,#44290,#44291,#44292,#44293,#44294,
#44295,#44296,#44297,#44298,#44299,#44300,#44301,#44302,#44303,#44304,#44305,
#44306,#44307,#44308,#44309,#44310,#44311,#44312,#44313,#44314,#44315,#44316,
#44317,#44318,#44319,#44320,#44321),.UNSPECIFIED.,.F.,.F.,(4,3,3,3,3,3,
3,3,3,3,3,3,3,3,4),(13.6891124208199,14.0177039777531,14.5010730804342,
14.9844421831154,15.4678112857965,15.9511803884777,16.4345494911588,16.9179185938399,
17.4012876965211,17.8846567992022,18.3680259018834,18.8513950045645,19.3347641072457,
19.8181332099268,19.9722977279999),.UNSPECIFIED.);
#793=B_SPLINE_CURVE_WITH_KNOTS('',3,(#44328,#44329,#44330,#44331,#44332,
#44333,#44334,#44335,#44336,#44337,#44338,#44339,#44340,#44341,#44342,#44343,
#44344,#44345,#44346,#44347,#44348,#44349,#44350,#44351,#44352,#44353,#44354,
#44355,#44356,#44357,#44358,#44359,#44360,#44361,#44362,#44363,#44364,#44365,
#44366,#44367),.UNSPECIFIED.,.F.,.F.,(4,3,3,3,3,3,3,3,3,3,3,3,3,4),(-29.0021461608684,
-28.5187770581875,-28.0354079555064,-27.5520388528253,-27.0686697501441,
-26.585300647463,-26.1019315447818,-25.6185624421007,-25.1351933394195,
-24.6518242367384,-24.1684551340572,-23.6850860313761,-23.201716928695,
-22.9426158987667),.UNSPECIFIED.);
#794=B_SPLINE_CURVE_WITH_KNOTS('',3,(#44368,#44369,#44370,#44371,#44372,
#44373,#44374,#44375,#44376,#44377,#44378,#44379,#44380,#44381,#44382,#44383,
#44384,#44385,#44386,#44387,#44388,#44389,#44390,#44391,#44392,#44393,#44394,
#44395,#44396,#44397,#44398,#44399,#44400,#44401,#44402,#44403,#44404,#44405,
#44406,#44407,#44408,#44409,#44410),.UNSPECIFIED.,.F.,.F.,(4,3,3,3,3,3,
3,3,3,3,3,3,3,3,4),(19.9722977279999,20.3015023126079,20.7848714152891,
21.2682405179702,21.7516096206514,22.2349787233325,22.7183478260136,23.2017169286948,
23.6850860313759,24.1684551340571,24.6518242367382,25.1351933394193,25.6185624421005,
26.1019315447816,26.2554830351794),.UNSPECIFIED.);
#795=B_SPLINE_CURVE_WITH_KNOTS('',3,(#44416,#44417,#44418,#44419,#44420,
#44421,#44422,#44423,#44424,#44425,#44426,#44427),.UNSPECIFIED.,.F.,.F.,
(4,1,1,1,1,1,1,1,1,4),(34.5575191894879,34.816620219416,35.2999893220971,
35.7833584247782,36.2667275274594,36.7500966301405,37.2334657328217,37.7168348355028,
38.200203938184,38.5428403214904),.UNSPECIFIED.);
#796=B_SPLINE_CURVE_WITH_KNOTS('',3,(#44430,#44431,#44432,#44433,#44434,
#44435,#44436,#44437,#44438),.UNSPECIFIED.,.F.,.F.,(4,1,1,1,1,1,4),(34.5575191894879,
34.8873368017712,35.3707059044523,35.8540750071334,36.3374441098146,36.8208132124957,
37.3041823151769),.UNSPECIFIED.);
#797=B_SPLINE_CURVE_WITH_KNOTS('',3,(#44443,#44444,#44445,#44446,#44447,
#44448,#44449,#44450,#44451,#44452,#44453,#44454,#44455,#44456,#44457,#44458,
#44459),.UNSPECIFIED.,.F.,.F.,(4,1,1,1,1,1,1,1,1,1,1,1,1,1,4),(28.2743338823079,
28.5328218845611,29.0161909872422,29.4995600899234,29.9829291926045,30.4662982952857,
30.9496673979668,31.4330365006479,31.9164056033291,32.3997747060102,32.8831438086914,
33.3665129113725,33.8498820140537,34.3332511167348,34.5575191894879),
 .UNSPECIFIED.);
#798=B_SPLINE_CURVE_WITH_KNOTS('',3,(#44460,#44461,#44462,#44463,#44464,
#44465,#44466,#44467,#44468,#44469,#44470,#44471,#44472,#44473,#44474,#44475,
#44476),.UNSPECIFIED.,.F.,.F.,(4,1,1,1,1,1,1,1,1,1,1,1,1,1,4),(28.2743338823079,
28.6035384669163,29.0869075695975,29.5702766722786,30.0536457749597,30.5370148776409,
31.020383980322,31.5037530830032,31.9871221856843,32.4704912883655,32.9538603910466,
33.4372294937277,33.9205985964089,34.40396769909,34.5575191894879),
 .UNSPECIFIED.);
#799=B_SPLINE_CURVE_WITH_KNOTS('',3,(#44481,#44482,#44483,#44484,#44485,
#44486,#44487,#44488,#44489,#44490,#44491,#44492,#44493,#44494,#44495,#44496,
#44497),.UNSPECIFIED.,.F.,.F.,(4,1,1,1,1,1,1,1,1,1,1,1,1,1,4),(21.9911485751285,
22.2490235497062,22.7323926523873,23.2157617550685,23.6991308577496,24.1824999604308,
24.6658690631119,25.1492381657931,25.6326072684742,26.1159763711553,26.5993454738365,
27.0827145765176,27.5660836791988,28.0494527818799,28.2743338823079),
 .UNSPECIFIED.);
#800=B_SPLINE_CURVE_WITH_KNOTS('',3,(#44498,#44499,#44500,#44501,#44502,
#44503,#44504,#44505,#44506,#44507,#44508,#44509,#44510,#44511,#44512,#44513,
#44514),.UNSPECIFIED.,.F.,.F.,(4,1,1,1,1,1,1,1,1,1,1,1,1,1,4),(21.9911485751284,
22.3197401320615,22.8031092347426,23.2864783374238,23.7698474401049,24.253216542786,
24.7365856454672,25.2199547481483,25.7033238508295,26.1866929535106,26.6700620561917,
27.1534311588729,27.636800261554,28.1201693642352,28.2743338823079),
 .UNSPECIFIED.);
#801=B_SPLINE_CURVE_WITH_KNOTS('',3,(#44519,#44520,#44521,#44522,#44523,
#44524,#44525,#44526,#44527,#44528,#44529,#44530,#44531,#44532,#44533,#44534,
#44535),.UNSPECIFIED.,.F.,.F.,(4,1,1,1,1,1,1,1,1,1,1,1,1,1,4),(15.707963267949,
15.9652252148513,16.4485943175325,16.9319634202136,17.4153325228947,17.8987016255759,
18.382070728257,18.8654398309382,19.3488089336193,19.8321780363005,20.3155471389816,
20.7989162416628,21.2822853443439,21.765654447025,21.9911485751285),
 .UNSPECIFIED.);
#802=B_SPLINE_CURVE_WITH_KNOTS('',3,(#44536,#44537,#44538,#44539,#44540,
#44541,#44542,#44543,#44544,#44545,#44546,#44547,#44548,#44549,#44550,#44551,
#44552),.UNSPECIFIED.,.F.,.F.,(4,1,1,1,1,1,1,1,1,1,1,1,1,1,4),(15.707963267949,
16.0359417972066,16.5193108998878,17.0026800025689,17.4860491052501,17.9694182079312,
18.4527873106123,18.9361564132935,19.4195255159746,19.9028946186558,20.3862637213369,
20.8696328240181,21.3530019266992,21.8363710293803,21.9911485751284),
 .UNSPECIFIED.);
#803=B_SPLINE_CURVE_WITH_KNOTS('',3,(#45386,#45387,#45388,#45389,#45390,
#45391,#45392,#45393,#45394,#45395,#45396,#45397,#45398,#45399,#45400,#45401,
#45402,#45403,#45404,#45405,#45406,#45407,#45408,#45409,#45410,#45411,#45412,
#45413,#45414,#45415,#45416,#45417,#45418,#45419,#45420,#45421,#45422,#45423,
#45424,#45425,#45426,#45427,#45428,#45429,#45430,#45431,#45432,#45433,#45434,
#45435,#45436,#45437,#45438,#45439,#45440,#45441,#45442,#45443,#45444,#45445,
#45446,#45447,#45448,#45449,#45450,#45451,#45452,#45453,#45454,#45455,#45456,
#45457,#45458,#45459,#45460,#45461,#45462,#45463,#45464,#45465,#45466,#45467,
#45468,#45469,#45470,#45471,#45472,#45473,#45474,#45475,#45476),
 .UNSPECIFIED.,.F.,.F.,(4,3,3,3,3,3,3,3,3,3,3,3,3,3,3,3,3,3,3,3,3,3,3,3,
3,3,3,3,3,3,4),(-2.88655140298914,-2.7102193708046,-2.67807220368065,-2.55828267008941,
-2.50176083674511,-2.46325112464318,-2.28839166473607,-2.20291800933891,
-2.13297054348664,-2.09735834895935,-1.9763367136572,-1.80417085977603,
-1.67697657920847,-1.61936340605544,-1.58062902684361,-1.54800677498682,
-1.37969242088531,-1.29539373750579,-1.1306741467308,-1.06564221343476,
-1.03346927595282,-1.00237020411154,-0.837024911419402,-0.673735787434826,
-0.63651537440582,-0.556950952605093,-0.517031410677791,-0.487820375823624,
-0.32585266849659,-0.162926334248295,0.),.UNSPECIFIED.);
#804=B_SPLINE_CURVE_WITH_KNOTS('',3,(#45477,#45478,#45479,#45480,#45481,
#45482,#45483),.UNSPECIFIED.,.F.,.F.,(4,3,4),(26.2554830351794,26.5853006474628,
26.9279370307691),.UNSPECIFIED.);
#805=B_SPLINE_CURVE_WITH_KNOTS('',3,(#45485,#45486,#45487,#45488,#45489,
#45490,#45491,#45492,#45493,#45494,#45495,#45496,#45497,#45498,#45499,#45500,
#45501,#45502,#45503,#45504,#45505,#45506,#45507,#45508,#45509,#45510,#45511,
#45512,#45513,#45514,#45515,#45516,#45517,#45518,#45519,#45520,#45521,#45522,
#45523,#45524,#45525,#45526,#45527,#45528,#45529,#45530,#45531,#45532,#45533,
#45534,#45535,#45536,#45537,#45538,#45539,#45540,#45541,#45542,#45543,#45544,
#45545,#45546,#45547,#45548,#45549,#45550,#45551,#45552,#45553,#45554,#45555,
#45556,#45557,#45558,#45559,#45560,#45561,#45562,#45563,#45564,#45565,#45566,
#45567,#45568,#45569,#45570,#45571,#45572,#45573,#45574,#45575),
 .UNSPECIFIED.,.F.,.F.,(4,3,3,3,3,3,3,3,3,3,3,3,3,3,3,3,3,3,3,3,3,3,3,3,
3,3,3,3,3,3,4),(-2.89533449801215,-2.73352650875014,-2.71205820706862,-2.59373915178661,
-2.55473003463996,-2.51830819618893,-2.35467992623886,-2.26957883251844,
-2.22055522388971,-2.18083698788503,-2.06810318921435,-1.90126059971141,
-1.77612865758421,-1.71255672102284,-1.67447106332452,-1.64582559314776,
-1.47561435227979,-1.4007328312026,-1.22836140698568,-1.15826779788408,
-1.12728054073534,-0.955264412683464,-0.781353242222385,-0.711247134334915,
-0.62234124254305,-0.578011318404134,-0.547059489792038,-0.371624702645109,
-0.185812351322555,-0.0101929273281714,0.),.UNSPECIFIED.);
#806=B_SPLINE_CURVE_WITH_KNOTS('',3,(#45576,#45577,#45578,#45579,#45580,
#45581,#45582,#45583,#45584,#45585,#45586,#45587,#45588,#45589,#45590),
 .UNSPECIFIED.,.F.,.F.,(4,1,1,1,1,1,1,1,1,1,1,1,4),(10.3762452844077,10.7188816677141,
11.2022507703952,11.6856198730764,12.1689889757575,12.6523580784387,13.1357271811198,
13.6190962838009,14.1024653864821,14.5858344891632,15.0692035918444,15.5525726945255,
15.707963267949),.UNSPECIFIED.);
#807=B_SPLINE_CURVE_WITH_KNOTS('',3,(#45594,#45595,#45596,#45597,#45598,
#45599,#45600,#45601,#45602,#45603,#45604,#45605),.UNSPECIFIED.,.F.,.F.,
(4,1,1,1,1,1,1,1,1,4),(11.614903290721,12.0982723934021,12.5816414960833,
13.0650105987644,13.5483797014456,14.0317488041267,14.5151179068079,14.998487009489,
15.4818561121702,15.707963267949),.UNSPECIFIED.);
#808=B_SPLINE_CURVE_WITH_KNOTS('',3,(#45858,#45859,#45860,#45861,#45862,
#45863,#45864,#45865,#45866,#45867,#45868,#45869,#45870,#45871,#45872,#45873,
#45874,#45875,#45876,#45877,#45878,#45879,#45880,#45881,#45882,#45883,#45884,
#45885,#45886,#45887,#45888,#45889,#45890,#45891,#45892,#45893,#45894,#45895,
#45896,#45897,#45898,#45899,#45900,#45901,#45902,#45903,#45904,#45905,#45906,
#45907,#45908,#45909,#45910,#45911,#45912,#45913,#45914,#45915,#45916,#45917,
#45918,#45919,#45920,#45921,#45922,#45923,#45924,#45925,#45926,#45927,#45928,
#45929,#45930,#45931,#45932,#45933,#45934,#45935,#45936,#45937,#45938,#45939,
#45940,#45941,#45942,#45943,#45944,#45945,#45946,#45947,#45948),
 .UNSPECIFIED.,.F.,.F.,(4,3,3,3,3,3,3,3,3,3,3,3,3,3,3,3,3,3,3,3,3,3,3,3,
3,3,3,3,3,3,4),(-2.89533449801219,-2.73352650875626,-2.71205820706864,-2.59373915175461,
-2.55473003455109,-2.51830819619465,-2.35467992625535,-2.26957883246004,
-2.22055522381054,-2.1808369878803,-2.06810318921433,-1.90126059971139,
-1.77612865758419,-1.71255672104602,-1.67447106339855,-1.64582559316971,
-1.47561435224765,-1.40073283120257,-1.22836140698566,-1.15826779788333,
-1.12728054084049,-0.955264412620505,-0.781353242677817,-0.711247134334909,
-0.622341242543046,-0.578011318009217,-0.547059488903834,-0.371624703144557,
-0.185812351572279,-0.0101929249643171,0.),.UNSPECIFIED.);
#809=B_SPLINE_CURVE_WITH_KNOTS('',3,(#45949,#45950,#45951,#45952,#45953,
#45954,#45955,#45956,#45957,#45958,#45959,#45960,#45961,#45962,#45963,#45964,
#45965,#45966,#45967,#45968,#45969,#45970,#45971,#45972,#45973,#45974,#45975,
#45976,#45977,#45978,#45979,#45980,#45981,#45982,#45983,#45984,#45985,#45986,
#45987,#45988,#45989,#45990,#45991,#45992,#45993,#45994,#45995,#45996,#45997,
#45998,#45999,#46000,#46001,#46002,#46003,#46004,#46005,#46006,#46007,#46008,
#46009,#46010,#46011,#46012,#46013,#46014,#46015,#46016,#46017,#46018,#46019,
#46020,#46021,#46022,#46023,#46024,#46025,#46026,#46027,#46028,#46029,#46030,
#46031,#46032,#46033,#46034,#46035,#46036,#46037,#46038,#46039),
 .UNSPECIFIED.,.F.,.F.,(4,3,3,3,3,3,3,3,3,3,3,3,3,3,3,3,3,3,3,3,3,3,3,3,
3,3,3,3,3,3,4),(-2.8865514029894,-2.7102193707971,-2.67807220368071,-2.55828267024697,
-2.50176083711203,-2.46325112472949,-2.28839166475814,-2.20291800935664,
-2.13297054351986,-2.09735834899737,-1.97633671365723,-1.8041708597012,
-1.67697657915235,-1.61936340596183,-1.58062902659333,-1.54800677505344,
-1.37969242083436,-1.2953937375058,-1.13067414673081,-1.06564221343148,
-1.03346927589314,-1.00237020410157,-0.837024911918307,-0.67373578950061,
-0.636515374405833,-0.556950952605104,-0.517031410437666,-0.48782037559651,
-0.325852668022188,-0.162926334011094,0.),.UNSPECIFIED.);
#810=B_SPLINE_CURVE_WITH_KNOTS('',3,(#46072,#46073,#46074,#46075,#46076,
#46077,#46078,#46079,#46080,#46081),.UNSPECIFIED.,.F.,.F.,(4,3,3,4),(-4.09274904019441,
-3.97454678650995,-2.98091008988247,-2.06120159751572),.UNSPECIFIED.);
#811=B_SPLINE_CURVE_WITH_KNOTS('',3,(#46084,#46085,#46086,#46087,#46088,
#46089,#46090,#46091,#46092,#46093),.UNSPECIFIED.,.F.,.F.,(4,3,3,4),(0.,
0.496818348313743,0.993636696627499,1.11004521091142),.UNSPECIFIED.);
#812=B_SPLINE_CURVE_WITH_KNOTS('',3,(#46098,#46099,#46100,#46101,#46102,
#46103,#46104,#46105,#46106,#46107,#46108,#46109,#46110,#46111,#46112,#46113,
#46114,#46115,#46116,#46117,#46118,#46119),.UNSPECIFIED.,.F.,.F.,(4,3,3,
3,3,3,3,4),(-10.375934347374,-9.93636696627486,-8.94273026964737,-7.94909357301989,
-6.9554568763924,-5.96182017976492,-4.96818348313743,-4.09274904019441),
 .UNSPECIFIED.);
#813=B_SPLINE_CURVE_WITH_KNOTS('',3,(#46120,#46121,#46122,#46123,#46124,
#46125,#46126,#46127,#46128,#46129,#46130,#46131,#46132,#46133,#46134,#46135,
#46136,#46137,#46138,#46139,#46140,#46141),.UNSPECIFIED.,.F.,.F.,(4,3,3,
3,3,3,3,4),(1.11004521091142,1.98727339325499,2.98091008988248,3.97454678650997,
4.96818348313745,5.96182017976494,6.95545687639243,7.393230518091),
 .UNSPECIFIED.);
#814=B_SPLINE_CURVE_WITH_KNOTS('',3,(#46146,#46147,#46148,#46149,#46150,
#46151,#46152,#46153,#46154,#46155,#46156,#46157,#46158,#46159,#46160,#46161,
#46162,#46163,#46164,#46165,#46166,#46167),.UNSPECIFIED.,.F.,.F.,(4,3,3,
3,3,3,3,4),(-16.6591196545536,-15.8981871460398,-14.9045504494123,-13.9109137527848,
-12.9172770561573,-11.9236403595298,-10.9300036629023,-10.375934347374),
 .UNSPECIFIED.);
#815=B_SPLINE_CURVE_WITH_KNOTS('',3,(#46168,#46169,#46170,#46171,#46172,
#46173,#46174,#46175,#46176,#46177,#46178,#46179,#46180,#46181,#46182,#46183,
#46184,#46185,#46186,#46187,#46188,#46189),.UNSPECIFIED.,.F.,.F.,(4,3,3,
3,3,3,3,4),(7.393230518091,7.94909357301991,8.94273026964739,9.93636696627487,
10.9300036629024,11.9236403595298,12.9172770561573,13.6764158252706),
 .UNSPECIFIED.);
#816=B_SPLINE_CURVE_WITH_KNOTS('',3,(#46194,#46195,#46196,#46197,#46198,
#46199,#46200,#46201,#46202,#46203,#46204,#46205,#46206,#46207,#46208,#46209,
#46210,#46211,#46212,#46213,#46214,#46215,#46216,#46217,#46218),
 .UNSPECIFIED.,.F.,.F.,(4,3,3,3,3,3,3,3,4),(-22.9423049617332,-22.8536440224322,
-21.8600073258047,-20.8663706291772,-19.8727339325497,-18.8790972359222,
-17.8854605392947,-16.8918238426673,-16.6591196545536),.UNSPECIFIED.);
#817=B_SPLINE_CURVE_WITH_KNOTS('',3,(#46219,#46220,#46221,#46222,#46223,
#46224,#46225,#46226,#46227,#46228,#46229,#46230,#46231,#46232,#46233,#46234,
#46235,#46236,#46237,#46238,#46239,#46240,#46241,#46242,#46243),
 .UNSPECIFIED.,.F.,.F.,(4,3,3,3,3,3,3,3,4),(13.6764158252706,13.9109137527848,
14.9045504494123,15.8981871460398,16.8918238426673,17.8854605392947,18.8790972359222,
19.8727339325497,19.9596011324502),.UNSPECIFIED.);
#818=B_SPLINE_CURVE_WITH_KNOTS('',3,(#46248,#46249,#46250,#46251,#46252,
#46253,#46254,#46255,#46256,#46257,#46258,#46259,#46260,#46261,#46262,#46263,
#46264,#46265,#46266,#46267,#46268,#46269),.UNSPECIFIED.,.F.,.F.,(4,3,3,
3,3,3,3,4),(-29.2254902689127,-28.8154642021971,-27.8218275055696,-26.8281908089421,
-25.8345541123146,-24.8409174156871,-23.8472807190597,-22.9423049617332),
 .UNSPECIFIED.);
#819=B_SPLINE_CURVE_WITH_KNOTS('',3,(#46270,#46271,#46272,#46273,#46274,
#46275,#46276,#46277,#46278,#46279,#46280,#46281,#46282,#46283,#46284,#46285,
#46286,#46287,#46288,#46289,#46290,#46291),.UNSPECIFIED.,.F.,.F.,(4,3,3,
3,3,3,3,4),(19.9596011324502,20.8663706291772,21.8600073258047,22.8536440224322,
23.8472807190597,24.8409174156871,25.8345541123146,26.2427864396298),
 .UNSPECIFIED.);
#820=B_SPLINE_CURVE_WITH_KNOTS('',3,(#46296,#46297,#46298,#46299,#46300,
#46301,#46302,#46303,#46304,#46305,#46306,#46307,#46308,#46309,#46310,#46311,
#46312,#46313,#46314,#46315,#46316,#46317),.UNSPECIFIED.,.F.,.F.,(4,3,3,
3,3,3,3,4),(-35.5086755760923,-34.777284381962,-33.7836476853345,-32.790010988707,
-31.7963742920795,-30.802737595452,-29.8091008988246,-29.2254902689127),
 .UNSPECIFIED.);
#821=B_SPLINE_CURVE_WITH_KNOTS('',3,(#46318,#46319,#46320,#46321,#46322,
#46323,#46324,#46325,#46326,#46327,#46328,#46329,#46330,#46331,#46332,#46333,
#46334,#46335,#46336,#46337,#46338,#46339),.UNSPECIFIED.,.F.,.F.,(4,3,3,
3,3,3,3,4),(26.2427864396298,26.8281908089421,27.8218275055696,28.8154642021971,
29.8091008988246,30.8027375954521,31.7963742920795,32.5259717468093),
 .UNSPECIFIED.);
#822=B_SPLINE_CURVE_WITH_KNOTS('',3,(#46344,#46345,#46346,#46347,#46348,
#46349,#46350,#46351,#46352,#46353,#46354,#46355,#46356,#46357,#46358,#46359,
#46360,#46361,#46362,#46363,#46364,#46365,#46366,#46367,#46368),
 .UNSPECIFIED.,.F.,.F.,(4,3,3,3,3,3,3,3,4),(-41.7918608832719,-41.7327412583544,
-40.7391045617269,-39.7454678650994,-38.7518311684719,-37.7581944718444,
-36.764557775217,-35.7709210785895,-35.5086755760923),.UNSPECIFIED.);
#823=B_SPLINE_CURVE_WITH_KNOTS('',3,(#46369,#46370,#46371,#46372,#46373,
#46374,#46375,#46376,#46377,#46378,#46379,#46380,#46381,#46382,#46383,#46384,
#46385,#46386,#46387,#46388,#46389,#46390,#46391,#46392,#46393),
 .UNSPECIFIED.,.F.,.F.,(4,3,3,3,3,3,3,3,4),(32.5259717468093,32.790010988707,
33.7836476853345,34.777284381962,35.7709210785895,36.764557775217,37.7581944718445,
38.751831168472,38.8091570539889),.UNSPECIFIED.);
#824=B_SPLINE_CURVE_WITH_KNOTS('',3,(#46398,#46399,#46400,#46401,#46402,
#46403,#46404,#46405,#46406,#46407,#46408,#46409,#46410,#46411,#46412,#46413,
#46414,#46415,#46416,#46417,#46418,#46419),.UNSPECIFIED.,.F.,.F.,(4,3,3,
3,3,3,3,4),(-48.0750461904515,-47.6945614381193,-46.7009247414918,-45.7072880448643,
-44.7136513482368,-43.7200146516094,-42.7263779549819,-41.7918608832719),
 .UNSPECIFIED.);
#825=B_SPLINE_CURVE_WITH_KNOTS('',3,(#46420,#46421,#46422,#46423,#46424,
#46425,#46426,#46427,#46428,#46429,#46430,#46431,#46432,#46433,#46434,#46435,
#46436,#46437,#46438,#46439,#46440,#46441),.UNSPECIFIED.,.F.,.F.,(4,3,3,
3,3,3,3,4),(38.8091570539889,39.7454678650994,40.7391045617269,41.7327412583544,
42.7263779549819,43.7200146516094,44.7136513482369,45.0923423611685),
 .UNSPECIFIED.);
#826=B_SPLINE_CURVE_WITH_KNOTS('',3,(#46446,#46447,#46448,#46449,#46450,
#46451,#46452,#46453,#46454,#46455,#46456,#46457,#46458,#46459,#46460,#46461,
#46462,#46463,#46464,#46465,#46466,#46467),.UNSPECIFIED.,.F.,.F.,(4,3,3,
3,3,3,3,4),(-54.3582314976311,-53.6563816178842,-52.6627449212567,-51.6691082246292,
-50.6754715280018,-49.6818348313743,-48.6881981347468,-48.0750461904515),
 .UNSPECIFIED.);
#827=B_SPLINE_CURVE_WITH_KNOTS('',3,(#46468,#46469,#46470,#46471,#46472,
#46473,#46474,#46475,#46476,#46477,#46478,#46479,#46480,#46481,#46482,#46483,
#46484,#46485,#46486,#46487,#46488,#46489),.UNSPECIFIED.,.F.,.F.,(4,3,3,
3,3,3,3,4),(45.0923423611685,45.7072880448643,46.7009247414918,47.6945614381193,
48.6881981347468,49.6818348313743,50.6754715280018,51.3755276683481),
 .UNSPECIFIED.);
#828=B_SPLINE_CURVE_WITH_KNOTS('',3,(#46494,#46495,#46496,#46497,#46498,
#46499,#46500,#46501,#46502,#46503,#46504,#46505,#46506,#46507,#46508,#46509,
#46510,#46511,#46512,#46513,#46514,#46515,#46516,#46517,#46518),
 .UNSPECIFIED.,.F.,.F.,(4,3,3,3,3,3,3,3,4),(-60.6414168048107,-60.6118384942766,
-59.6182017976491,-58.6245651010216,-57.6309284043942,-56.6372917077667,
-55.6436550111392,-54.6500183145117,-54.3582314976311),.UNSPECIFIED.);
#829=B_SPLINE_CURVE_WITH_KNOTS('',3,(#46519,#46520,#46521,#46522,#46523,
#46524,#46525,#46526,#46527,#46528,#46529,#46530,#46531,#46532,#46533,#46534,
#46535,#46536,#46537,#46538,#46539,#46540,#46541,#46542,#46543),
 .UNSPECIFIED.,.F.,.F.,(4,3,3,3,3,3,3,3,4),(51.3755276683481,51.6691082246293,
52.6627449212567,53.6563816178842,54.6500183145117,55.6436550111392,56.6372917077667,
57.6309284043942,57.6587129755277),.UNSPECIFIED.);
#830=B_SPLINE_CURVE_WITH_KNOTS('',3,(#46548,#46549,#46550,#46551,#46552,
#46553,#46554,#46555,#46556,#46557,#46558,#46559,#46560,#46561,#46562,#46563,
#46564,#46565,#46566,#46567,#46568,#46569),.UNSPECIFIED.,.F.,.F.,(4,3,3,
3,3,3,3,4),(-66.9246021119903,-66.5736586740415,-65.580021977414,-64.5863852807866,
-63.5927485841591,-62.5991118875316,-61.6054751909041,-60.6414168048107),
 .UNSPECIFIED.);
#831=B_SPLINE_CURVE_WITH_KNOTS('',3,(#46570,#46571,#46572,#46573,#46574,
#46575,#46576,#46577,#46578,#46579,#46580,#46581,#46582,#46583,#46584,#46585,
#46586,#46587,#46588,#46589,#46590,#46591),.UNSPECIFIED.,.F.,.F.,(4,3,3,
3,3,3,3,4),(57.6587129755277,58.6245651010217,59.6182017976491,60.6118384942766,
61.6054751909041,62.5991118875316,63.5927485841591,63.9418982827073),
 .UNSPECIFIED.);
#832=B_SPLINE_CURVE_WITH_KNOTS('',3,(#46596,#46597,#46598,#46599,#46600,
#46601,#46602,#46603,#46604,#46605,#46606,#46607,#46608,#46609,#46610,#46611,
#46612,#46613,#46614,#46615,#46616,#46617),.UNSPECIFIED.,.F.,.F.,(4,3,3,
3,3,3,3,4),(-73.2077874191699,-72.5354788538064,-71.541842157179,-70.5482054605515,
-69.554568763924,-68.5609320672965,-67.567295370669,-66.9246021119903),
 .UNSPECIFIED.);
#833=B_SPLINE_CURVE_WITH_KNOTS('',3,(#46618,#46619,#46620,#46621,#46622,
#46623,#46624,#46625,#46626,#46627,#46628,#46629,#46630,#46631,#46632,#46633,
#46634,#46635,#46636,#46637,#46638,#46639),.UNSPECIFIED.,.F.,.F.,(4,3,3,
3,3,3,3,4),(63.9418982827073,64.5863852807866,65.580021977414,66.5736586740415,
67.567295370669,68.5609320672965,69.554568763924,70.2250835898869),
 .UNSPECIFIED.);
#834=B_SPLINE_CURVE_WITH_KNOTS('',3,(#46644,#46645,#46646,#46647,#46648,
#46649,#46650,#46651,#46652,#46653,#46654,#46655,#46656,#46657,#46658,#46659,
#46660,#46661,#46662,#46663,#46664,#46665),.UNSPECIFIED.,.F.,.F.,(4,3,3,
3,3,3,3,4),(-79.4909727263495,-78.4972990335714,-77.5036623369439,-76.5100256403164,
-75.5163889436889,-74.5227522470614,-73.5291155504339,-73.2077874191699),
 .UNSPECIFIED.);
#835=B_SPLINE_CURVE_WITH_KNOTS('',3,(#46666,#46667,#46668,#46669,#46670,
#46671,#46672,#46673,#46674,#46675,#46676,#46677,#46678,#46679,#46680,#46681,
#46682,#46683,#46684,#46685,#46686,#46687),.UNSPECIFIED.,.F.,.F.,(4,3,3,
3,3,3,3,4),(70.2250835898869,70.5482054605515,71.5418421571789,72.5354788538064,
73.5291155504339,74.5227522470614,75.5163889436889,76.5082688970665),
 .UNSPECIFIED.);
#836=B_SPLINE_CURVE_WITH_KNOTS('',3,(#46692,#46693,#46694,#46695,#46696,
#46697,#46698,#46699,#46700,#46701,#46702,#46703,#46704,#46705,#46706,#46707,
#46708,#46709,#46710,#46711,#46712,#46713),.UNSPECIFIED.,.F.,.F.,(4,3,3,
3,3,3,3,4),(-85.7741580335291,-85.4527559099638,-84.4591192133363,-83.4654825167088,
-82.4718458200813,-81.4782091234538,-80.4845724268263,-79.4909727263495),
 .UNSPECIFIED.);
#837=B_SPLINE_CURVE_WITH_KNOTS('',3,(#46714,#46715,#46716,#46717,#46718,
#46719,#46720,#46721,#46722,#46723,#46724,#46725,#46726,#46727,#46728,#46729,
#46730,#46731,#46732,#46733,#46734,#46735),.UNSPECIFIED.,.F.,.F.,(4,3,3,
3,3,3,3,4),(76.5082688970665,77.5036623369438,78.4972990335713,79.4909357301988,
80.4845724268263,81.4782091234538,82.4718458200813,82.7914542042461),
 .UNSPECIFIED.);
#838=B_SPLINE_CURVE_WITH_KNOTS('',3,(#46740,#46741,#46742,#46743,#46744,
#46745,#46746,#46747,#46748,#46749,#46750,#46751,#46752,#46753,#46754,#46755,
#46756,#46757,#46758,#46759,#46760,#46761),.UNSPECIFIED.,.F.,.F.,(4,3,3,
3,3,3,3,4),(-92.0573433407087,-91.4145760897287,-90.4209393931012,-89.4273026964737,
-88.4336659998462,-87.4400293032187,-86.4463926065912,-85.7741580335291),
 .UNSPECIFIED.);
#839=B_SPLINE_CURVE_WITH_KNOTS('',3,(#46762,#46763,#46764,#46765,#46766,
#46767,#46768,#46769,#46770,#46771,#46772,#46773,#46774,#46775,#46776,#46777,
#46778,#46779,#46780,#46781,#46782,#46783),.UNSPECIFIED.,.F.,.F.,(4,3,3,
3,3,3,3,4),(82.7914542042461,83.4654825167088,84.4591192133363,85.4527559099638,
86.4463926065912,87.4400293032187,88.4336659998462,89.0746395114257),
 .UNSPECIFIED.);
#840=B_SPLINE_CURVE_WITH_KNOTS('',3,(#46789,#46790,#46791,#46792,#46793),
 .UNSPECIFIED.,.F.,.F.,(4,1,4),(103.672557568463,104.023427014111,104.943135506477),
 .UNSPECIFIED.);
#841=B_SPLINE_CURVE_WITH_KNOTS('',3,(#46796,#46797,#46798,#46799),
 .UNSPECIFIED.,.F.,.F.,(4,4),(103.672557568463,103.703855626096),
 .UNSPECIFIED.);
#842=B_SPLINE_CURVE_WITH_KNOTS('',3,(#46804,#46805,#46806,#46807,#46808,
#46809,#46810,#46811,#46812,#46813),.UNSPECIFIED.,.F.,.F.,(4,1,1,1,1,1,
1,4),(97.3893722612836,98.0616068343457,99.0552435309732,100.048880227601,
101.042516924228,102.036153620856,103.029790317483,103.672557568463),
 .UNSPECIFIED.);
#843=B_SPLINE_CURVE_WITH_KNOTS('',3,(#46814,#46815,#46816,#46817,#46818,
#46819,#46820,#46821,#46822,#46823,#46824),.UNSPECIFIED.,.F.,.F.,(4,1,1,
1,1,1,1,1,4),(97.3893722612836,97.7420354463315,98.735672142959,99.7293088395865,
100.722945536214,101.716582232841,102.710218929469,103.207037277783,103.672557568463),
 .UNSPECIFIED.);
#844=B_SPLINE_CURVE_WITH_KNOTS('',3,(#46829,#46830,#46831,#46832,#46833,
#46834,#46835,#46836,#46837,#46838),.UNSPECIFIED.,.F.,.F.,(4,1,1,1,1,1,
1,4),(91.106186954104,92.0997866545808,93.0934233512083,94.0870600478358,
95.0806967444633,96.0743334410907,97.0679701377182,97.3893722612836),
 .UNSPECIFIED.);
#845=B_SPLINE_CURVE_WITH_KNOTS('',3,(#46839,#46840,#46841,#46842,#46843,
#46844,#46845,#46846,#46847,#46848),.UNSPECIFIED.,.F.,.F.,(4,1,1,1,1,1,
1,4),(91.106186954104,91.7802152665666,92.7738519631941,93.7674886598216,
94.761125356449,95.7547620530765,96.748398749704,97.3893722612836),
 .UNSPECIFIED.);
#846=B_SPLINE_CURVE_WITH_KNOTS('',3,(#46853,#46854,#46855,#46856,#46857,
#46858,#46859,#46860,#46861,#46862,#46863),.UNSPECIFIED.,.F.,.F.,(4,1,1,
1,1,1,1,1,4),(84.8230016469244,85.1443297781884,86.1379664748159,87.1316031714434,
88.1252398680709,89.1188765646984,90.1125132613258,91.1061499579533,91.106186954104),
 .UNSPECIFIED.);
#847=B_SPLINE_CURVE_WITH_KNOTS('',3,(#46864,#46865,#46866,#46867,#46868,
#46869,#46870,#46871,#46872,#46873,#46874),.UNSPECIFIED.,.F.,.F.,(4,1,1,
1,1,1,1,1,4),(84.8230016469244,84.8247583901742,85.8183950868017,86.8120317834291,
87.8056684800567,88.7993051766841,89.7929418733116,90.7865785699391,91.106186954104),
 .UNSPECIFIED.);
#848=B_SPLINE_CURVE_WITH_KNOTS('',3,(#46879,#46880,#46881,#46882,#46883,
#46884,#46885,#46886,#46887,#46888),.UNSPECIFIED.,.F.,.F.,(4,1,1,1,1,1,
1,4),(78.5398163397448,79.1825095984235,80.176146295051,81.1697829916785,
82.163419688306,83.1570563849334,84.1506930815609,84.8230016469244),
 .UNSPECIFIED.);
#849=B_SPLINE_CURVE_WITH_KNOTS('',3,(#46889,#46890,#46891,#46892,#46893,
#46894,#46895,#46896,#46897,#46898),.UNSPECIFIED.,.F.,.F.,(4,1,1,1,1,1,
1,4),(78.5398163397448,78.8629382104093,79.8565749070368,80.8502116036642,
81.8438483002917,82.8374849969192,83.8311216935467,84.8230016469244),
 .UNSPECIFIED.);
#850=B_SPLINE_CURVE_WITH_KNOTS('',3,(#46903,#46904,#46905,#46906,#46907,
#46908,#46909,#46910,#46911,#46912),.UNSPECIFIED.,.F.,.F.,(4,1,1,1,1,1,
1,4),(72.2566310325652,73.2206894186586,74.2143261152861,75.2079628119136,
76.201599508541,77.1952362051685,78.188872901796,78.5398163397448),
 .UNSPECIFIED.);
#851=B_SPLINE_CURVE_WITH_KNOTS('',3,(#46913,#46914,#46915,#46916,#46917,
#46918,#46919,#46920,#46921,#46922),.UNSPECIFIED.,.F.,.F.,(4,1,1,1,1,1,
1,4),(72.2566310325652,72.9011180306444,73.8947547272718,74.8883914238993,
75.8820281205268,76.8756648171543,77.8693015137818,78.5398163397448),
 .UNSPECIFIED.);
#852=B_SPLINE_CURVE_WITH_KNOTS('',3,(#46927,#46928,#46929,#46930,#46931,
#46932,#46933,#46934,#46935,#46936,#46937),.UNSPECIFIED.,.F.,.F.,(4,1,1,
1,1,1,1,1,4),(65.9734457253856,66.2652325422662,67.2588692388937,68.2525059355212,
69.2461426321486,70.2397793287761,71.2334160254036,72.2270527220311,72.2566310325652),
 .UNSPECIFIED.);
#853=B_SPLINE_CURVE_WITH_KNOTS('',3,(#46938,#46939,#46940,#46941,#46942,
#46943,#46944,#46945,#46946,#46947),.UNSPECIFIED.,.F.,.F.,(4,1,1,1,1,1,
1,4),(65.9734457253856,66.9392978508795,67.9329345475069,68.9265712441344,
69.9202079407619,70.9138446373894,71.9074813340169,72.2566310325652),
 .UNSPECIFIED.);
#854=B_SPLINE_CURVE_WITH_KNOTS('',3,(#46952,#46953,#46954,#46955,#46956,
#46957,#46958,#46959,#46960,#46961),.UNSPECIFIED.,.F.,.F.,(4,1,1,1,1,1,
1,4),(59.690260418206,60.3034123625013,61.2970490591288,62.2906857557562,
63.2843224523837,64.2779591490112,65.2715958456387,65.9734457253856),
 .UNSPECIFIED.);
#855=B_SPLINE_CURVE_WITH_KNOTS('',3,(#46962,#46963,#46964,#46965,#46966,
#46967,#46968,#46969,#46970,#46971,#46972),.UNSPECIFIED.,.F.,.F.,(4,1,1,
1,1,1,1,1,4),(59.690260418206,59.9838409744871,60.9774776711145,61.971114367742,
62.9647510643695,63.958387760997,64.9520244576245,65.945661154252,65.9734457253856),
 .UNSPECIFIED.);
#856=B_SPLINE_CURVE_WITH_KNOTS('',3,(#46977,#46978,#46979,#46980,#46981,
#46982,#46983,#46984,#46985,#46986),.UNSPECIFIED.,.F.,.F.,(4,1,1,1,1,1,
1,4),(53.4070751110265,54.3415921827364,55.3352288793638,56.3288655759913,
57.3225022726188,58.3161389692463,59.3097756658738,59.690260418206),
 .UNSPECIFIED.);
#857=B_SPLINE_CURVE_WITH_KNOTS('',3,(#46987,#46988,#46989,#46990,#46991,
#46992,#46993,#46994,#46995,#46996),.UNSPECIFIED.,.F.,.F.,(4,1,1,1,1,1,
1,4),(53.4070751110264,54.0220207947221,55.0156574913496,56.0092941879771,
57.0029308846046,57.9965675812321,58.9902042778596,59.690260418206),
 .UNSPECIFIED.);
#858=B_SPLINE_CURVE_WITH_KNOTS('',3,(#47001,#47002,#47003,#47004,#47005,
#47006,#47007,#47008,#47009,#47010,#47011),.UNSPECIFIED.,.F.,.F.,(4,1,1,
1,1,1,1,1,4),(47.1238898038469,47.386135306344,48.3797720029714,49.3734086995989,
50.3670453962264,51.3606820928539,52.3543187894814,53.3479554861089,53.4070751110265),
 .UNSPECIFIED.);
#859=B_SPLINE_CURVE_WITH_KNOTS('',3,(#47012,#47013,#47014,#47015,#47016,
#47017,#47018,#47019,#47020,#47021),.UNSPECIFIED.,.F.,.F.,(4,1,1,1,1,1,
1,4),(47.1238898038469,48.0602006149572,49.0538373115847,50.0474740082122,
51.0411107048397,52.0347474014672,53.0283840980947,53.4070751110264),
 .UNSPECIFIED.);
#860=B_SPLINE_CURVE_WITH_KNOTS('',3,(#47026,#47027,#47028,#47029,#47030,
#47031,#47032,#47033,#47034,#47035),.UNSPECIFIED.,.F.,.F.,(4,1,1,1,1,1,
1,4),(40.8407044966672,41.4243151265791,42.4179518232065,43.411588519834,
44.4052252164615,45.398861913089,46.3924986097165,47.1238898038469),
 .UNSPECIFIED.);
#861=B_SPLINE_CURVE_WITH_KNOTS('',3,(#47036,#47037,#47038,#47039,#47040,
#47041,#47042,#47043,#47044,#47045,#47046),.UNSPECIFIED.,.F.,.F.,(4,1,1,
1,1,1,1,1,4),(40.8407044966673,41.1047437385648,42.0983804351923,43.0920171318198,
44.0856538284473,45.0792905250748,46.0729272217023,47.0665639183297,47.1238898038469),
 .UNSPECIFIED.);
#862=B_SPLINE_CURVE_WITH_KNOTS('',3,(#47051,#47052,#47053,#47054,#47055,
#47056,#47057,#47058,#47059,#47060),.UNSPECIFIED.,.F.,.F.,(4,1,1,1,1,1,
1,4),(34.5575191894877,35.4624949468141,36.4561316434416,37.4497683400691,
38.4434050366966,39.4370417333241,40.4306784299516,40.8407044966672),
 .UNSPECIFIED.);
#863=B_SPLINE_CURVE_WITH_KNOTS('',3,(#47061,#47062,#47063,#47064,#47065,
#47066,#47067,#47068,#47069,#47070),.UNSPECIFIED.,.F.,.F.,(4,1,1,1,1,1,
1,4),(34.5575191894877,35.1429235587999,36.1365602554274,37.1301969520549,
38.1238336486824,39.1174703453099,40.1111070419373,40.8407044966673),
 .UNSPECIFIED.);
#864=B_SPLINE_CURVE_WITH_KNOTS('',3,(#47075,#47076,#47077,#47078,#47079,
#47080,#47081,#47082,#47083,#47084,#47085),.UNSPECIFIED.,.F.,.F.,(4,1,1,
1,1,1,1,1,4),(28.2743338823081,28.5070380704217,29.5006747670492,30.4943114636767,
31.4879481603042,32.4815848569317,33.4752215535592,34.4688582501867,34.5575191894877),
 .UNSPECIFIED.);
#865=B_SPLINE_CURVE_WITH_KNOTS('',3,(#47086,#47087,#47088,#47089,#47090,
#47091,#47092,#47093,#47094,#47095),.UNSPECIFIED.,.F.,.F.,(4,1,1,1,1,1,
1,4),(28.2743338823081,29.181103379035,30.1747400756625,31.16837677229,
32.1620134689175,33.155650165545,34.1492868621724,34.5575191894877),
 .UNSPECIFIED.);
#866=B_SPLINE_CURVE_WITH_KNOTS('',3,(#47100,#47101,#47102,#47103,#47104,
#47105,#47106,#47107,#47108,#47109),.UNSPECIFIED.,.F.,.F.,(4,1,1,1,1,1,
1,4),(21.9911485751285,22.5452178906568,23.5388545872843,24.5324912839118,
25.5261279805393,26.5197646771668,27.5134013737943,28.2743338823081),
 .UNSPECIFIED.);
#867=B_SPLINE_CURVE_WITH_KNOTS('',3,(#47110,#47111,#47112,#47113,#47114,
#47115,#47116,#47117,#47118,#47119,#47120),.UNSPECIFIED.,.F.,.F.,(4,1,1,
1,1,1,1,1,4),(21.9911485751285,22.2256465026426,23.2192831992701,24.2129198958976,
25.2065565925251,26.2001932891526,27.19382998578,28.1874666824075,28.2743338823081),
 .UNSPECIFIED.);
#868=B_SPLINE_CURVE_WITH_KNOTS('',3,(#47125,#47126,#47127,#47128,#47129,
#47130,#47131,#47132,#47133,#47134),.UNSPECIFIED.,.F.,.F.,(4,1,1,1,1,1,
1,4),(15.7079632679489,16.5833977108919,17.5770344075194,18.5706711041469,
19.5643078007744,20.5579444974019,21.5515811940293,21.9911485751285),
 .UNSPECIFIED.);
#869=B_SPLINE_CURVE_WITH_KNOTS('',3,(#47135,#47136,#47137,#47138,#47139,
#47140,#47141,#47142,#47143,#47144),.UNSPECIFIED.,.F.,.F.,(4,1,1,1,1,1,
1,4),(15.7079632679489,16.2638263228777,17.2574630195052,18.2510997161327,
19.2447364127602,20.2383731093876,21.2320098060151,21.9911485751285),
 .UNSPECIFIED.);
#870=B_SPLINE_CURVE_WITH_KNOTS('',3,(#47952,#47953,#47954,#47955,#47956,
#47957,#47958,#47959,#47960,#47961,#47962,#47963,#47964,#47965,#47966,#47967,
#47968,#47969,#47970,#47971,#47972,#47973,#47974,#47975,#47976,#47977,#47978,
#47979,#47980,#47981,#47982,#47983,#47984,#47985,#47986,#47987,#47988,#47989,
#47990,#47991,#47992,#47993,#47994,#47995,#47996,#47997,#47998,#47999,#48000,
#48001,#48002,#48003,#48004,#48005,#48006,#48007,#48008,#48009,#48010,#48011,
#48012,#48013,#48014,#48015),.UNSPECIFIED.,.F.,.F.,(4,3,3,3,3,3,3,3,3,3,
3,3,3,3,3,3,3,3,3,3,3,4),(-0.741270768406293,-0.712255887547373,-0.665684585950267,
-0.644578145540201,-0.627409884287908,-0.56289444703525,-0.543149871110002,
-0.525346816277411,-0.462778575991627,-0.422541646340016,-0.403602109472732,
-0.388134731867962,-0.339685474770525,-0.287921025014436,-0.267367512869476,
-0.250461281201999,-0.191574752108606,-0.165649592692258,-0.130279761088628,
-0.116485368772831,-0.0582426843864153,0.),.UNSPECIFIED.);
#871=B_SPLINE_CURVE_WITH_KNOTS('',3,(#48016,#48017,#48018,#48019,#48020,
#48021,#48022,#48023,#48024,#48025,#48026,#48027,#48028,#48029,#48030,#48031),
 .UNSPECIFIED.,.F.,.F.,(4,3,3,3,3,4),(89.0746395114257,89.4273026964737,
90.4209393931012,91.4145760897287,92.4082127863561,93.3279212787228),
 .UNSPECIFIED.);
#872=B_SPLINE_CURVE_WITH_KNOTS('',3,(#48033,#48034,#48035,#48036,#48037,
#48038,#48039,#48040,#48041,#48042,#48043,#48044,#48045,#48046,#48047,#48048,
#48049,#48050,#48051,#48052,#48053,#48054,#48055,#48056,#48057,#48058,#48059,
#48060,#48061,#48062,#48063,#48064,#48065,#48066,#48067,#48068,#48069,#48070,
#48071,#48072,#48073,#48074,#48075,#48076,#48077,#48078,#48079,#48080,#48081,
#48082,#48083,#48084,#48085,#48086,#48087,#48088,#48089,#48090,#48091,#48092,
#48093,#48094,#48095,#48096),.UNSPECIFIED.,.F.,.F.,(4,3,3,3,3,3,3,3,3,3,
3,3,3,3,3,3,3,3,3,3,3,4),(-0.744397949170265,-0.720232764262911,-0.673202521468055,
-0.646203568187049,-0.596939292083825,-0.573499405051569,-0.555762434684145,
-0.495454099387841,-0.456502934283493,-0.439348901583241,-0.424325906339616,
-0.376932525681518,-0.330843929367177,-0.304626791409719,-0.285107413231915,
-0.222343876864638,-0.192578140424153,-0.156226789527131,-0.140024719995705,
-0.0753705999558412,-0.0106626303314335,0.),.UNSPECIFIED.);
#873=B_SPLINE_CURVE_WITH_KNOTS('',3,(#48097,#48098,#48099,#48100,#48101,
#48102,#48103,#48104,#48105),.UNSPECIFIED.,.F.,.F.,(4,1,1,1,1,1,4),(10.3759343473736,
11.2956428397403,12.2892795363678,13.2829162329952,14.2765529296227,15.2701896262502,
15.7079632679489),.UNSPECIFIED.);
#874=B_SPLINE_CURVE_WITH_KNOTS('',3,(#48111,#48112,#48113,#48114,#48115,
#48116,#48117,#48118,#48119,#48120,#48121,#48122,#48123,#48124,#48125,#48126,
#48127,#48128,#48129,#48130,#48131,#48132,#48133,#48134,#48135,#48136,#48137,
#48138,#48139,#48140,#48141,#48142,#48143,#48144,#48145,#48146,#48147,#48148,
#48149,#48150,#48151,#48152,#48153,#48154,#48155,#48156,#48157,#48158,#48159,
#48160,#48161,#48162,#48163,#48164,#48165,#48166,#48167,#48168,#48169,#48170,
#48171,#48172,#48173,#48174),.UNSPECIFIED.,.F.,.F.,(4,3,3,3,3,3,3,3,3,3,
3,3,3,3,3,3,3,3,3,3,3,4),(-0.741270768406662,-0.712255887547674,-0.665684585950538,
-0.644578143487901,-0.627409881579087,-0.562894446898948,-0.543149865542399,
-0.525346815316762,-0.462778578250359,-0.4225416506717,-0.403602129361835,
-0.388134740123997,-0.339685474770589,-0.287920989652608,-0.267367466812484,
-0.250461299706187,-0.191574764229376,-0.165649592692285,-0.130279760406768,
-0.116485367671245,-0.0582426838356225,0.),.UNSPECIFIED.);
#875=B_SPLINE_CURVE_WITH_KNOTS('',3,(#48177,#48178,#48179,#48180,#48181,
#48182,#48183,#48184,#48185),.UNSPECIFIED.,.F.,.F.,(4,1,1,1,1,1,4),(11.6152142277545,
12.1120325760682,12.608850924382,13.6024876210095,14.5961243176369,15.5897610142644,
15.7079632679489),.UNSPECIFIED.);
#876=B_SPLINE_CURVE_WITH_KNOTS('',3,(#48591,#48592,#48593,#48594,#48595,
#48596,#48597,#48598,#48599,#48600,#48601,#48602,#48603,#48604,#48605,#48606,
#48607,#48608,#48609,#48610,#48611,#48612,#48613,#48614,#48615,#48616,#48617,
#48618,#48619,#48620,#48621,#48622,#48623,#48624,#48625,#48626,#48627,#48628,
#48629,#48630,#48631,#48632,#48633,#48634,#48635,#48636,#48637,#48638,#48639,
#48640,#48641,#48642,#48643,#48644,#48645,#48646,#48647,#48648,#48649,#48650,
#48651,#48652,#48653,#48654),.UNSPECIFIED.,.F.,.F.,(4,3,3,3,3,3,3,3,3,3,
3,3,3,3,3,3,3,3,3,3,3,4),(-0.744397949170718,-0.720232764263358,-0.673202521370767,
-0.646203568277415,-0.596939266463238,-0.573498931627384,-0.555762400888746,
-0.495454066743922,-0.456502918787901,-0.439348839381182,-0.424325811011317,
-0.376932525681586,-0.330843929367237,-0.304626788677627,-0.285107412643743,
-0.222343877199312,-0.19257814042419,-0.156226788834009,-0.140024719746733,
-0.0753705894557632,-0.0106626208978399,0.),.UNSPECIFIED.);
#877=B_SPLINE_CURVE_WITH_KNOTS('',3,(#48655,#48656,#48657,#48658,#48659,
#48660,#48661,#48662,#48663,#48664,#48665,#48666,#48667,#48668,#48669,#48670),
 .UNSPECIFIED.,.F.,.F.,(4,3,3,3,3,4),(-95.3891228762386,-94.8923045279249,
-94.3954861796111,-93.4018494829836,-92.4082127863561,-92.0573433407087),
 .UNSPECIFIED.);
#878=B_SPLINE_CURVE_WITH_KNOTS('',3,(#48749,#48750,#48751,#48752,#48753,
#48754,#48755,#48756,#48757,#48758,#48759,#48760,#48761,#48762,#48763,#48764,
#48765,#48766),.UNSPECIFIED.,.F.,.F.,(4,2,2,2,2,2,2,2,4),(0.214479017187888,
0.226613658149299,0.453227316298599,0.679830564793567,0.906433813288534,
1.1330370617835,1.35964031027847,1.58625396842777,1.59838860938918),
 .UNSPECIFIED.);
#879=B_SPLINE_CURVE_WITH_KNOTS('',3,(#48768,#48769,#48770,#48771,#48772,
#48773,#48774,#48775,#48776,#48777,#48778,#48779,#48780,#48781,#48782,#48783,
#48784,#48785),.UNSPECIFIED.,.F.,.F.,(4,2,2,2,2,2,2,2,4),(2.02734664376496,
2.03948128472637,2.26609494287567,2.49269819137064,2.7193014398656,2.94590468836057,
3.17250793685554,3.39912159500484,3.41125623596625),.UNSPECIFIED.);
#880=B_SPLINE_CURVE_WITH_KNOTS('',3,(#49263,#49264,#49265,#49266,#49267,
#49268,#49269,#49270,#49271,#49272,#49273,#49274,#49275,#49276,#49277,#49278,
#49279),.UNSPECIFIED.,.F.,.F.,(4,2,2,2,2,2,2,1,4),(0.,0.094448813972548,
0.188897627945096,0.283341149511147,0.377784671077197,0.472228192643248,
0.566671714209298,0.661120528181846,0.755569342154394),.UNSPECIFIED.);
#881=B_SPLINE_CURVE_WITH_KNOTS('',3,(#49280,#49281,#49282,#49283,#49284,
#49285,#49286,#49287,#49288,#49289,#49290,#49291,#49292,#49293,#49294,#49295,
#49296),.UNSPECIFIED.,.F.,.F.,(4,1,2,2,2,2,2,2,4),(0.755569342154394,0.850018156126942,
0.94446697009949,1.03891049166554,1.13335401323159,1.22779753479764,1.32224105636369,
1.41668987033624,1.51113868430879),.UNSPECIFIED.);
#882=B_SPLINE_CURVE_WITH_KNOTS('',3,(#49297,#49298,#49299,#49300,#49301,
#49302,#49303,#49304,#49305,#49306,#49307,#49308,#49309,#49310,#49311,#49312,
#49313,#49314,#49315,#49316,#49317,#49318,#49319,#49320,#49321,#49322,#49323,
#49324,#49325,#49326,#49327),.UNSPECIFIED.,.T.,.F.,(4,2,2,2,2,2,2,1,1,1,
2,2,2,2,2,2,4),(-1.51113868430879,-1.41668987033624,-1.32224105636369,-1.22779753479764,
-1.13335401323159,-1.03891049166554,-0.94446697009949,-0.850018156126942,
-0.755569342154394,-0.661120528181846,-0.566671714209298,-0.472228192643248,
-0.377784671077197,-0.283341149511147,-0.188897627945096,-0.094448813972548,
0.),.UNSPECIFIED.);
#883=B_SPLINE_CURVE_WITH_KNOTS('',3,(#49332,#49333,#49334,#49335,#49336,
#49337,#49338,#49339,#49340,#49341,#49342,#49343,#49344,#49345,#49346,#49347),
 .UNSPECIFIED.,.F.,.F.,(4,2,2,1,2,2,2,1,4),(0.,0.094448813972548,0.283341149511147,
0.330562910294172,0.377784671077197,0.472228192643248,0.566671714209298,
0.661120528181846,0.755569342154394),.UNSPECIFIED.);
#884=B_SPLINE_CURVE_WITH_KNOTS('',3,(#49348,#49349,#49350,#49351,#49352,
#49353,#49354,#49355,#49356,#49357,#49358,#49359,#49360,#49361,#49362,#49363,
#49364,#49365),.UNSPECIFIED.,.F.,.F.,(4,1,1,2,2,2,2,2,2,4),(0.755569342154394,
0.779181545647531,0.850018156126942,0.94446697009949,1.03891049166554,1.13335401323159,
1.22779753479764,1.32224105636369,1.41668987033624,1.51113868430879),
 .UNSPECIFIED.);
#885=B_SPLINE_CURVE_WITH_KNOTS('',3,(#49373,#49374,#49375,#49376,#49377,
#49378,#49379,#49380,#49381,#49382,#49383,#49384,#49385,#49386,#49387,#49388,
#49389,#49390,#49391,#49392,#49393,#49394,#49395,#49396,#49397,#49398,#49399,
#49400,#49401,#49402,#49403),.UNSPECIFIED.,.T.,.F.,(4,2,2,2,2,2,2,1,1,1,
1,2,2,2,1,2,2,4),(-1.51113868430879,-1.41668987033624,-1.32224105636369,
-1.22779753479764,-1.13335401323159,-1.03891049166554,-0.94446697009949,
-0.850018156126942,-0.779181545647531,-0.755569342154394,-0.661120528181846,
-0.566671714209298,-0.472228192643248,-0.377784671077197,-0.330562910294172,
-0.283341149511147,-0.094448813972548,0.),.UNSPECIFIED.);
#886=B_SPLINE_CURVE_WITH_KNOTS('',3,(#49535,#49536,#49537,#49538,#49539,
#49540,#49541,#49542),.UNSPECIFIED.,.F.,.F.,(4,2,2,4),(0.,0.128865571792524,
0.312353805988101,0.450725664145117),.UNSPECIFIED.);
#887=B_SPLINE_CURVE_WITH_KNOTS('',3,(#49544,#49545,#49546,#49547,#49548,
#49549,#49550,#49551,#49552,#49553,#49554,#49555,#49556,#49557,#49558,#49559,
#49560,#49561,#49562,#49563,#49564,#49565,#49566,#49567,#49568,#49569),
 .UNSPECIFIED.,.F.,.F.,(4,2,2,2,2,2,2,2,2,2,2,2,4),(3.03100409690103,3.10724965658915,
3.31962805616212,3.55816001091835,3.71946361604111,3.8667157448743,4.00577882547157,
4.14436012284324,4.2798687704017,4.40986006512752,4.53061941509967,4.63980546599939,
4.72630087619969),.UNSPECIFIED.);
#888=B_SPLINE_CURVE_WITH_KNOTS('',3,(#49570,#49571,#49572,#49573,#49574,
#49575,#49576,#49577,#49578,#49579,#49580,#49581,#49582,#49583,#49584,#49585,
#49586,#49587,#49588,#49589,#49590,#49591,#49592,#49593,#49594,#49595,#49596,
#49597,#49598,#49599,#49600,#49601),.UNSPECIFIED.,.F.,.F.,(4,2,2,2,2,2,
2,2,2,2,2,2,2,2,2,4),(0.450725664145117,0.504434541071938,0.741766796410238,
1.06081742489875,1.26362192220824,1.44561364264116,1.61660881920843,1.78645082881554,
1.9531313289519,2.11323423539159,2.26278985619793,2.3977184604128,2.53060287457306,
2.68742490157839,2.91311758246269,3.03100409690103),.UNSPECIFIED.);
#889=B_SPLINE_CURVE_WITH_KNOTS('',3,(#49969,#49970,#49971,#49972,#49973,
#49974,#49975,#49976,#49977,#49978,#49979,#49980,#49981,#49982,#49983,#49984,
#49985,#49986,#49987,#49988,#49989,#49990,#49991,#49992,#49993,#49994,#49995,
#49996,#49997,#49998),.UNSPECIFIED.,.F.,.F.,(4,1,1,1,1,1,1,1,1,1,1,1,1,
1,1,1,1,1,1,1,1,1,1,1,1,1,1,4),(0.,0.0714285714285714,0.142857142857143,
0.19047619047619,0.238095238095238,0.285714285714286,0.30952380952381,0.333333333333333,
0.357142857142857,0.380952380952381,0.404761904761905,0.428571428571429,
0.464285714285714,0.5,0.535714285714286,0.571428571428571,0.607142857142857,
0.642857142857143,0.678571428571428,0.714285714285714,0.767857142857143,
0.785714285714286,0.821428571428571,0.857142857142857,0.892857142857143,
0.928571428571429,0.964285714285714,1.),.UNSPECIFIED.);
#890=B_SPLINE_CURVE_WITH_KNOTS('',3,(#50566,#50567,#50568,#50569,#50570,
#50571,#50572,#50573,#50574,#50575,#50576,#50577),.UNSPECIFIED.,.F.,.F.,
(4,2,2,2,2,4),(-0.933147704973241,-0.868188382212497,-0.834902175531159,
-0.786275576815645,-0.713790971965885,-0.697816473428944),.UNSPECIFIED.);
#891=B_SPLINE_CURVE_WITH_KNOTS('',3,(#50579,#50580,#50581,#50582,#50583,
#50584),.UNSPECIFIED.,.F.,.F.,(4,2,4),(1.52674033862511,1.66437329412415,
1.90849204295496),.UNSPECIFIED.);
#892=B_SPLINE_CURVE_WITH_KNOTS('',3,(#50585,#50586,#50587,#50588,#50589,
#50590,#50591,#50592,#50593,#50594,#50595,#50596,#50597,#50598,#50599,#50600,
#50601,#50602,#50603,#50604,#50605,#50606,#50607,#50608,#50609,#50610,#50611,
#50612,#50613,#50614,#50615,#50616,#50617,#50618,#50619,#50620,#50621,#50622,
#50623,#50624),.UNSPECIFIED.,.F.,.F.,(4,2,2,2,2,2,2,2,2,2,2,2,2,2,2,2,2,
2,2,4),(-0.697816473428944,-0.641492100456325,-0.561892654258354,-0.487270261093736,
-0.415523326738581,-0.352999977835186,-0.297288562200619,-0.245809461273269,
-0.188090467029938,-0.125165205371812,-0.0693938271837363,-0.0288166579795215,
-0.011031688571819,-0.00807673967083518,-0.00722367058716677,-0.00670135601612909,
-0.00622856149277745,-0.00563313335098952,-0.00468105421360917,0.),
 .UNSPECIFIED.);
#893=B_SPLINE_CURVE_WITH_KNOTS('',3,(#50626,#50627,#50628,#50629,#50630,
#50631,#50632,#50633,#50634,#50635,#50636,#50637,#50638,#50639,#50640,#50641,
#50642,#50643,#50644,#50645,#50646,#50647,#50648,#50649,#50650,#50651,#50652,
#50653,#50654,#50655,#50656,#50657,#50658,#50659,#50660,#50661,#50662,#50663,
#50664,#50665,#50666,#50667,#50668,#50669,#50670,#50671,#50672,#50673,#50674,
#50675,#50676,#50677,#50678,#50679,#50680,#50681,#50682,#50683,#50684,#50685,
#50686,#50687,#50688,#50689,#50690,#50691,#50692,#50693,#50694,#50695,#50696,
#50697,#50698,#50699,#50700,#50701,#50702,#50703),.UNSPECIFIED.,.T.,.F.,
(4,2,2,2,2,2,2,2,2,2,2,2,2,2,2,2,2,2,2,2,2,2,2,2,2,2,2,2,2,2,2,2,2,2,2,
2,2,2,4),(-1.16741385635012,-1.10893818912616,-1.06985976541729,-1.01498651099856,
-0.957285325740818,-0.898716427496627,-0.845101968396542,-0.7947628116729,
-0.745735950293246,-0.70071813649017,-0.666843371188012,-0.652997165338416,
-0.650589913669786,-0.649860176796543,-0.649408501557424,-0.649035642498711,
-0.64859072183499,-0.64786537956541,-0.645071095706766,-0.607574421195404,
-0.548734010794119,-0.48697591956556,-0.422962984513004,-0.359428990992207,
-0.305338489109769,-0.258926095287273,-0.213872662481025,-0.174949340171218,
-0.126693953481541,-0.0878751286972278,-0.0691962799768968,-0.066111534629531,
-0.0652308285619241,-0.0646975390346177,-0.0642131862427494,-0.0636068772368167,
-0.0626447206708484,-0.0580389183869797,0.),.UNSPECIFIED.);
#894=B_SPLINE_CURVE_WITH_KNOTS('',3,(#50706,#50707,#50708,#50709,#50710,
#50711),.UNSPECIFIED.,.F.,.F.,(4,2,4),(0.,0.505462201201323,0.508054856552492),
 .UNSPECIFIED.);
#895=B_SPLINE_CURVE_WITH_KNOTS('',3,(#50713,#50714,#50715,#50716,#50717,
#50718,#50719,#50720,#50721,#50722,#50723,#50724,#50725,#50726,#50727,#50728,
#50729,#50730,#50731),.UNSPECIFIED.,.F.,.F.,(4,2,2,2,3,2,2,2,4),(-0.23884634225481,
-0.226840467123682,-0.146855278175233,-0.0717726254858313,0.,0.0717726254858312,
0.146855278175234,0.226840467123682,0.238846342254813),.UNSPECIFIED.);
#896=B_SPLINE_CURVE_WITH_KNOTS('',3,(#50733,#50734,#50735,#50736,#50737,
#50738),.UNSPECIFIED.,.F.,.F.,(4,2,4),(-0.00355989556968658,0.,0.694034650560975),
 .UNSPECIFIED.);
#897=B_SPLINE_CURVE_WITH_KNOTS('',3,(#50740,#50741,#50742,#50743,#50744,
#50745),.UNSPECIFIED.,.F.,.F.,(4,2,4),(0.,0.0964705143506219,0.100030271138855),
 .UNSPECIFIED.);
#898=B_SPLINE_CURVE_WITH_KNOTS('',3,(#50747,#50748,#50749,#50750,#50751,
#50752,#50753,#50754,#50755,#50756,#50757,#50758,#50759,#50760,#50761,#50762,
#50763,#50764,#50765),.UNSPECIFIED.,.F.,.F.,(4,2,2,2,3,2,2,2,4),(0.891901698199051,
0.964304578588269,1.03849807176645,1.11257300217037,1.18656345354505,1.26055390491972,
1.33462883532365,1.40882232850183,1.48122520889105),.UNSPECIFIED.);
#899=B_SPLINE_CURVE_WITH_KNOTS('',3,(#50766,#50767,#50768,#50769,#50770,
#50771),.UNSPECIFIED.,.F.,.F.,(4,2,4),(-0.00355989556973241,0.,0.0964742753718417),
 .UNSPECIFIED.);
#900=B_SPLINE_CURVE_WITH_KNOTS('',3,(#50787,#50788,#50789,#50790,#50791,
#50792),.UNSPECIFIED.,.F.,.F.,(4,2,4),(9.80464399094971E-6,0.571610756625481,
0.573957203361489),.UNSPECIFIED.);
#901=B_SPLINE_CURVE_WITH_KNOTS('',3,(#50794,#50795,#50796,#50797,#50798,
#50799,#50800,#50801,#50802,#50803,#50804),.UNSPECIFIED.,.F.,.F.,(4,3,2,
2,4),(-0.000224177666558713,0.,0.070831562509613,0.146325160065373,0.2126836341045),
 .UNSPECIFIED.);
#902=B_SPLINE_CURVE_WITH_KNOTS('',3,(#50806,#50807,#50808,#50809,#50810,
#50811),.UNSPECIFIED.,.F.,.F.,(4,2,4),(5.93567910240686,6.07331205917363,
6.14204532250066),.UNSPECIFIED.);
#903=B_SPLINE_CURVE_WITH_KNOTS('',3,(#50813,#50814,#50815,#50816,#50817,
#50818,#50819,#50820,#50821,#50822,#50823,#50824,#50825,#50826,#50827,#50828,
#50829,#50830,#50831,#50832,#50833,#50834,#50835,#50836,#50837,#50838),
 .UNSPECIFIED.,.F.,.F.,(4,2,2,2,2,2,2,2,2,2,2,2,4),(-0.217220359894287,
-0.188091234086745,-0.125165638249208,-0.0693942084995795,-0.0288171491726731,
-0.0110319711967647,-0.00807696643551894,-0.00722387847193592,-0.00670155176446524,
-0.00622874591968683,-0.00563330291795246,-0.0046811987490239,0.),
 .UNSPECIFIED.);
#904=B_SPLINE_CURVE_WITH_KNOTS('',3,(#50840,#50841,#50842,#50843,#50844,
#50845,#50846,#50847,#50848,#50849,#50850,#50851,#50852,#50853,#50854,#50855,
#50856,#50857),.UNSPECIFIED.,.F.,.F.,(4,2,2,2,2,2,2,2,4),(-0.631559418815847,
-0.620592602298802,-0.55666742562014,-0.487473041324762,-0.420697012696697,
-0.353000616097942,-0.297289069423837,-0.245809975607455,-0.217220359894287),
 .UNSPECIFIED.);
#905=B_SPLINE_CURVE_WITH_KNOTS('',3,(#50858,#50859,#50860,#50861,#50862,
#50863),.UNSPECIFIED.,.F.,.F.,(4,2,4),(-0.00341976532710713,0.,0.574420226027791),
 .UNSPECIFIED.);
#906=B_SPLINE_CURVE_WITH_KNOTS('',3,(#50865,#50866,#50867,#50868,#50869,
#50870,#50871,#50872,#50873,#50874,#50875,#50876,#50877,#50878,#50879,#50880,
#50881,#50882,#50883,#50884,#50885,#50886,#50887,#50888,#50889,#50890,#50891,
#50892,#50893,#50894,#50895,#50896,#50897,#50898,#50899,#50900,#50901,#50902,
#50903,#50904,#50905,#50906,#50907,#50908,#50909,#50910,#50911,#50912,#50913,
#50914,#50915,#50916,#50917,#50918,#50919,#50920,#50921,#50922,#50923,#50924,
#50925,#50926,#50927,#50928,#50929,#50930,#50931,#50932,#50933,#50934,#50935,
#50936,#50937,#50938,#50939,#50940,#50941,#50942),.UNSPECIFIED.,.T.,.F.,
(4,2,2,2,2,2,2,2,2,2,2,2,2,2,2,2,2,2,2,2,2,2,2,2,2,2,2,2,2,2,2,2,2,2,2,
2,2,2,4),(-1.17168724851018,-1.13237503013972,-1.09879160541631,-1.03889691152247,
-0.981512507143146,-0.933213815656585,-0.888967230915786,-0.842464807937823,
-0.794362427770576,-0.753634236924923,-0.729805391435721,-0.726300945076248,
-0.725393129119785,-0.724861929520477,-0.724439462673908,-0.723953337160863,
-0.723043143227618,-0.7198098911947,-0.676758603427299,-0.614155893881885,
-0.553909544915966,-0.497500965420826,-0.437567654472521,-0.378252271962478,
-0.324152481036834,-0.273011005634134,-0.22337038625395,-0.178756642448113,
-0.146924605801202,-0.134819177627514,-0.133668424425745,-0.133121159543081,
-0.132739051473177,-0.132344954721629,-0.131807139835994,-0.130466280257678,
-0.116500318328084,-0.0541945170664063,0.),.UNSPECIFIED.);
#907=B_SPLINE_CURVE_WITH_KNOTS('',3,(#50950,#50951,#50952,#50953,#50954,
#50955,#50956,#50957,#50958,#50959,#50960,#50961,#50962,#50963,#50964,#50965),
 .UNSPECIFIED.,.F.,.F.,(4,2,2,2,2,2,2,4),(-0.892813994576797,-0.891702748036019,
-0.737380938279843,-0.613095387365794,-0.519181223685694,-0.442588537124146,
-0.369088033168532,-0.363543775985196),.UNSPECIFIED.);
#908=B_SPLINE_CURVE_WITH_KNOTS('',3,(#56488,#56489,#56490,#56491,#56492,
#56493,#56494,#56495,#56496,#56497,#56498,#56499,#56500,#56501,#56502,#56503,
#56504,#56505,#56506,#56507,#56508,#56509,#56510,#56511,#56512,#56513,#56514,
#56515,#56516,#56517,#56518,#56519,#56520,#56521,#56522,#56523,#56524,#56525,
#56526,#56527,#56528,#56529,#56530,#56531,#56532,#56533,#56534,#56535,#56536,
#56537,#56538,#56539,#56540,#56541,#56542,#56543,#56544,#56545,#56546,#56547,
#56548,#56549,#56550,#56551,#56552,#56553,#56554,#56555,#56556,#56557,#56558,
#56559,#56560,#56561,#56562,#56563,#56564,#56565,#56566,#56567,#56568,#56569,
#56570,#56571,#56572,#56573,#56574,#56575,#56576,#56577,#56578,#56579,#56580,
#56581,#56582,#56583,#56584,#56585,#56586,#56587,#56588,#56589,#56590,#56591,
#56592,#56593,#56594,#56595,#56596,#56597,#56598,#56599,#56600,#56601,#56602,
#56603,#56604,#56605,#56606,#56607,#56608,#56609,#56610,#56611,#56612,#56613,
#56614,#56615,#56616,#56617,#56618,#56619,#56620,#56621,#56622,#56623,#56624,
#56625,#56626,#56627,#56628,#56629,#56630,#56631,#56632,#56633,#56634,#56635,
#56636,#56637,#56638,#56639,#56640,#56641,#56642,#56643,#56644,#56645,#56646,
#56647,#56648,#56649,#56650,#56651,#56652,#56653,#56654,#56655,#56656,#56657,
#56658,#56659,#56660,#56661,#56662,#56663,#56664,#56665,#56666,#56667,#56668,
#56669,#56670,#56671,#56672,#56673,#56674,#56675,#56676,#56677,#56678,#56679,
#56680,#56681,#56682,#56683,#56684,#56685,#56686,#56687,#56688,#56689,#56690,
#56691,#56692,#56693,#56694,#56695,#56696,#56697,#56698,#56699,#56700,#56701,
#56702,#56703,#56704,#56705,#56706,#56707,#56708,#56709,#56710,#56711,#56712,
#56713,#56714,#56715,#56716,#56717,#56718,#56719,#56720,#56721,#56722,#56723,
#56724,#56725,#56726,#56727,#56728,#56729,#56730,#56731,#56732,#56733,#56734,
#56735,#56736,#56737,#56738,#56739,#56740,#56741,#56742,#56743,#56744,#56745,
#56746,#56747,#56748,#56749,#56750,#56751,#56752,#56753,#56754,#56755,#56756,
#56757,#56758,#56759,#56760,#56761,#56762,#56763,#56764,#56765,#56766,#56767,
#56768,#56769,#56770,#56771,#56772,#56773,#56774,#56775,#56776,#56777,#56778,
#56779,#56780,#56781,#56782,#56783,#56784,#56785,#56786,#56787,#56788,#56789,
#56790,#56791,#56792,#56793,#56794,#56795,#56796,#56797,#56798,#56799,#56800,
#56801,#56802,#56803,#56804,#56805,#56806,#56807,#56808,#56809,#56810,#56811,
#56812,#56813,#56814,#56815,#56816,#56817,#56818,#56819,#56820,#56821,#56822,
#56823,#56824,#56825,#56826,#56827,#56828,#56829,#56830,#56831,#56832,#56833,
#56834,#56835,#56836,#56837,#56838,#56839,#56840,#56841,#56842,#56843,#56844,
#56845,#56846,#56847,#56848,#56849,#56850,#56851,#56852,#56853,#56854,#56855,
#56856,#56857,#56858,#56859,#56860,#56861,#56862,#56863,#56864,#56865,#56866,
#56867,#56868,#56869,#56870,#56871,#56872,#56873,#56874,#56875,#56876,#56877,
#56878,#56879,#56880,#56881,#56882,#56883,#56884,#56885,#56886,#56887,#56888,
#56889,#56890,#56891,#56892,#56893,#56894,#56895,#56896,#56897,#56898,#56899,
#56900,#56901,#56902,#56903,#56904,#56905,#56906,#56907,#56908,#56909,#56910,
#56911,#56912,#56913,#56914,#56915,#56916,#56917,#56918,#56919,#56920,#56921,
#56922,#56923,#56924,#56925,#56926,#56927,#56928,#56929,#56930,#56931,#56932,
#56933,#56934,#56935,#56936,#56937,#56938,#56939,#56940,#56941,#56942,#56943,
#56944,#56945,#56946,#56947,#56948,#56949,#56950,#56951,#56952,#56953,#56954,
#56955,#56956,#56957,#56958,#56959,#56960,#56961,#56962,#56963,#56964,#56965,
#56966,#56967,#56968,#56969,#56970,#56971,#56972,#56973,#56974,#56975,#56976,
#56977,#56978,#56979,#56980,#56981,#56982,#56983,#56984,#56985,#56986,#56987,
#56988,#56989),.UNSPECIFIED.,.F.,.F.,(4,1,1,1,1,1,1,1,1,1,1,1,1,1,1,1,1,
1,1,1,1,1,1,1,1,1,1,1,1,1,1,1,1,1,1,1,1,1,1,1,1,1,1,1,1,1,1,1,1,1,1,1,1,
1,1,1,1,1,1,1,1,1,1,1,1,1,1,1,1,1,1,1,1,1,1,1,1,1,1,1,1,1,1,1,1,1,1,1,1,
1,1,1,1,1,1,1,1,1,1,1,1,1,1,1,1,1,1,1,1,1,1,1,1,1,1,1,1,1,1,1,1,1,1,1,1,
1,1,1,1,1,1,1,1,1,1,1,1,1,1,1,1,1,1,1,1,1,1,1,1,1,1,1,1,1,1,1,1,1,1,1,1,
1,1,1,1,1,1,1,1,1,1,1,1,1,1,1,1,1,1,1,1,1,1,1,1,1,1,1,1,1,1,1,1,1,1,1,1,
1,1,1,1,1,1,1,1,1,1,1,1,1,1,1,1,1,1,1,1,1,1,1,1,1,1,1,1,1,1,1,1,1,1,1,1,
1,1,1,1,1,1,1,1,1,1,1,1,1,1,1,1,1,1,1,1,1,1,1,1,1,1,1,1,1,1,1,1,1,1,1,1,
1,1,1,1,1,1,1,1,1,1,1,1,1,1,1,1,1,1,1,1,1,1,1,1,1,1,1,1,1,1,1,1,1,1,1,1,
1,1,1,1,1,1,1,1,1,1,1,1,1,1,1,1,1,1,1,1,1,1,1,1,1,1,1,1,1,1,1,1,1,1,1,1,
1,1,1,1,1,1,1,1,1,1,1,1,1,1,1,1,1,1,1,1,1,1,1,1,1,1,1,1,1,1,1,1,1,1,1,1,
1,1,1,1,1,1,1,1,1,1,1,1,1,1,1,1,1,1,1,1,1,1,1,1,1,1,1,1,1,1,1,1,1,1,1,1,
1,1,1,1,1,1,1,1,1,1,1,1,1,1,1,1,1,1,1,1,1,1,1,1,1,1,1,1,1,1,1,1,1,1,1,1,
1,1,1,1,1,1,1,1,1,1,1,1,1,1,1,1,1,1,1,1,1,1,1,1,1,1,1,1,1,1,1,1,1,1,1,1,
1,1,1,1,1,1,1,1,1,1,1,1,1,1,4),(0.000669054243018642,0.00167410714285714,
0.00223214285714286,0.00334821428571429,0.00446428571428571,0.00558035714285714,
0.00669642857142857,0.00892857142857143,0.0111607142857143,0.0133928571428571,
0.015625,0.0178571428571429,0.0200892857142857,0.0223214285714286,0.0245535714285714,
0.0267857142857143,0.0290178571428571,0.03125,0.0334821428571429,0.0357142857142857,
0.0379464285714286,0.0401785714285714,0.0424107142857143,0.0446428571428571,
0.046875,0.0491071428571428,0.0513392857142857,0.0535714285714286,0.0558035714285714,
0.0580357142857143,0.0602678571428571,0.0625,0.0647321428571428,0.0669642857142857,
0.0680803571428572,0.0691964285714286,0.0714285714285714,0.0736607142857143,
0.0758928571428571,0.078125,0.0803571428571428,0.0825892857142857,0.0848214285714286,
0.0870535714285714,0.0892857142857143,0.0915178571428571,0.09375,0.0959821428571428,
0.0982142857142857,0.100446428571429,0.102678571428571,0.104910714285714,
0.107142857142857,0.109375,0.111607142857143,0.113839285714286,0.116071428571429,
0.118303571428571,0.119419642857143,0.120535714285714,0.122767857142857,
0.125,0.127232142857143,0.129464285714286,0.131696428571429,0.133928571428571,
0.136160714285714,0.138392857142857,0.140625,0.142857142857143,0.144345238095238,
0.145833333333333,0.146205357142857,0.146577380952381,0.146949404761905,
0.147321428571429,0.148809523809524,0.150297619047619,0.151785714285714,
0.15327380952381,0.154761904761905,0.15625,0.157738095238095,0.160714285714286,
0.162202380952381,0.162946428571429,0.163690476190476,0.165178571428571,
0.165550595238095,0.165922619047619,0.166294642857143,0.166480654761905,
0.166666666666667,0.169312169312169,0.171957671957672,0.172839506172839,
0.173721340388007,0.174162257495591,0.174603174603175,0.177248677248677,
0.17989417989418,0.182539682539683,0.18452380952381,0.186507936507937,0.188492063492063,
0.19047619047619,0.191468253968254,0.192460317460317,0.193452380952381,
0.193948412698413,0.194444444444444,0.196428571428571,0.198412698412698,
0.200396825396825,0.202380952380952,0.202876984126984,0.203373015873016,
0.204365079365079,0.206349206349206,0.206597222222222,0.206845238095238,
0.207093253968254,0.20734126984127,0.207589285714286,0.207837301587302,
0.208333333333333,0.21031746031746,0.212301587301587,0.214285714285714,
0.216269841269841,0.218253968253968,0.220238095238095,0.222222222222222,
0.222883597883598,0.223544973544974,0.224867724867725,0.227513227513228,
0.23015873015873,0.232804232804233,0.235449735449735,0.238095238095238,
0.239583333333333,0.241071428571429,0.244047619047619,0.247023809523809,
0.25,0.25297619047619,0.255952380952381,0.258928571428571,0.260416666666667,
0.261904761904762,0.263392857142857,0.264880952380952,0.267857142857143,
0.270833333333333,0.273809523809524,0.276785714285714,0.279761904761905,
0.282738095238095,0.285714285714286,0.288690476190476,0.291666666666667,
0.294642857142857,0.297619047619048,0.300595238095238,0.303571428571429,
0.306547619047619,0.30952380952381,0.3125,0.31547619047619,0.318452380952381,
0.321428571428571,0.324404761904762,0.327380952380952,0.328869047619048,
0.330357142857143,0.333333333333333,0.336309523809524,0.339285714285714,
0.342261904761905,0.345238095238095,0.348214285714286,0.351190476190476,
0.354166666666667,0.357142857142857,0.360119047619048,0.363095238095238,
0.366071428571428,0.367559523809524,0.369047619047619,0.370535714285714,
0.37202380952381,0.373511904761905,0.375,0.376488095238095,0.37797619047619,
0.378720238095238,0.379464285714286,0.380952380952381,0.383928571428571,
0.386904761904762,0.389880952380952,0.391369047619048,0.392113095238095,
0.392857142857143,0.394345238095238,0.395833333333333,0.398809523809524,
0.401785714285714,0.404761904761905,0.407738095238095,0.40922619047619,
0.410714285714286,0.411458333333333,0.411830357142857,0.412202380952381,
0.412946428571429,0.413690476190476,0.415178571428571,0.416666666666667,
0.418154761904762,0.419642857142857,0.421130952380952,0.422619047619048,
0.424107142857143,0.425595238095238,0.427083333333333,0.427827380952381,
0.428571428571429,0.430803571428571,0.433035714285714,0.435267857142857,
0.4375,0.439732142857143,0.441964285714286,0.444196428571429,0.446428571428571,
0.447544642857143,0.448660714285714,0.450892857142857,0.453125,0.455357142857143,
0.457589285714286,0.459821428571429,0.462053571428571,0.464285714285714,
0.466517857142857,0.46875,0.470982142857143,0.472098214285714,0.473214285714286,
0.475446428571429,0.477678571428571,0.479910714285714,0.482142857142857,
0.484375,0.486607142857143,0.488839285714286,0.491071428571429,0.493303571428571,
0.495535714285714,0.497767857142857,0.5,0.502232142857143,0.504464285714286,
0.506696428571429,0.508928571428571,0.511160714285714,0.513392857142857,
0.515625,0.517857142857143,0.520089285714286,0.522321428571428,0.524553571428571,
0.526785714285714,0.529017857142857,0.53125,0.533482142857143,0.535714285714286,
0.537946428571429,0.540178571428571,0.542410714285714,0.544642857142857,
0.545200892857143,0.545758928571429,0.546875,0.549107142857143,0.551339285714286,
0.553571428571429,0.555803571428571,0.558035714285714,0.560267857142857,
0.5625,0.564732142857143,0.566964285714286,0.569196428571429,0.571428571428571,
0.573660714285714,0.575892857142857,0.578125,0.580357142857143,0.582589285714286,
0.584821428571428,0.587053571428571,0.589285714285714,0.591517857142857,
0.59375,0.595982142857143,0.598214285714286,0.600446428571428,0.602678571428571,
0.604910714285714,0.607142857142857,0.609375,0.611607142857143,0.613839285714286,
0.616071428571429,0.618303571428571,0.620535714285714,0.622767857142857,
0.625,0.627232142857143,0.629464285714286,0.631696428571429,0.633928571428571,
0.636160714285714,0.638392857142857,0.640625,0.642857142857143,0.644345238095238,
0.645833333333333,0.648809523809524,0.651785714285714,0.654761904761905,
0.657738095238095,0.660714285714286,0.663690476190476,0.665178571428571,
0.666666666666667,0.667989417989418,0.669312169312169,0.671957671957672,
0.674603174603175,0.675925925925926,0.677248677248677,0.67989417989418,
0.682539682539682,0.684523809523809,0.686507936507936,0.688492063492063,
0.69047619047619,0.692460317460317,0.694444444444444,0.696428571428571,
0.697420634920635,0.698412698412698,0.701058201058201,0.703703703703704,
0.705026455026455,0.706349206349206,0.707671957671958,0.71031746031746,
0.712301587301587,0.714285714285714,0.716517857142857,0.71875,0.720982142857143,
0.72265625,0.723214285714286,0.724702380952381,0.726190476190476,0.727678571428571,
0.729166666666667,0.730654761904762,0.732142857142857,0.733258928571428,
0.734375,0.736607142857143,0.738839285714286,0.741071428571428,0.743303571428571,
0.745535714285714,0.747767857142857,0.75,0.752232142857143,0.754464285714286,
0.756696428571428,0.758928571428571,0.761160714285714,0.763392857142857,
0.765625,0.767857142857143,0.770089285714286,0.772321428571428,0.774553571428571,
0.776785714285714,0.779017857142857,0.78125,0.783482142857143,0.785714285714286,
0.787946428571428,0.790178571428571,0.792410714285714,0.794642857142857,
0.796875,0.799107142857143,0.801339285714286,0.803571428571428,0.805803571428571,
0.808035714285714,0.810267857142857,0.8125,0.814732142857143,0.816964285714286,
0.819196428571429,0.821428571428571,0.823660714285714,0.825892857142857,
0.828125,0.830357142857143,0.832589285714286,0.834821428571428,0.837053571428571,
0.839285714285714,0.841517857142857,0.84375,0.845982142857143,0.848214285714286,
0.850446428571428,0.852678571428571,0.854910714285714,0.857142857142857,
0.859375,0.861607142857143,0.863839285714286,0.866071428571429,0.868303571428571,
0.870535714285714,0.872767857142857,0.875,0.877232142857143,0.879464285714286,
0.881696428571429,0.883928571428571,0.886160714285714,0.888392857142857,
0.890625,0.892857142857143,0.895089285714286,0.897321428571428,0.899553571428571,
0.901785714285714,0.904017857142857,0.90625,0.908482142857143,0.910714285714286,
0.912946428571429,0.915178571428571,0.917410714285714,0.919642857142857,
0.921875,0.922991071428571,0.924107142857143,0.926339285714286,0.928571428571429,
0.930803571428571,0.933035714285714,0.935267857142857,0.9375,0.939732142857143,
0.941964285714286,0.944196428571429,0.946428571428571,0.948660714285714,
0.950892857142857,0.953125,0.955357142857143,0.957589285714286,0.959821428571429,
0.962053571428571,0.964285714285714,0.966517857142857,0.96875,0.970982142857143,
0.973214285714286,0.975446428571429,0.977678571428572,0.979910714285714,
0.982142857142857,0.984375,0.986607142857143,0.988839285714286,0.991071428571429,
0.993303571428571,0.994419642857143,0.995535714285714,0.996651785714286,
0.997767857142857,0.998883928571429,0.999194256023389),.UNSPECIFIED.);
#909=B_SPLINE_CURVE_WITH_KNOTS('',3,(#56996,#56997,#56998,#56999,#57000,
#57001,#57002,#57003,#57004,#57005),.UNSPECIFIED.,.F.,.F.,(4,3,3,4),(-4.09323272002469,
-3.95713141738306,-2.9678485630373,-2.06652207565085),.UNSPECIFIED.);
#910=B_SPLINE_CURVE_WITH_KNOTS('',3,(#57008,#57009,#57010,#57011,#57012,
#57013,#57014,#57015,#57016,#57017),.UNSPECIFIED.,.F.,.F.,(4,3,3,4),(0.,
0.494641427172876,0.989282854345763,1.11488200921591),.UNSPECIFIED.);
#911=B_SPLINE_CURVE_WITH_KNOTS('',3,(#57022,#57023,#57024,#57025,#57026,
#57027,#57028,#57029,#57030,#57031,#57032,#57033,#57034,#57035,#57036,#57037,
#57038,#57039,#57040,#57041,#57042,#57043),.UNSPECIFIED.,.F.,.F.,(4,3,3,
3,3,3,3,4),(-10.3764180272043,-9.89282854345765,-8.90354568911189,-7.91426283476612,
-6.92497998042036,-5.93569712607459,-4.94641427172883,-4.09323272002469),
 .UNSPECIFIED.);
#912=B_SPLINE_CURVE_WITH_KNOTS('',3,(#57044,#57045,#57046,#57047,#57048,
#57049,#57050,#57051,#57052,#57053,#57054,#57055,#57056,#57057,#57058,#57059,
#57060,#57061,#57062,#57063,#57064,#57065),.UNSPECIFIED.,.F.,.F.,(4,3,3,
3,3,3,3,4),(1.11488200921591,1.97856570869153,2.9678485630373,3.95713141738306,
4.94641427172883,5.93569712607459,6.92497998042036,7.39806731639549),
 .UNSPECIFIED.);
#913=B_SPLINE_CURVE_WITH_KNOTS('',3,(#57070,#57071,#57072,#57073,#57074,
#57075,#57076,#57077,#57078,#57079,#57080,#57081,#57082,#57083,#57084,#57085,
#57086,#57087,#57088,#57089,#57090,#57091),.UNSPECIFIED.,.F.,.F.,(4,3,3,
3,3,3,3,4),(-16.6596033343839,-15.8285256695322,-14.8392428151865,-13.8499599608407,
-12.860677106495,-11.8713942521492,-10.8821113978034,-10.3764180272043),
 .UNSPECIFIED.);
#914=B_SPLINE_CURVE_WITH_KNOTS('',3,(#57092,#57093,#57094,#57095,#57096,
#57097,#57098,#57099,#57100,#57101,#57102,#57103,#57104,#57105,#57106,#57107,
#57108,#57109,#57110,#57111,#57112,#57113),.UNSPECIFIED.,.F.,.F.,(4,3,3,
3,3,3,3,4),(7.39806731639549,7.91426283476612,8.90354568911189,9.89282854345766,
10.8821113978034,11.8713942521492,12.860677106495,13.6812526235751),
 .UNSPECIFIED.);
#915=B_SPLINE_CURVE_WITH_KNOTS('',3,(#57118,#57119,#57120,#57121,#57122,
#57123,#57124,#57125,#57126,#57127,#57128,#57129,#57130,#57131,#57132,#57133,
#57134,#57135,#57136,#57137,#57138,#57139,#57140,#57141,#57142),
 .UNSPECIFIED.,.F.,.F.,(4,3,3,3,3,3,3,3,4),(-22.9427886415635,-22.7535056499526,
-21.7642227956068,-20.7749399412611,-19.7856570869153,-18.7963742325695,
-17.8070913782238,-16.817808523878,-16.6596033343839),.UNSPECIFIED.);
#916=B_SPLINE_CURVE_WITH_KNOTS('',3,(#57143,#57144,#57145,#57146,#57147,
#57148,#57149,#57150,#57151,#57152,#57153,#57154,#57155,#57156,#57157,#57158,
#57159,#57160,#57161,#57162,#57163,#57164,#57165,#57166,#57167),
 .UNSPECIFIED.,.F.,.F.,(4,3,3,3,3,3,3,3,4),(13.6812526235751,13.8499599608407,
14.8392428151865,15.8285256695323,16.817808523878,17.8070913782238,18.7963742325695,
19.7856570869153,19.9644379307547),.UNSPECIFIED.);
#917=B_SPLINE_CURVE_WITH_KNOTS('',3,(#57172,#57173,#57174,#57175,#57176,
#57177,#57178,#57179,#57180,#57181,#57182,#57183,#57184,#57185,#57186,#57187,
#57188,#57189,#57190,#57191,#57192,#57193),.UNSPECIFIED.,.F.,.F.,(4,3,3,
3,3,3,3,4),(-29.225973948743,-28.6892027760272,-27.6999199216814,-26.7106370673357,
-25.7213542129899,-24.7320713586441,-23.7427885042984,-22.9427886415635),
 .UNSPECIFIED.);
#918=B_SPLINE_CURVE_WITH_KNOTS('',3,(#57194,#57195,#57196,#57197,#57198,
#57199,#57200,#57201,#57202,#57203,#57204,#57205,#57206,#57207,#57208,#57209,
#57210,#57211,#57212,#57213,#57214,#57215),.UNSPECIFIED.,.F.,.F.,(4,3,3,
3,3,3,3,4),(19.9644379307547,20.7749399412611,21.7642227956068,22.7535056499526,
23.7427885042984,24.7320713586441,25.7213542129899,26.2476232379343),
 .UNSPECIFIED.);
#919=B_SPLINE_CURVE_WITH_KNOTS('',3,(#57220,#57221,#57222,#57223,#57224,
#57225,#57226,#57227,#57228,#57229,#57230,#57231,#57232,#57233,#57234,#57235,
#57236,#57237,#57238,#57239,#57240,#57241),.UNSPECIFIED.,.F.,.F.,(4,3,3,
3,3,3,3,4),(-35.5091592559226,-34.6248999021018,-33.635617047756,-32.6463341934103,
-31.6570513390645,-30.6677684847187,-29.678485630373,-29.225973948743),
 .UNSPECIFIED.);
#920=B_SPLINE_CURVE_WITH_KNOTS('',3,(#57242,#57243,#57244,#57245,#57246,
#57247,#57248,#57249,#57250,#57251,#57252,#57253,#57254,#57255,#57256,#57257,
#57258,#57259,#57260,#57261,#57262,#57263),.UNSPECIFIED.,.F.,.F.,(4,3,3,
3,3,3,3,4),(26.2476232379343,26.7106370673357,27.6999199216814,28.6892027760272,
29.678485630373,30.6677684847187,31.6570513390645,32.5308085451138),
 .UNSPECIFIED.);
#921=B_SPLINE_CURVE_WITH_KNOTS('',3,(#57268,#57269,#57270,#57271,#57272,
#57273,#57274,#57275,#57276,#57277,#57278,#57279,#57280,#57281,#57282,#57283,
#57284,#57285,#57286,#57287,#57288,#57289,#57290,#57291,#57292),
 .UNSPECIFIED.,.F.,.F.,(4,3,3,3,3,3,3,3,4),(-41.7923445631022,-41.5498798825222,
-40.5605970281764,-39.5713141738306,-38.5820313194849,-37.5927484651391,
-36.6034656107933,-35.6141827564476,-35.5091592559226),.UNSPECIFIED.);
#922=B_SPLINE_CURVE_WITH_KNOTS('',3,(#57293,#57294,#57295,#57296,#57297,
#57298,#57299,#57300,#57301,#57302,#57303,#57304,#57305,#57306,#57307,#57308,
#57309,#57310,#57311,#57312,#57313,#57314,#57315,#57316,#57317),
 .UNSPECIFIED.,.F.,.F.,(4,3,3,3,3,3,3,3,4),(32.5308085451138,32.6463341934103,
33.635617047756,34.6248999021018,35.6141827564476,36.6034656107933,37.5927484651391,
38.5820313194849,38.8139938522934),.UNSPECIFIED.);
#923=B_SPLINE_CURVE_WITH_KNOTS('',3,(#57322,#57323,#57324,#57325,#57326,
#57327,#57328,#57329,#57330,#57331,#57332,#57333,#57334,#57335,#57336,#57337,
#57338,#57339,#57340,#57341,#57342,#57343),.UNSPECIFIED.,.F.,.F.,(4,3,3,
3,3,3,3,4),(-48.0755298702818,-47.4855770085967,-46.496294154251,-45.5070112999052,
-44.5177284455594,-43.5284455912137,-42.5391627368679,-41.7923445631022),
 .UNSPECIFIED.);
#924=B_SPLINE_CURVE_WITH_KNOTS('',3,(#57344,#57345,#57346,#57347,#57348,
#57349,#57350,#57351,#57352,#57353,#57354,#57355,#57356,#57357,#57358,#57359,
#57360,#57361,#57362,#57363,#57364,#57365),.UNSPECIFIED.,.F.,.F.,(4,3,3,
3,3,3,3,4),(38.8139938522934,39.5713141738306,40.5605970281764,41.5498798825221,
42.5391627368679,43.5284455912137,44.5177284455594,45.097179159473),
 .UNSPECIFIED.);
#925=B_SPLINE_CURVE_WITH_KNOTS('',3,(#57370,#57371,#57372,#57373,#57374,
#57375,#57376,#57377,#57378,#57379,#57380,#57381,#57382,#57383,#57384,#57385,
#57386,#57387,#57388,#57389,#57390,#57391),.UNSPECIFIED.,.F.,.F.,(4,3,3,
3,3,3,3,4),(-54.3587151774614,-53.4212741346713,-52.4319912803256,-51.4427084259798,
-50.453425571634,-49.4641427172883,-48.4748598629425,-48.0755298702818),
 .UNSPECIFIED.);
#926=B_SPLINE_CURVE_WITH_KNOTS('',3,(#57392,#57393,#57394,#57395,#57396,
#57397,#57398,#57399,#57400,#57401,#57402,#57403,#57404,#57405,#57406,#57407,
#57408,#57409,#57410,#57411,#57412,#57413),.UNSPECIFIED.,.F.,.F.,(4,3,3,
3,3,3,3,4),(45.097179159473,45.5070112999052,46.496294154251,47.4855770085967,
48.4748598629425,49.4641427172883,50.4534255716341,51.3803644666526),
 .UNSPECIFIED.);
#927=B_SPLINE_CURVE_WITH_KNOTS('',3,(#57418,#57419,#57420,#57421,#57422,
#57423,#57424,#57425,#57426,#57427,#57428,#57429,#57430,#57431,#57432,#57433,
#57434,#57435,#57436,#57437,#57438,#57439,#57440,#57441,#57442),
 .UNSPECIFIED.,.F.,.F.,(4,3,3,3,3,3,3,3,4),(-60.641900484641,-60.3462541150917,
-59.3569712607459,-58.3676884064002,-57.3784055520544,-56.3891226977086,
-55.3998398433629,-54.4105569890171,-54.3587151774614),.UNSPECIFIED.);
#928=B_SPLINE_CURVE_WITH_KNOTS('',3,(#57443,#57444,#57445,#57446,#57447,
#57448,#57449,#57450,#57451,#57452,#57453,#57454,#57455,#57456,#57457,#57458,
#57459,#57460,#57461,#57462,#57463,#57464,#57465,#57466,#57467),
 .UNSPECIFIED.,.F.,.F.,(4,3,3,3,3,3,3,3,4),(51.3803644666526,51.4427084259798,
52.4319912803256,53.4212741346713,54.4105569890171,55.3998398433629,56.3891226977086,
57.3784055520544,57.6635497738322),.UNSPECIFIED.);
#929=B_SPLINE_CURVE_WITH_KNOTS('',3,(#57472,#57473,#57474,#57475,#57476,
#57477,#57478,#57479,#57480,#57481,#57482,#57483,#57484,#57485,#57486,#57487,
#57488,#57489,#57490,#57491,#57492,#57493),.UNSPECIFIED.,.F.,.F.,(4,3,3,
3,3,3,3,4),(-66.9250857918206,-66.2819512411663,-65.2926683868205,-64.3033855324747,
-63.314102678129,-62.3248198237832,-61.3355369694375,-60.641900484641),
 .UNSPECIFIED.);
#930=B_SPLINE_CURVE_WITH_KNOTS('',3,(#57494,#57495,#57496,#57497,#57498,
#57499,#57500,#57501,#57502,#57503,#57504,#57505,#57506,#57507,#57508,#57509,
#57510,#57511,#57512,#57513,#57514,#57515),.UNSPECIFIED.,.F.,.F.,(4,3,3,
3,3,3,3,4),(57.6635497738322,58.3676884064002,59.3569712607459,60.3462541150917,
61.3355369694375,62.3248198237832,63.314102678129,63.9467350810118),
 .UNSPECIFIED.);
#931=B_SPLINE_CURVE_WITH_KNOTS('',3,(#57521,#57522,#57523,#57524,#57525),
 .UNSPECIFIED.,.F.,.F.,(4,1,4),(78.5398163397448,78.8859646434363,79.7872911308227),
 .UNSPECIFIED.);
#932=B_SPLINE_CURVE_WITH_KNOTS('',3,(#57528,#57529,#57530,#57531),
 .UNSPECIFIED.,.F.,.F.,(4,4),(78.5398163397448,78.5489786101027),
 .UNSPECIFIED.);
#933=B_SPLINE_CURVE_WITH_KNOTS('',3,(#57536,#57537,#57538,#57539,#57540,
#57541,#57542,#57543,#57544,#57545),.UNSPECIFIED.,.F.,.F.,(4,1,1,1,1,1,
1,4),(72.2566310325653,72.9502675173617,73.9395503717074,74.9288332260532,
75.918116080399,76.9073989347447,77.8966817890905,78.5398163397448),
 .UNSPECIFIED.);
#934=B_SPLINE_CURVE_WITH_KNOTS('',3,(#57546,#57547,#57548,#57549,#57550,
#57551,#57552,#57553,#57554,#57555,#57556),.UNSPECIFIED.,.F.,.F.,(4,1,1,
1,1,1,1,1,4),(72.2566310325652,72.6132814840281,73.6025643383739,74.5918471927197,
75.5811300470654,76.5704129014112,77.5596957557569,78.0543371829298,78.5398163397448),
 .UNSPECIFIED.);
#935=B_SPLINE_CURVE_WITH_KNOTS('',3,(#57561,#57562,#57563,#57564,#57565,
#57566,#57567,#57568,#57569,#57570,#57571),.UNSPECIFIED.,.F.,.F.,(4,1,1,
1,1,1,1,1,4),(65.9734457253856,66.0252875369413,67.0145703912871,68.0038532456329,
68.9931360999786,69.9824189543244,70.9717018086701,71.9609846630159,72.2566310325653),
 .UNSPECIFIED.);
#936=B_SPLINE_CURVE_WITH_KNOTS('',3,(#57572,#57573,#57574,#57575,#57576,
#57577,#57578,#57579,#57580,#57581),.UNSPECIFIED.,.F.,.F.,(4,1,1,1,1,1,
1,4),(65.9734457253856,66.6775843579535,67.6668672122993,68.6561500666451,
69.6454329209908,70.6347157753366,71.6239986296824,72.2566310325652),
 .UNSPECIFIED.);
#937=B_SPLINE_CURVE_WITH_KNOTS('',3,(#57586,#57587,#57588,#57589,#57590,
#57591,#57592,#57593,#57594,#57595),.UNSPECIFIED.,.F.,.F.,(4,1,1,1,1,1,
1,4),(59.6902604182061,60.0895904108667,61.0788732652125,62.0681561195583,
63.057438973904,64.0467218282498,65.0360046825956,65.9734457253856),
 .UNSPECIFIED.);
#938=B_SPLINE_CURVE_WITH_KNOTS('',3,(#57596,#57597,#57598,#57599,#57600,
#57601,#57602,#57603,#57604,#57605,#57606),.UNSPECIFIED.,.F.,.F.,(4,1,1,
1,1,1,1,1,4),(59.6902604182061,59.7526043775332,60.7418872318789,61.7311700862247,
62.7204529405705,63.7097357949162,64.699018649262,65.6883015036078,65.9734457253856),
 .UNSPECIFIED.);
#939=B_SPLINE_CURVE_WITH_KNOTS('',3,(#57611,#57612,#57613,#57614,#57615,
#57616,#57617,#57618,#57619,#57620),.UNSPECIFIED.,.F.,.F.,(4,1,1,1,1,1,
1,4),(53.4070751110265,54.1538932847921,55.1431761391379,56.1324589934837,
57.1217418478294,58.1110247021752,59.100307556521,59.6902604182061),
 .UNSPECIFIED.);
#940=B_SPLINE_CURVE_WITH_KNOTS('',3,(#57621,#57622,#57623,#57624,#57625,
#57626,#57627,#57628,#57629,#57630),.UNSPECIFIED.,.F.,.F.,(4,1,1,1,1,1,
1,4),(53.4070751110265,53.8169072514586,54.8061901058043,55.7954729601501,
56.7847558144959,57.7740386688416,58.7633215231874,59.6902604182061),
 .UNSPECIFIED.);
#941=B_SPLINE_CURVE_WITH_KNOTS('',3,(#57635,#57636,#57637,#57638,#57639,
#57640,#57641,#57642,#57643,#57644,#57645),.UNSPECIFIED.,.F.,.F.,(4,1,1,
1,1,1,1,1,4),(47.1238898038469,47.2289133043718,48.2181961587175,49.2074790130633,
50.1967618674091,51.1860447217548,52.1753275761006,53.1646104304464,53.4070751110265),
 .UNSPECIFIED.);
#942=B_SPLINE_CURVE_WITH_KNOTS('',3,(#57646,#57647,#57648,#57649,#57650,
#57651,#57652,#57653,#57654,#57655),.UNSPECIFIED.,.F.,.F.,(4,1,1,1,1,1,
1,4),(47.1238898038469,47.881210125384,48.8704929797298,49.8597758340755,
50.8490586884213,51.8383415427671,52.8276243971128,53.4070751110265),
 .UNSPECIFIED.);
#943=B_SPLINE_CURVE_WITH_KNOTS('',3,(#57660,#57661,#57662,#57663,#57664,
#57665,#57666,#57667,#57668,#57669),.UNSPECIFIED.,.F.,.F.,(4,1,1,1,1,1,
1,4),(40.8407044966673,41.2932161782972,42.2824990326429,43.2717818869887,
44.2610647413345,45.2503475956803,46.239630450026,47.1238898038469),
 .UNSPECIFIED.);
#944=B_SPLINE_CURVE_WITH_KNOTS('',3,(#57670,#57671,#57672,#57673,#57674,
#57675,#57676,#57677,#57678,#57679,#57680),.UNSPECIFIED.,.F.,.F.,(4,1,1,
1,1,1,1,1,4),(40.8407044966673,40.9562301449636,41.9455129993094,42.9347958536552,
43.9240787080009,44.9133615623467,45.9026444166925,46.8919272710382,47.1238898038469),
 .UNSPECIFIED.);
#945=B_SPLINE_CURVE_WITH_KNOTS('',3,(#57685,#57686,#57687,#57688,#57689,
#57690,#57691,#57692,#57693,#57694),.UNSPECIFIED.,.F.,.F.,(4,1,1,1,1,1,
1,4),(34.5575191894877,35.3575190522226,36.3468019065684,37.3360847609141,
38.3253676152599,39.3146504696057,40.3039333239514,40.8407044966673),
 .UNSPECIFIED.);
#946=B_SPLINE_CURVE_WITH_KNOTS('',3,(#57695,#57696,#57697,#57698,#57699,
#57700,#57701,#57702,#57703,#57704),.UNSPECIFIED.,.F.,.F.,(4,1,1,1,1,1,
1,4),(34.5575191894877,35.020533018889,36.0098158732348,36.9990987275806,
37.9883815819263,38.9776644362721,39.9669472906179,40.8407044966673),
 .UNSPECIFIED.);
#947=B_SPLINE_CURVE_WITH_KNOTS('',3,(#57709,#57710,#57711,#57712,#57713,
#57714,#57715,#57716,#57717,#57718,#57719),.UNSPECIFIED.,.F.,.F.,(4,1,1,
1,1,1,1,1,4),(28.2743338823081,28.4325390718022,29.421821926148,30.4111047804938,
31.4003876348395,32.3896704891853,33.3789533435311,34.3682361978768,34.5575191894877),
 .UNSPECIFIED.);
#948=B_SPLINE_CURVE_WITH_KNOTS('',3,(#57720,#57721,#57722,#57723,#57724,
#57725,#57726,#57727,#57728,#57729),.UNSPECIFIED.,.F.,.F.,(4,1,1,1,1,1,
1,4),(28.2743338823081,29.0848358928144,30.0741187471602,31.063401601506,
32.0526844558517,33.0419673101975,34.0312501645433,34.5575191894877),
 .UNSPECIFIED.);
#949=B_SPLINE_CURVE_WITH_KNOTS('',3,(#57734,#57735,#57736,#57737,#57738,
#57739,#57740,#57741,#57742,#57743),.UNSPECIFIED.,.F.,.F.,(4,1,1,1,1,1,
1,4),(21.9911485751285,22.4968419457276,23.4861248000734,24.4754076544192,
25.4646905087649,26.4539733631107,27.4432562174565,28.2743338823081),
 .UNSPECIFIED.);
#950=B_SPLINE_CURVE_WITH_KNOTS('',3,(#57744,#57745,#57746,#57747,#57748,
#57749,#57750,#57751,#57752,#57753,#57754),.UNSPECIFIED.,.F.,.F.,(4,1,1,
1,1,1,1,1,4),(21.9911485751285,22.1598559123941,23.1491387667399,24.1384216210856,
25.1277044754314,26.1169873297771,27.1062701841229,28.0955530384687,28.2743338823081),
 .UNSPECIFIED.);
#951=B_SPLINE_CURVE_WITH_KNOTS('',3,(#57759,#57760,#57761,#57762,#57763,
#57764,#57765,#57766,#57767,#57768),.UNSPECIFIED.,.F.,.F.,(4,1,1,1,1,1,
1,4),(15.7079632679489,16.561144819653,17.5504276739988,18.5397105283446,
19.5289933826903,20.5182762370361,21.5075590913819,21.9911485751285),
 .UNSPECIFIED.);
#952=B_SPLINE_CURVE_WITH_KNOTS('',3,(#57769,#57770,#57771,#57772,#57773,
#57774,#57775,#57776,#57777,#57778),.UNSPECIFIED.,.F.,.F.,(4,1,1,1,1,1,
1,4),(15.7079632679489,16.2241587863195,17.2134416406653,18.202724495011,
19.1920073493568,20.1812902037026,21.1705730580483,21.9911485751285),
 .UNSPECIFIED.);
#953=B_SPLINE_CURVE_WITH_KNOTS('',3,(#57784,#57785,#57786,#57787,#57788,
#57789),.UNSPECIFIED.,.F.,.F.,(4,2,4),(-0.342456092017903,-0.262804961413355,
0.),.UNSPECIFIED.);
#954=B_SPLINE_CURVE_WITH_KNOTS('',3,(#57791,#57792,#57793,#57794,#57795,
#57796,#57797,#57798,#57799,#57800,#57801,#57802),.UNSPECIFIED.,.F.,.F.,
(4,2,2,2,2,4),(0.,0.178010957135692,0.381093675614414,0.596885981784515,
0.750004601526435,0.833159445966906),.UNSPECIFIED.);
#955=B_SPLINE_CURVE_WITH_KNOTS('',3,(#57804,#57805,#57806,#57807,#57808,
#57809,#57810,#57811,#57812,#57813,#57814,#57815,#57816,#57817),
 .UNSPECIFIED.,.F.,.F.,(4,2,2,2,2,2,4),(2.8879030854515,2.90631755511173,
3.01588868292827,3.10104216567944,3.18619564843061,3.29576677624714,3.31418124590738),
 .UNSPECIFIED.);
#956=B_SPLINE_CURVE_WITH_KNOTS('',3,(#57819,#57820,#57821,#57822,#57823,
#57824,#57825,#57826,#57827,#57828,#57829,#57830),.UNSPECIFIED.,.F.,.F.,
(4,2,2,2,2,4),(0.,0.182810359067708,0.452655692105918,0.783610652837132,
0.960006030065839,1.14418486243573),.UNSPECIFIED.);
#957=B_SPLINE_CURVE_WITH_KNOTS('',3,(#57832,#57833,#57834,#57835,#57836,
#57837),.UNSPECIFIED.,.F.,.F.,(4,2,4),(3.5322737051841,3.79507866659746,
3.87472979720201),.UNSPECIFIED.);
#958=B_SPLINE_CURVE_WITH_KNOTS('',3,(#57841,#57842,#57843,#57844,#57845,
#57846),.UNSPECIFIED.,.F.,.F.,(4,2,4),(3.1898176131662,3.26946874377075,
3.5322737051841),.UNSPECIFIED.);
#959=B_SPLINE_CURVE_WITH_KNOTS('',3,(#57848,#57849,#57850,#57851,#57852,
#57853,#57854,#57855,#57856,#57857,#57858,#57859),.UNSPECIFIED.,.F.,.F.,
(4,2,2,2,2,4),(0.,0.178010957135693,0.381093675614418,0.59688598178454,
0.750004601526475,0.833159445966973),.UNSPECIFIED.);
#960=B_SPLINE_CURVE_WITH_KNOTS('',3,(#57861,#57862,#57863,#57864,#57865,
#57866,#57867,#57868,#57869,#57870,#57871,#57872,#57873,#57874),
 .UNSPECIFIED.,.F.,.F.,(4,2,2,2,2,2,4),(0.820541641665208,0.838956111325442,
0.948527239141976,1.03368072189315,1.11883420464432,1.22840533246085,1.24681980212109),
 .UNSPECIFIED.);
#961=B_SPLINE_CURVE_WITH_KNOTS('',3,(#57876,#57877,#57878,#57879,#57880,
#57881,#57882,#57883,#57884,#57885,#57886,#57887),.UNSPECIFIED.,.F.,.F.,
(4,2,2,2,2,4),(0.,0.182810359067185,0.452655692103104,0.783610652831579,
0.960006030058821,1.14418486242717),.UNSPECIFIED.);
#962=B_SPLINE_CURVE_WITH_KNOTS('',3,(#57888,#57889,#57890,#57891,#57892,
#57893),.UNSPECIFIED.,.F.,.F.,(4,2,4),(0.,0.262804961413355,0.342456092017903),
 .UNSPECIFIED.);
#963=B_SPLINE_CURVE_WITH_KNOTS('',3,(#57909,#57910,#57911,#57912,#57913,
#57914,#57915,#57916,#57917,#57918,#57919,#57920,#57921,#57922,#57923,#57924,
#57925,#57926,#57927,#57928,#57929,#57930,#57931,#57932,#57933,#57934,#57935,
#57936,#57937,#57938,#57939,#57940,#57941,#57942,#57943,#57944,#57945,#57946,
#57947,#57948,#57949,#57950,#57951,#57952,#57953,#57954,#57955,#57956,#57957,
#57958,#57959,#57960,#57961,#57962,#57963,#57964,#57965,#57966,#57967,#57968,
#57969,#57970,#57971,#57972,#57973,#57974,#57975),.UNSPECIFIED.,.F.,.F.,
(4,3,3,3,3,3,3,3,3,3,3,3,3,3,3,3,3,3,3,3,3,3,4),(-0.93774096308181,-0.870261948404392,
-0.832251019814623,-0.812039353702878,-0.742348954142412,-0.729339847034109,
-0.705081468871194,-0.634283519265674,-0.572488451018333,-0.549579435213131,
-0.530963570226855,-0.510693382770993,-0.438960472290944,-0.388997500739232,
-0.372134856040166,-0.354858390446,-0.276993114348998,-0.218594157276247,
-0.196204166307054,-0.17703031168743,-0.099567067450566,-0.043397286057993,
0.),.UNSPECIFIED.);
#964=B_SPLINE_CURVE_WITH_KNOTS('',3,(#57977,#57978,#57979,#57980,#57981,
#57982,#57983,#57984,#57985,#57986,#57987,#57988,#57989,#57990,#57991,#57992,
#57993,#57994,#57995,#57996,#57997,#57998,#57999,#58000,#58001,#58002,#58003,
#58004,#58005,#58006,#58007,#58008,#58009,#58010,#58011,#58012,#58013,#58014,
#58015,#58016,#58017,#58018,#58019,#58020,#58021,#58022,#58023,#58024,#58025,
#58026,#58027,#58028,#58029,#58030,#58031,#58032,#58033,#58034,#58035,#58036,
#58037,#58038,#58039,#58040,#58041,#58042,#58043),.UNSPECIFIED.,.F.,.F.,
(4,3,3,3,3,3,3,3,3,3,3,3,3,3,3,3,3,3,3,3,3,3,4),(-0.933975894023158,-0.856824867797122,
-0.821914501343845,-0.791558113020374,-0.71597790947688,-0.694994410329363,
-0.668582197141203,-0.594616471062628,-0.530120471538128,-0.507052841767612,
-0.490181983238915,-0.465624472013627,-0.393047138731511,-0.348092731553511,
-0.32871533726739,-0.312541480427752,-0.242076479471633,-0.190609197809111,
-0.162579557995071,-0.14514061306184,-0.078314656879451,-0.0362073528215457,
0.),.UNSPECIFIED.);
#965=B_SPLINE_CURVE_WITH_KNOTS('',3,(#58356,#58357,#58358,#58359,#58360,
#58361,#58362,#58363,#58364),.UNSPECIFIED.,.F.,.F.,(4,1,1,1,1,1,4),(11.6147305479242,
12.1093719750971,12.60401340227,13.5932962566158,14.5825791109615,15.5718619653073,
15.7079632679489),.UNSPECIFIED.);
#966=B_SPLINE_CURVE_WITH_KNOTS('',3,(#58365,#58366,#58367,#58368,#58369,
#58370,#58371,#58372,#58373,#58374,#58375,#58376,#58377,#58378,#58379,#58380,
#58381,#58382,#58383,#58384,#58385,#58386,#58387,#58388,#58389,#58390,#58391,
#58392,#58393,#58394,#58395,#58396,#58397,#58398,#58399,#58400,#58401,#58402,
#58403,#58404,#58405,#58406,#58407,#58408,#58409,#58410,#58411,#58412,#58413,
#58414,#58415,#58416,#58417,#58418,#58419,#58420,#58421,#58422,#58423,#58424,
#58425,#58426,#58427,#58428,#58429,#58430,#58431),.UNSPECIFIED.,.F.,.F.,
(4,3,3,3,3,3,3,3,3,3,3,3,3,3,3,3,3,3,3,3,3,3,4),(-0.933975894023119,-0.890767895830556,
-0.832649055223636,-0.807165334613026,-0.784870232004528,-0.708420338291616,
-0.684040660118115,-0.663611018024939,-0.589324938941615,-0.542495792243922,
-0.504321658003645,-0.487154884783798,-0.425817170975192,-0.367338377334077,
-0.338840187897342,-0.316929096908672,-0.246728742864094,-0.207915887991521,
-0.16973711093609,-0.149619355722235,-0.0812991141899627,-0.0146711098764389,
0.),.UNSPECIFIED.);
#967=B_SPLINE_CURVE_WITH_KNOTS('',3,(#58432,#58433,#58434,#58435,#58436,
#58437,#58438,#58439,#58440,#58441,#58442,#58443,#58444,#58445,#58446,#58447),
 .UNSPECIFIED.,.F.,.F.,(4,3,3,3,3,4),(-70.2390826585493,-69.7444412313765,
-69.2497998042036,-68.2605169498578,-67.2712340955121,-66.9250857918206),
 .UNSPECIFIED.);
#968=B_SPLINE_CURVE_WITH_KNOTS('',3,(#58450,#58451,#58452,#58453,#58454,
#58455,#58456,#58457,#58458),.UNSPECIFIED.,.F.,.F.,(4,1,1,1,1,1,4),(10.3764180272042,
11.2777445145907,12.2670273689364,13.2563102232822,14.245593077628,15.2348759319737,
15.7079632679489),.UNSPECIFIED.);
#969=B_SPLINE_CURVE_WITH_KNOTS('',3,(#58764,#58765,#58766,#58767,#58768,
#58769,#58770,#58771,#58772,#58773,#58774,#58775,#58776,#58777,#58778,#58779),
 .UNSPECIFIED.,.F.,.F.,(4,3,3,3,3,4),(63.9467350810118,64.3033855324747,
65.2926683868205,66.2819512411663,67.2712340955121,68.1725605828985),
 .UNSPECIFIED.);
#970=B_SPLINE_CURVE_WITH_KNOTS('',3,(#58780,#58781,#58782,#58783,#58784,
#58785,#58786,#58787,#58788,#58789,#58790,#58791,#58792,#58793,#58794,#58795,
#58796,#58797,#58798,#58799,#58800,#58801,#58802,#58803,#58804,#58805,#58806,
#58807,#58808,#58809,#58810,#58811,#58812,#58813,#58814,#58815,#58816,#58817,
#58818,#58819,#58820,#58821,#58822,#58823,#58824,#58825,#58826,#58827,#58828,
#58829,#58830,#58831,#58832,#58833,#58834,#58835,#58836,#58837,#58838,#58839,
#58840,#58841,#58842,#58843),.UNSPECIFIED.,.F.,.F.,(4,3,3,3,3,3,3,3,3,3,
3,3,3,3,3,3,3,3,3,3,3,4),(-0.937740963081774,-0.901429380350922,-0.842615939984195,
-0.815134419970695,-0.763821611298058,-0.734138838750838,-0.715144480290609,
-0.643654231153057,-0.571972635037333,-0.551702893088566,-0.534998195849319,
-0.470725533976372,-0.413107434862205,-0.384514347555702,-0.359013510944126,
-0.284551929400665,-0.240253137519706,-0.200676800014282,-0.176385565585146,
-0.0995853117506865,-0.0229257113100043,0.),.UNSPECIFIED.);
#971=B_SPLINE_CURVE_WITH_KNOTS('',3,(#59083,#59084,#59085,#59086,#59087,
#59088,#59089,#59090,#59091,#59092),.UNSPECIFIED.,.F.,.F.,(4,3,3,4),(-4.0929304201308,
-3.25801350823594,-2.42309659634109,-2.07498647268397),.UNSPECIFIED.);
#972=B_SPLINE_CURVE_WITH_KNOTS('',3,(#59095,#59096,#59097,#59098,#59099,
#59100,#59101,#59102,#59103,#59104),.UNSPECIFIED.,.F.,.F.,(4,3,3,4),(0.,
0.499092211205179,0.998184422410358,1.12364870614423),.UNSPECIFIED.);
#973=B_SPLINE_CURVE_WITH_KNOTS('',3,(#59109,#59110,#59111,#59112,#59113,
#59114,#59115,#59116,#59117,#59118,#59119,#59120,#59121,#59122,#59123,#59124,
#59125,#59126,#59127,#59128,#59129,#59130,#59131,#59132,#59133,#59134,#59135,
#59136,#59137,#59138,#59139),.UNSPECIFIED.,.F.,.F.,(4,3,3,3,3,3,3,3,3,3,
4),(-10.3761157273104,-9.98184422410361,-8.98365980169324,-8.48456759048806,
-7.98547537928288,-6.98729095687252,-6.48819874566734,-5.98910653446216,
-5.49001432325698,-4.9909221120518,-4.0929304201308),.UNSPECIFIED.);
#974=B_SPLINE_CURVE_WITH_KNOTS('',3,(#59140,#59141,#59142,#59143,#59144,
#59145,#59146,#59147,#59148,#59149,#59150,#59151,#59152,#59153,#59154,#59155,
#59156,#59157,#59158,#59159,#59160,#59161,#59162,#59163,#59164,#59165,#59166,
#59167,#59168,#59169,#59170),.UNSPECIFIED.,.F.,.F.,(4,3,3,3,3,3,3,3,3,3,
4),(1.12364870614423,1.49727663361554,1.99636884482072,2.99455326723107,
3.99273768964143,4.99092211205179,5.49001432325697,5.98910653446215,6.48819874566733,
6.98729095687251,7.4068340133238),.UNSPECIFIED.);
#975=B_SPLINE_CURVE_WITH_KNOTS('',3,(#59175,#59176,#59177,#59178,#59179,
#59180,#59181,#59182,#59183,#59184,#59185,#59186,#59187,#59188,#59189,#59190,
#59191,#59192,#59193,#59194,#59195,#59196,#59197,#59198,#59199,#59200,#59201,
#59202,#59203,#59204,#59205),.UNSPECIFIED.,.F.,.F.,(4,3,3,3,3,3,3,3,3,3,
4),(-16.65930103449,-15.9709507585658,-15.4718585473606,-14.9727663361554,
-13.974581913745,-13.4754897025399,-12.9763974913347,-12.4773052801295,
-11.9782130689243,-10.980028646514,-10.3761157273104),.UNSPECIFIED.);
#976=B_SPLINE_CURVE_WITH_KNOTS('',3,(#59206,#59207,#59208,#59209,#59210,
#59211,#59212,#59213,#59214,#59215,#59216,#59217,#59218,#59219,#59220,#59221,
#59222,#59223,#59224,#59225,#59226,#59227,#59228,#59229,#59230),
 .UNSPECIFIED.,.F.,.F.,(4,3,3,3,3,3,3,3,4),(7.4068340133238,8.24175092521866,
9.07666783711352,9.91158474900838,10.7465016609032,11.5814185727981,12.416335484693,
13.2512523965878,13.6900193205034),.UNSPECIFIED.);
#977=B_SPLINE_CURVE_WITH_KNOTS('',3,(#59235,#59236,#59237,#59238,#59239,
#59240,#59241,#59242,#59243,#59244,#59245,#59246,#59247,#59248,#59249,#59250,
#59251,#59252,#59253,#59254,#59255,#59256,#59257,#59258,#59259,#59260,#59261,
#59262,#59263,#59264,#59265),.UNSPECIFIED.,.F.,.F.,(4,3,3,3,3,3,3,3,3,3,
4),(-22.9424863416695,-22.4591495042331,-21.9600572930279,-20.9618728706176,
-20.4627806594124,-19.9636884482072,-19.464596237002,-18.9655040257968,
-17.9673196033865,-16.9691351809761,-16.65930103449),.UNSPECIFIED.);
#978=B_SPLINE_CURVE_WITH_KNOTS('',3,(#59266,#59267,#59268,#59269,#59270,
#59271,#59272,#59273,#59274,#59275,#59276,#59277,#59278,#59279,#59280,#59281,
#59282,#59283,#59284,#59285,#59286,#59287,#59288,#59289,#59290),
 .UNSPECIFIED.,.F.,.F.,(4,3,3,3,3,3,3,3,4),(13.6900193205034,14.5249362323982,
15.3598531442931,16.1947700561879,17.0296869680828,17.8646038799776,18.6995207918725,
19.5344377037673,19.973204627683),.UNSPECIFIED.);
#979=B_SPLINE_CURVE_WITH_KNOTS('',3,(#59295,#59296,#59297,#59298,#59299,
#59300,#59301,#59302,#59303,#59304,#59305,#59306,#59307,#59308,#59309,#59310,
#59311,#59312,#59313,#59314,#59315,#59316,#59317,#59318,#59319,#59320,#59321,
#59322,#59323,#59324,#59325),.UNSPECIFIED.,.F.,.F.,(4,3,3,3,3,3,3,3,3,3,
4),(-29.2256716488491,-28.9473482499005,-27.9491638274901,-27.4500716162849,
-26.9509794050797,-26.4518871938745,-25.9527949826694,-24.954610560259,
-23.9564261378486,-22.9582417154383,-22.9424863416695),.UNSPECIFIED.);
#980=B_SPLINE_CURVE_WITH_KNOTS('',3,(#59326,#59327,#59328,#59329,#59330,
#59331,#59332,#59333,#59334,#59335,#59336,#59337,#59338,#59339,#59340,#59341,
#59342,#59343,#59344,#59345,#59346,#59347,#59348,#59349,#59350,#59351,#59352,
#59353),.UNSPECIFIED.,.F.,.F.,(4,3,3,3,3,3,3,3,3,4),(19.973204627683,20.4627806594124,
20.9618728706176,21.9600572930279,22.4591495042331,22.9582417154383,23.9564261378486,
24.954610560259,25.9527949826694,26.2563899348625),.UNSPECIFIED.);
#981=B_SPLINE_CURVE_WITH_KNOTS('',3,(#59358,#59359,#59360,#59361,#59362,
#59363,#59364,#59365,#59366,#59367,#59368,#59369,#59370,#59371,#59372,#59373,
#59374,#59375,#59376,#59377,#59378,#59379,#59380,#59381,#59382),
 .UNSPECIFIED.,.F.,.F.,(4,3,3,3,3,3,3,3,4),(-35.5088569560287,-34.6739400441339,
-33.839023132239,-33.0041062203442,-32.1691893084493,-31.3342723965544,
-30.4993554846596,-29.6644385727647,-29.2256716488491),.UNSPECIFIED.);
#982=B_SPLINE_CURVE_WITH_KNOTS('',3,(#59383,#59384,#59385,#59386,#59387,
#59388,#59389,#59390,#59391,#59392,#59393,#59394,#59395,#59396,#59397,#59398,
#59399,#59400,#59401,#59402,#59403,#59404,#59405,#59406,#59407,#59408,#59409,
#59410,#59411,#59412,#59413),.UNSPECIFIED.,.F.,.F.,(4,3,3,3,3,3,3,3,3,3,
4),(26.2563899348625,26.4518871938745,26.9509794050797,27.4500716162849,
27.9491638274901,28.9473482499005,29.4464404611057,29.9455326723108,30.9437170947212,
31.9419015171316,32.5395752420422),.UNSPECIFIED.);
#983=B_SPLINE_CURVE_WITH_KNOTS('',3,(#59418,#59419,#59420,#59421,#59422,
#59423,#59424,#59425,#59426,#59427,#59428,#59429,#59430,#59431,#59432,#59433,
#59434,#59435,#59436,#59437,#59438,#59439,#59440,#59441,#59442),
 .UNSPECIFIED.,.F.,.F.,(4,3,3,3,3,3,3,3,4),(-41.7920422632083,-40.9571253513134,
-40.1222084394186,-39.2872915275237,-38.4523746156289,-37.617457703734,
-36.7825407918392,-35.9476238799443,-35.5088569560287),.UNSPECIFIED.);
#984=B_SPLINE_CURVE_WITH_KNOTS('',3,(#59443,#59444,#59445,#59446,#59447,
#59448,#59449,#59450,#59451,#59452,#59453,#59454,#59455,#59456,#59457,#59458,
#59459,#59460,#59461,#59462,#59463,#59464,#59465,#59466,#59467,#59468,#59469,
#59470,#59471,#59472,#59473),.UNSPECIFIED.,.F.,.F.,(4,3,3,3,3,3,3,3,3,3,
4),(32.5395752420422,32.940085939542,33.4391781507471,33.9382703619523,
34.4373625731575,34.9364547843627,35.934639206773,36.4337314179782,36.9328236291834,
37.9310080515937,38.8227605492217),.UNSPECIFIED.);
#985=B_SPLINE_CURVE_WITH_KNOTS('',3,(#59478,#59479,#59480,#59481,#59482,
#59483,#59484,#59485,#59486,#59487,#59488,#59489,#59490,#59491,#59492,#59493,
#59494,#59495,#59496,#59497,#59498,#59499,#59500,#59501,#59502),
 .UNSPECIFIED.,.F.,.F.,(4,3,3,3,3,3,3,3,4),(-48.0752275703879,-47.240310658493,
-46.4053937465982,-45.5704768347033,-44.7355599228084,-43.9006430109136,
-43.0657260990187,-42.2308091871238,-41.7920422632083),.UNSPECIFIED.);
#986=B_SPLINE_CURVE_WITH_KNOTS('',3,(#59503,#59504,#59505,#59506,#59507,
#59508,#59509,#59510,#59511,#59512,#59513,#59514,#59515,#59516,#59517,#59518,
#59519,#59520,#59521,#59522,#59523,#59524,#59525,#59526,#59527,#59528,#59529,
#59530,#59531,#59532,#59533,#59534,#59535,#59536),.UNSPECIFIED.,.F.,.F.,
(4,3,3,3,3,3,3,3,3,3,3,4),(38.8227605492217,38.929192474004,39.9273768964144,
40.4264691076196,40.9255613188247,41.4246535300299,41.9237457412351,42.9219301636455,
43.4210223748506,43.9201145860558,44.9182990084662,45.1059458564013),
 .UNSPECIFIED.);
#987=B_SPLINE_CURVE_WITH_KNOTS('',3,(#59541,#59542,#59543,#59544,#59545,
#59546,#59547,#59548,#59549,#59550,#59551,#59552,#59553,#59554,#59555,#59556,
#59557,#59558,#59559,#59560,#59561,#59562,#59563,#59564,#59565),
 .UNSPECIFIED.,.F.,.F.,(4,3,3,3,3,3,3,3,4),(-54.3584128775675,-53.5234959656726,
-52.6885790537778,-51.8536621418829,-51.018745229988,-50.1838283180932,
-49.3489114061983,-48.5139944943034,-48.0752275703879),.UNSPECIFIED.);
#988=B_SPLINE_CURVE_WITH_KNOTS('',3,(#59566,#59567,#59568,#59569,#59570,
#59571,#59572,#59573,#59574,#59575,#59576,#59577,#59578,#59579,#59580,#59581,
#59582,#59583,#59584,#59585,#59586,#59587,#59588,#59589,#59590,#59591,#59592,
#59593,#59594,#59595,#59596),.UNSPECIFIED.,.F.,.F.,(4,3,3,3,3,3,3,3,3,3,
4),(45.1059458564013,45.9164834308765,46.9146678532869,47.4137600644921,
47.9128522756973,48.4119444869025,48.9110366981077,49.909221120518,50.4083133317232,
50.9074055429284,51.3891311635809),.UNSPECIFIED.);
#989=B_SPLINE_CURVE_WITH_KNOTS('',3,(#59601,#59602,#59603,#59604,#59605,
#59606,#59607,#59608,#59609,#59610,#59611,#59612,#59613,#59614,#59615,#59616,
#59617,#59618,#59619,#59620,#59621,#59622,#59623,#59624,#59625,#59626,#59627,
#59628,#59629,#59630,#59631),.UNSPECIFIED.,.F.,.F.,(4,3,3,3,3,3,3,3,3,3,
4),(-60.6415981847471,-59.8910653446216,-58.8928809222113,-57.8946964998009,
-57.3956042885957,-56.8965120773905,-55.8983276549802,-55.399235443775,
-54.9001432325698,-54.4010510213646,-54.3584128775675),.UNSPECIFIED.);
#990=B_SPLINE_CURVE_WITH_KNOTS('',3,(#59632,#59633,#59634,#59635,#59636,
#59637,#59638,#59639,#59640,#59641,#59642,#59643,#59644,#59645,#59646,#59647,
#59648,#59649,#59650,#59651,#59652,#59653,#59654,#59655,#59656,#59657,#59658,
#59659,#59660,#59661,#59662),.UNSPECIFIED.,.F.,.F.,(4,3,3,3,3,3,3,3,3,3,
4),(51.3891311635809,51.9055899653388,52.9037743877492,53.9019588101595,
54.4010510213647,54.9001432325699,55.3992354437751,55.8983276549802,56.8965120773906,
57.3956042885958,57.6723164707605),.UNSPECIFIED.);
#991=B_SPLINE_CURVE_WITH_KNOTS('',3,(#59667,#59668,#59669,#59670,#59671,
#59672,#59673,#59674,#59675,#59676,#59677,#59678,#59679,#59680,#59681,#59682,
#59683,#59684,#59685,#59686,#59687,#59688,#59689,#59690,#59691,#59692,#59693,
#59694,#59695,#59696,#59697,#59698,#59699,#59700),.UNSPECIFIED.,.F.,.F.,
(4,3,3,3,3,3,3,3,3,3,3,4),(-66.9247834919267,-66.8783563014941,-65.8801718790838,
-64.8819874566734,-64.3828952454682,-63.8838030342631,-62.8856186118527,
-62.3865264006475,-61.8874341894423,-61.3883419782372,-60.889249767032,
-60.6415981847471),.UNSPECIFIED.);
#992=B_SPLINE_CURVE_WITH_KNOTS('',3,(#59701,#59702,#59703,#59704,#59705,
#59706,#59707,#59708,#59709,#59710,#59711,#59712,#59713,#59714,#59715,#59716,
#59717,#59718,#59719,#59720,#59721,#59722,#59723,#59724,#59725,#59726,#59727,
#59728,#59729,#59730,#59731),.UNSPECIFIED.,.F.,.F.,(4,3,3,3,3,3,3,3,3,3,
4),(57.6723164707605,57.894696499801,58.8928809222113,59.8910653446217,
60.8892497670321,61.3883419782372,61.8874341894424,62.3865264006476,62.8856186118528,
63.8838030342631,63.9555017779401),.UNSPECIFIED.);
#993=B_SPLINE_CURVE_WITH_KNOTS('',3,(#59736,#59737,#59738,#59739,#59740,
#59741,#59742,#59743,#59744,#59745,#59746,#59747,#59748,#59749,#59750,#59751,
#59752,#59753,#59754,#59755,#59756,#59757,#59758,#59759,#59760,#59761,#59762,
#59763,#59764,#59765,#59766),.UNSPECIFIED.,.F.,.F.,(4,3,3,3,3,3,3,3,3,3,
4),(-73.2079687991063,-72.8674628359563,-71.869278413546,-71.3701862023408,
-70.8710939911356,-69.8729095687252,-69.37381735752,-68.8747251463149,-68.3756329351097,
-67.8765407239045,-66.9247834919267),.UNSPECIFIED.);
#994=B_SPLINE_CURVE_WITH_KNOTS('',3,(#59767,#59768,#59769,#59770,#59771,
#59772,#59773,#59774,#59775,#59776,#59777,#59778,#59779,#59780,#59781,#59782,
#59783,#59784,#59785,#59786,#59787,#59788,#59789,#59790,#59791,#59792,#59793,
#59794,#59795,#59796,#59797),.UNSPECIFIED.,.F.,.F.,(4,3,3,3,3,3,3,3,3,3,
4),(63.9555017779401,64.3828952454683,64.8819874566735,65.8801718790838,
66.8783563014942,67.8765407239045,68.3756329351097,68.8747251463149,69.37381735752,
69.8729095687252,70.2386870851197),.UNSPECIFIED.);
#995=B_SPLINE_CURVE_WITH_KNOTS('',3,(#59802,#59803,#59804,#59805,#59806,
#59807,#59808,#59809,#59810,#59811,#59812,#59813,#59814,#59815,#59816,#59817,
#59818,#59819,#59820,#59821,#59822,#59823,#59824,#59825,#59826,#59827,#59828,
#59829,#59830,#59831,#59832),.UNSPECIFIED.,.F.,.F.,(4,3,3,3,3,3,3,3,3,3,
4),(-79.4911541062859,-78.8565693704185,-78.3574771592133,-77.8583849480081,
-76.8602005255977,-76.3611083143926,-75.8620161031874,-75.3629238919822,
-74.863831680777,-73.8656472583666,-73.2079687991063),.UNSPECIFIED.);
#996=B_SPLINE_CURVE_WITH_KNOTS('',3,(#59833,#59834,#59835,#59836,#59837,
#59838,#59839,#59840,#59841,#59842,#59843,#59844,#59845,#59846,#59847,#59848,
#59849,#59850,#59851,#59852,#59853,#59854,#59855,#59856,#59857),
 .UNSPECIFIED.,.F.,.F.,(4,3,3,3,3,3,3,3,4),(70.2386870851197,71.0736039970146,
71.9085209089095,72.7434378208043,73.5783547326992,74.413271644594,75.2481885564889,
76.0831054683838,76.5218723922993),.UNSPECIFIED.);
#997=B_SPLINE_CURVE_WITH_KNOTS('',3,(#59862,#59863,#59864,#59865,#59866,
#59867,#59868,#59869,#59870,#59871,#59872,#59873,#59874,#59875,#59876,#59877,
#59878,#59879,#59880,#59881,#59882,#59883,#59884,#59885,#59886,#59887,#59888,
#59889,#59890,#59891,#59892),.UNSPECIFIED.,.F.,.F.,(4,3,3,3,3,3,3,3,3,3,
4),(-85.7743394134655,-85.3447681160858,-84.8456759048806,-83.8474914824703,
-83.3483992712651,-82.8493070600599,-82.3502148488547,-81.8511226376495,
-80.8529382152392,-79.8547537928288,-79.4911541062859),.UNSPECIFIED.);
#998=B_SPLINE_CURVE_WITH_KNOTS('',3,(#59893,#59894,#59895,#59896,#59897,
#59898,#59899,#59900,#59901,#59902,#59903,#59904,#59905,#59906,#59907,#59908,
#59909,#59910,#59911,#59912,#59913,#59914,#59915,#59916,#59917,#59918,#59919,
#59920),.UNSPECIFIED.,.F.,.F.,(4,3,3,3,3,3,3,3,3,4),(76.5218723922993,76.8602005255978,
77.8583849480082,78.3574771592134,78.8565693704185,79.8547537928289,80.8529382152392,
81.8511226376496,82.3502148488548,82.8050576994789),.UNSPECIFIED.);
#999=B_SPLINE_CURVE_WITH_KNOTS('',3,(#59925,#59926,#59927,#59928,#59929,
#59930,#59931,#59932,#59933,#59934,#59935,#59936,#59937,#59938,#59939,#59940,
#59941,#59942,#59943,#59944,#59945,#59946,#59947,#59948,#59949,#59950,#59951,
#59952,#59953,#59954,#59955),.UNSPECIFIED.,.F.,.F.,(4,3,3,3,3,3,3,3,3,3,
4),(-92.057524720645,-91.8329668617531,-90.8347824393428,-90.3356902281376,
-89.8365980169324,-89.3375058057272,-88.8384135945221,-87.8402291721117,
-86.8420447497013,-85.843860327291,-85.7743394134655),.UNSPECIFIED.);
#1000=B_SPLINE_CURVE_WITH_KNOTS('',3,(#59956,#59957,#59958,#59959,#59960,
#59961,#59962,#59963,#59964,#59965,#59966,#59967,#59968,#59969,#59970,#59971,
#59972,#59973,#59974,#59975,#59976,#59977,#59978,#59979,#59980,#59981,#59982,
#59983,#59984,#59985,#59986),.UNSPECIFIED.,.F.,.F.,(4,3,3,3,3,3,3,3,3,3,
4),(82.8050576994789,82.84930706006,83.3483992712651,83.8474914824703,84.8456759048807,
85.3447681160858,85.843860327291,86.8420447497014,87.8402291721117,88.8384135945221,
89.0882430066585),.UNSPECIFIED.);
#1001=B_SPLINE_CURVE_WITH_KNOTS('',3,(#59991,#59992,#59993,#59994,#59995,
#59996,#59997,#59998,#59999,#60000,#60001,#60002,#60003,#60004,#60005,#60006,
#60007,#60008,#60009,#60010,#60011,#60012,#60013,#60014,#60015),
 .UNSPECIFIED.,.F.,.F.,(4,3,3,3,3,3,3,3,4),(-98.3407100278246,-97.5057931159298,
-96.6708762040349,-95.8359592921401,-95.0010423802452,-94.1661254683504,
-93.3312085564555,-92.4962916445607,-92.057524720645),.UNSPECIFIED.);
#1002=B_SPLINE_CURVE_WITH_KNOTS('',3,(#60016,#60017,#60018,#60019,#60020,
#60021,#60022,#60023,#60024,#60025,#60026,#60027,#60028,#60029,#60030,#60031,
#60032,#60033,#60034,#60035,#60036,#60037,#60038,#60039,#60040,#60041,#60042,
#60043,#60044,#60045,#60046),.UNSPECIFIED.,.F.,.F.,(4,3,3,3,3,3,3,3,3,3,
4),(89.0882430066585,89.3375058057273,89.8365980169325,90.3356902281376,
90.8347824393428,91.8329668617532,92.3320590729584,92.8311512841636,93.8293357065739,
94.8275201289843,95.3714283138381),.UNSPECIFIED.);
#1003=B_SPLINE_CURVE_WITH_KNOTS('',3,(#60051,#60052,#60053,#60054,#60055,
#60056,#60057,#60058,#60059,#60060,#60061,#60062,#60063,#60064,#60065,#60066,
#60067,#60068,#60069,#60070,#60071,#60072,#60073,#60074,#60075),
 .UNSPECIFIED.,.F.,.F.,(4,3,3,3,3,3,3,3,4),(-104.623895335004,-103.788978423109,
-102.954061511215,-102.11914459932,-101.284227687425,-100.44931077553,-99.6143938636351,
-98.7794769517402,-98.3407100278246),.UNSPECIFIED.);
#1004=B_SPLINE_CURVE_WITH_KNOTS('',3,(#60076,#60077,#60078,#60079,#60080,
#60081,#60082,#60083,#60084,#60085,#60086,#60087,#60088,#60089,#60090,#60091,
#60092,#60093,#60094,#60095,#60096,#60097,#60098,#60099,#60100),
 .UNSPECIFIED.,.F.,.F.,(4,3,3,3,3,3,3,3,4),(95.3714283138381,96.206345225733,
97.0412621376278,97.8761790495227,98.7110959614176,99.5460128733125,100.380929785207,
101.215846697102,101.654613621018),.UNSPECIFIED.);
#1005=B_SPLINE_CURVE_WITH_KNOTS('',3,(#60105,#60106,#60107,#60108,#60109,
#60110,#60111,#60112,#60113,#60114,#60115,#60116,#60117,#60118,#60119,#60120,
#60121,#60122,#60123,#60124,#60125,#60126,#60127,#60128,#60129),
 .UNSPECIFIED.,.F.,.F.,(4,3,3,3,3,3,3,3,4),(-110.907080642184,-110.072163730289,
-109.237246818394,-108.402329906499,-107.567412994604,-106.73249608271,
-105.897579170815,-105.06266225892,-104.623895335004),.UNSPECIFIED.);
#1006=B_SPLINE_CURVE_WITH_KNOTS('',3,(#60130,#60131,#60132,#60133,#60134,
#60135,#60136,#60137,#60138,#60139,#60140,#60141,#60142,#60143,#60144,#60145,
#60146,#60147,#60148,#60149,#60150,#60151,#60152,#60153,#60154),
 .UNSPECIFIED.,.F.,.F.,(4,3,3,3,3,3,3,3,4),(101.654613621018,102.489530532913,
103.324447444807,104.159364356702,104.994281268597,105.829198180492,106.664115092387,
107.499032004282,107.937798928197),.UNSPECIFIED.);
#1007=B_SPLINE_CURVE_WITH_KNOTS('',3,(#60159,#60160,#60161,#60162,#60163,
#60164,#60165,#60166,#60167,#60168,#60169,#60170,#60171,#60172,#60173,#60174,
#60175,#60176,#60177,#60178,#60179,#60180,#60181,#60182,#60183),
 .UNSPECIFIED.,.F.,.F.,(4,3,3,3,3,3,3,3,4),(-117.190265949363,-116.355349037469,
-115.520432125574,-114.685515213679,-113.850598301784,-113.015681389889,
-112.180764477994,-111.345847566099,-110.907080642184),.UNSPECIFIED.);
#1008=B_SPLINE_CURVE_WITH_KNOTS('',3,(#60184,#60185,#60186,#60187,#60188,
#60189,#60190,#60191,#60192,#60193,#60194,#60195,#60196,#60197,#60198,#60199,
#60200,#60201,#60202,#60203,#60204,#60205,#60206,#60207,#60208,#60209,#60210,
#60211,#60212,#60213,#60214),.UNSPECIFIED.,.F.,.F.,(4,3,3,3,3,3,3,3,3,3,
4),(107.937798928197,108.802102042729,109.80028646514,110.299378676345,
110.79847088755,111.297563098755,111.79665530996,112.794839732371,113.293931943576,
113.793024154781,114.220984235377),.UNSPECIFIED.);
#1009=B_SPLINE_CURVE_WITH_KNOTS('',3,(#60219,#60220,#60221,#60222,#60223,
#60224,#60225,#60226,#60227,#60228,#60229,#60230,#60231,#60232,#60233,#60234,
#60235,#60236,#60237,#60238,#60239,#60240,#60241,#60242,#60243,#60244,#60245,
#60246,#60247,#60248,#60249),.UNSPECIFIED.,.F.,.F.,(4,3,3,3,3,3,3,3,3,3,
4),(-123.473451256543,-122.776683956474,-121.778499534064,-120.780315111654,
-120.281222900448,-119.782130689243,-118.783946266833,-118.284854055628,
-117.785761844422,-117.286669633217,-117.190265949363),.UNSPECIFIED.);
#1010=B_SPLINE_CURVE_WITH_KNOTS('',3,(#60250,#60251,#60252,#60253,#60254,
#60255,#60256,#60257,#60258,#60259,#60260,#60261,#60262,#60263,#60264,#60265,
#60266,#60267,#60268,#60269,#60270,#60271,#60272,#60273,#60274,#60275,#60276,
#60277,#60278,#60279,#60280),.UNSPECIFIED.,.F.,.F.,(4,3,3,3,3,3,3,3,3,3,
4),(114.220984235377,114.791208577191,115.789392999602,116.787577422012,
117.286669633217,117.785761844423,118.284854055628,118.783946266833,119.782130689243,
120.281222900448,120.504169542556),.UNSPECIFIED.);
#1011=B_SPLINE_CURVE_WITH_KNOTS('',3,(#60285,#60286,#60287,#60288,#60289,
#60290,#60291,#60292,#60293,#60294,#60295,#60296,#60297,#60298,#60299,#60300,
#60301,#60302,#60303,#60304,#60305,#60306,#60307,#60308,#60309,#60310,#60311,
#60312,#60313,#60314,#60315),.UNSPECIFIED.,.F.,.F.,(4,3,3,3,3,3,3,3,3,3,
4),(-129.756636563723,-128.765790490936,-127.767606068526,-127.268513857321,
-126.769421646116,-125.771237223705,-125.2721450125,-124.773052801295,-124.27396059009,
-123.774868378885,-123.473451256543),.UNSPECIFIED.);
#1012=B_SPLINE_CURVE_WITH_KNOTS('',3,(#60316,#60317,#60318,#60319,#60320,
#60321,#60322,#60323,#60324,#60325,#60326,#60327,#60328,#60329,#60330,#60331,
#60332,#60333,#60334,#60335,#60336,#60337,#60338,#60339,#60340,#60341,#60342,
#60343,#60344,#60345,#60346),.UNSPECIFIED.,.F.,.F.,(4,3,3,3,3,3,3,3,3,3,
4),(120.504169542556,120.780315111654,121.778499534064,122.776683956474,
123.774868378885,124.27396059009,124.773052801295,125.2721450125,125.771237223705,
126.769421646116,126.787354849736),.UNSPECIFIED.);
#1013=B_SPLINE_CURVE_WITH_KNOTS('',3,(#60351,#60352,#60353,#60354,#60355,
#60356,#60357,#60358,#60359,#60360,#60361,#60362,#60363,#60364,#60365,#60366,
#60367,#60368,#60369,#60370,#60371,#60372,#60373,#60374,#60375,#60376,#60377,
#60378,#60379,#60380,#60381,#60382,#60383,#60384),.UNSPECIFIED.,.F.,.F.,
(4,3,3,3,3,3,3,3,3,3,3,4),(-136.039821870902,-135.753081447809,-134.754897025399,
-134.255804814193,-133.756712602988,-132.758528180578,-132.259435969373,
-131.760343758168,-131.261251546962,-130.762159335757,-129.763974913347,
-129.756636563723),.UNSPECIFIED.);
#1014=B_SPLINE_CURVE_WITH_KNOTS('',3,(#60385,#60386,#60387,#60388,#60389,
#60390,#60391,#60392,#60393,#60394,#60395,#60396,#60397,#60398,#60399,#60400,
#60401,#60402,#60403,#60404,#60405,#60406,#60407,#60408,#60409,#60410,#60411,
#60412,#60413,#60414,#60415),.UNSPECIFIED.,.F.,.F.,(4,3,3,3,3,3,3,3,3,3,
4),(126.787354849736,127.268513857321,127.767606068526,128.765790490936,
129.763974913347,130.762159335757,131.261251546962,131.760343758168,132.259435969373,
132.758528180578,133.070540156916),.UNSPECIFIED.);
#1015=B_SPLINE_CURVE_WITH_KNOTS('',3,(#60420,#60421,#60422,#60423,#60424,
#60425,#60426,#60427,#60428,#60429,#60430,#60431,#60432,#60433,#60434,#60435,
#60436,#60437,#60438,#60439,#60440,#60441,#60442,#60443,#60444,#60445,#60446,
#60447,#60448,#60449,#60450),.UNSPECIFIED.,.F.,.F.,(4,3,3,3,3,3,3,3,3,3,
4),(-142.323007178082,-141.742187982271,-141.243095771066,-140.744003559861,
-139.74581913745,-139.246726926245,-138.74763471504,-138.248542503835,-137.74945029263,
-136.751265870219,-136.039821870902),.UNSPECIFIED.);
#1016=B_SPLINE_CURVE_WITH_KNOTS('',3,(#60451,#60452,#60453,#60454,#60455,
#60456,#60457,#60458,#60459,#60460,#60461,#60462,#60463,#60464,#60465,#60466,
#60467,#60468,#60469,#60470,#60471,#60472,#60473,#60474,#60475),
 .UNSPECIFIED.,.F.,.F.,(4,3,3,3,3,3,3,3,4),(133.070540156916,133.905457068811,
134.740373980705,135.5752908926,136.410207804495,137.24512471639,138.080041628285,
138.91495854018,139.353725464095),.UNSPECIFIED.);
#1017=B_SPLINE_CURVE_WITH_KNOTS('',3,(#60480,#60481,#60482,#60483,#60484,
#60485,#60486,#60487,#60488,#60489,#60490,#60491,#60492,#60493,#60494,#60495,
#60496,#60497,#60498,#60499,#60500,#60501,#60502,#60503,#60504,#60505,#60506,
#60507,#60508,#60509,#60510),.UNSPECIFIED.,.F.,.F.,(4,3,3,3,3,3,3,3,3,3,
4),(-148.606192485261,-148.230386727938,-147.731294516733,-146.733110094323,
-146.234017883118,-145.734925671913,-145.235833460707,-144.736741249502,
-143.738556827092,-142.740372404682,-142.323007178082),.UNSPECIFIED.);
#1018=B_SPLINE_CURVE_WITH_KNOTS('',3,(#60511,#60512,#60513,#60514,#60515,
#60516,#60517,#60518,#60519,#60520,#60521,#60522,#60523,#60524,#60525,#60526,
#60527,#60528,#60529,#60530,#60531,#60532,#60533,#60534,#60535,#60536,#60537,
#60538),.UNSPECIFIED.,.F.,.F.,(4,3,3,3,3,3,3,3,3,4),(139.353725464095,139.74581913745,
140.744003559861,141.243095771066,141.742187982271,142.740372404682,143.738556827092,
144.736741249502,145.235833460707,145.636910771275),.UNSPECIFIED.);
#1019=B_SPLINE_CURVE_WITH_KNOTS('',3,(#60543,#60544,#60545,#60546,#60547,
#60548,#60549,#60550,#60551,#60552,#60553,#60554,#60555,#60556,#60557,#60558,
#60559,#60560,#60561,#60562,#60563,#60564,#60565,#60566,#60567,#60568,#60569,
#60570,#60571,#60572,#60573),.UNSPECIFIED.,.F.,.F.,(4,3,3,3,3,3,3,3,3,3,
4),(-154.889377792441,-154.718585473606,-153.720401051195,-153.22130883999,
-152.722216628785,-152.22312441758,-151.724032206375,-150.725847783964,
-149.727663361554,-148.729478939144,-148.606192485261),.UNSPECIFIED.);
#1020=B_SPLINE_CURVE_WITH_KNOTS('',3,(#60574,#60575,#60576,#60577,#60578,
#60579,#60580,#60581,#60582,#60583,#60584,#60585,#60586,#60587,#60588,#60589,
#60590,#60591,#60592,#60593,#60594,#60595,#60596,#60597,#60598,#60599,#60600,
#60601,#60602,#60603,#60604),.UNSPECIFIED.,.F.,.F.,(4,3,3,3,3,3,3,3,3,3,
4),(145.636910771275,145.734925671913,146.234017883118,146.733110094323,
147.731294516733,148.230386727939,148.729478939144,149.727663361554,150.725847783964,
151.724032206375,151.920096078454),.UNSPECIFIED.);
#1021=B_SPLINE_CURVE_WITH_KNOTS('',3,(#60609,#60610,#60611,#60612,#60613,
#60614,#60615,#60616,#60617,#60618,#60619,#60620,#60621,#60622,#60623,#60624,
#60625,#60626,#60627,#60628,#60629,#60630,#60631,#60632,#60633,#60634,#60635,
#60636,#60637,#60638,#60639),.UNSPECIFIED.,.F.,.F.,(4,3,3,3,3,3,3,3,3,3,
4),(-161.17256309962,-160.707692008068,-160.208599796863,-159.709507585658,
-159.210415374452,-158.711323163247,-157.713138740837,-156.714954318427,
-155.716769896016,-155.217677684811,-154.889377792441),.UNSPECIFIED.);
#1022=B_SPLINE_CURVE_WITH_KNOTS('',3,(#60640,#60641,#60642,#60643,#60644,
#60645,#60646,#60647,#60648,#60649,#60650,#60651,#60652,#60653,#60654,#60655,
#60656,#60657,#60658,#60659,#60660,#60661,#60662,#60663,#60664,#60665,#60666,
#60667,#60668,#60669,#60670),.UNSPECIFIED.,.F.,.F.,(4,3,3,3,3,3,3,3,3,3,
4),(151.920096078454,152.22312441758,152.722216628785,153.22130883999,153.720401051196,
154.718585473606,155.217677684811,155.716769896016,156.714954318427,157.713138740837,
158.203281385634),.UNSPECIFIED.);
#1023=B_SPLINE_CURVE_WITH_KNOTS('',3,(#60675,#60676,#60677,#60678,#60679,
#60680,#60681,#60682,#60683,#60684,#60685,#60686,#60687,#60688,#60689,#60690,
#60691,#60692,#60693,#60694,#60695,#60696,#60697,#60698,#60699),
 .UNSPECIFIED.,.F.,.F.,(4,3,3,3,3,3,3,3,4),(-167.4557484068,-166.620831494905,
-165.78591458301,-164.950997671115,-164.116080759221,-163.281163847326,
-162.446246935431,-161.611330023536,-161.17256309962),.UNSPECIFIED.);
#1024=B_SPLINE_CURVE_WITH_KNOTS('',3,(#60700,#60701,#60702,#60703,#60704,
#60705,#60706,#60707,#60708,#60709,#60710,#60711,#60712,#60713,#60714,#60715,
#60716,#60717,#60718,#60719,#60720,#60721,#60722,#60723,#60724),
 .UNSPECIFIED.,.F.,.F.,(4,3,3,3,3,3,3,3,4),(158.203281385634,159.038198297529,
159.873115209424,160.708032121319,161.542949033213,162.377865945108,163.212782857003,
164.047699768898,164.486466692813),.UNSPECIFIED.);
#1025=B_SPLINE_CURVE_WITH_KNOTS('',3,(#60729,#60730,#60731,#60732,#60733,
#60734,#60735,#60736,#60737,#60738,#60739,#60740,#60741,#60742,#60743,#60744,
#60745,#60746,#60747,#60748,#60749,#60750,#60751,#60752,#60753),
 .UNSPECIFIED.,.F.,.F.,(4,3,3,3,3,3,3,3,4),(-173.73893371398,-172.904016802085,
-172.06909989019,-171.234182978295,-170.3992660664,-169.564349154505,-168.72943224261,
-167.894515330716,-167.4557484068),.UNSPECIFIED.);
#1026=B_SPLINE_CURVE_WITH_KNOTS('',3,(#60754,#60755,#60756,#60757,#60758,
#60759,#60760,#60761,#60762,#60763,#60764,#60765,#60766,#60767,#60768,#60769,
#60770,#60771,#60772,#60773,#60774,#60775,#60776,#60777,#60778),
 .UNSPECIFIED.,.F.,.F.,(4,3,3,3,3,3,3,3,4),(164.486466692813,165.321383604708,
166.156300516603,166.991217428498,167.826134340393,168.661051252288,169.495968164183,
170.330885076077,170.769651999993),.UNSPECIFIED.);
#1027=B_SPLINE_CURVE_WITH_KNOTS('',3,(#60783,#60784,#60785,#60786,#60787,
#60788,#60789,#60790,#60791,#60792,#60793,#60794,#60795,#60796,#60797,#60798,
#60799,#60800,#60801,#60802,#60803,#60804,#60805,#60806,#60807,#60808,#60809,
#60810),.UNSPECIFIED.,.F.,.F.,(4,3,3,3,3,3,3,3,3,4),(-180.022119021159,
-179.673196033865,-178.675011611454,-177.676827189044,-176.678642766634,
-176.179550555429,-175.680458344223,-174.682273921813,-174.183181710608,
-173.73893371398),.UNSPECIFIED.);
#1028=B_SPLINE_CURVE_WITH_KNOTS('',3,(#60811,#60812,#60813,#60814,#60815,
#60816,#60817,#60818,#60819,#60820,#60821,#60822,#60823,#60824,#60825,#60826,
#60827,#60828,#60829,#60830,#60831,#60832,#60833,#60834,#60835,#60836,#60837,
#60838,#60839,#60840,#60841),.UNSPECIFIED.,.F.,.F.,(4,3,3,3,3,3,3,3,3,3,
4),(170.769651999993,171.687720654582,172.685905076992,173.184997288198,
173.684089499403,174.183181710608,174.682273921813,175.680458344223,176.179550555429,
176.678642766634,177.052837307173),.UNSPECIFIED.);
#1029=B_SPLINE_CURVE_WITH_KNOTS('',3,(#60846,#60847,#60848,#60849,#60850,
#60851,#60852,#60853,#60854,#60855,#60856,#60857,#60858,#60859,#60860,#60861,
#60862,#60863,#60864,#60865,#60866,#60867,#60868,#60869,#60870,#60871,#60872,
#60873,#60874,#60875,#60876),.UNSPECIFIED.,.F.,.F.,(4,3,3,3,3,3,3,3,3,3,
4),(-186.305304328339,-185.662302568327,-184.664118145917,-183.665933723506,
-183.166841512301,-182.667749301096,-181.669564878686,-181.17047266748,
-180.671380456275,-180.17228824507,-180.022119021159),.UNSPECIFIED.);
#1030=B_SPLINE_CURVE_WITH_KNOTS('',3,(#60877,#60878,#60879,#60880,#60881,
#60882,#60883,#60884,#60885,#60886,#60887,#60888,#60889,#60890,#60891,#60892,
#60893,#60894,#60895,#60896,#60897,#60898,#60899,#60900,#60901,#60902,#60903,
#60904,#60905,#60906,#60907),.UNSPECIFIED.,.F.,.F.,(4,3,3,3,3,3,3,3,3,3,
4),(177.052837307173,177.676827189044,178.675011611455,179.673196033865,
180.17228824507,180.671380456275,181.17047266748,181.669564878686,182.667749301096,
183.166841512301,183.336022614352),.UNSPECIFIED.);
#1031=B_SPLINE_CURVE_WITH_KNOTS('',3,(#60912,#60913,#60914,#60915,#60916,
#60917,#60918,#60919,#60920,#60921,#60922,#60923,#60924,#60925,#60926,#60927,
#60928,#60929,#60930,#60931,#60932,#60933,#60934,#60935,#60936),
 .UNSPECIFIED.,.F.,.F.,(4,3,3,3,3,3,3,3,4),(-192.588489635518,-191.753572723623,
-190.918655811729,-190.083738899834,-189.248821987939,-188.413905076044,
-187.578988164149,-186.744071252255,-186.305304328339),.UNSPECIFIED.);
#1032=B_SPLINE_CURVE_WITH_KNOTS('',3,(#60937,#60938,#60939,#60940,#60941,
#60942,#60943,#60944,#60945,#60946,#60947,#60948,#60949,#60950,#60951,#60952,
#60953,#60954,#60955,#60956,#60957,#60958),.UNSPECIFIED.,.F.,.F.,(4,3,3,
3,3,3,3,4),(183.336022614352,183.665933723506,184.664118145917,185.662302568327,
186.660486990737,187.658671413148,188.656855835558,189.619207921532),
 .UNSPECIFIED.);
#1033=B_SPLINE_CURVE_WITH_KNOTS('',3,(#60963,#60964,#60965,#60966,#60967,
#60968,#60969,#60970,#60971,#60972,#60973,#60974,#60975,#60976,#60977,#60978,
#60979,#60980,#60981,#60982,#60983,#60984,#60985,#60986,#60987),
 .UNSPECIFIED.,.F.,.F.,(4,3,3,3,3,3,3,3,4),(-198.871674942698,-198.036758030803,
-197.201841118908,-196.366924207013,-195.532007295118,-194.697090383223,
-193.862173471329,-193.027256559434,-192.588489635518),.UNSPECIFIED.);
#1034=B_SPLINE_CURVE_WITH_KNOTS('',3,(#60988,#60989,#60990,#60991,#60992,
#60993,#60994,#60995,#60996,#60997,#60998,#60999,#61000,#61001,#61002,#61003,
#61004,#61005,#61006,#61007,#61008,#61009,#61010,#61011,#61012,#61013,#61014,
#61015,#61016,#61017,#61018,#61019,#61020,#61021),.UNSPECIFIED.,.F.,.F.,
(4,3,3,3,3,3,3,3,3,3,3,4),(189.619207921532,189.655040257969,190.653224680379,
191.152316891584,191.651409102789,192.6495935252,193.148685736405,193.64777794761,
194.146870158815,194.64596237002,195.644146792431,195.902393228711),
 .UNSPECIFIED.);
#1035=B_SPLINE_CURVE_WITH_KNOTS('',3,(#61026,#61027,#61028,#61029,#61030,
#61031,#61032,#61033,#61034,#61035,#61036,#61037,#61038,#61039,#61040,#61041,
#61042,#61043,#61044,#61045,#61046,#61047,#61048,#61049,#61050),
 .UNSPECIFIED.,.F.,.F.,(4,3,3,3,3,3,3,3,4),(-205.154860249877,-204.319943337983,
-203.485026426088,-202.650109514193,-201.815192602298,-200.980275690403,
-200.145358778508,-199.310441866614,-198.871674942698),.UNSPECIFIED.);
#1036=B_SPLINE_CURVE_WITH_KNOTS('',3,(#61051,#61052,#61053,#61054,#61055,
#61056,#61057,#61058,#61059,#61060,#61061,#61062,#61063,#61064,#61065,#61066,
#61067,#61068,#61069,#61070,#61071,#61072,#61073,#61074,#61075),
 .UNSPECIFIED.,.F.,.F.,(4,3,3,3,3,3,3,3,4),(195.902393228711,196.737310140606,
197.572227052501,198.407143964396,199.242060876291,200.076977788185,200.91189470008,
201.746811611975,202.185578535891),.UNSPECIFIED.);
#1037=B_SPLINE_CURVE_WITH_KNOTS('',3,(#61080,#61081,#61082,#61083,#61084,
#61085,#61086,#61087,#61088,#61089,#61090,#61091,#61092,#61093,#61094,#61095,
#61096,#61097,#61098,#61099,#61100,#61101,#61102,#61103,#61104,#61105,#61106,
#61107),.UNSPECIFIED.,.F.,.F.,(4,3,3,3,3,3,3,3,3,4),(-211.438045557057,
-210.616913128586,-209.618728706176,-208.620544283765,-208.12145207256,
-207.622359861355,-207.12326765015,-206.624175438945,-205.625991016534,
-205.154860249877),.UNSPECIFIED.);
#1038=B_SPLINE_CURVE_WITH_KNOTS('',3,(#61108,#61109,#61110,#61111,#61112,
#61113,#61114,#61115,#61116,#61117,#61118,#61119,#61120,#61121,#61122,#61123,
#61124,#61125,#61126,#61127,#61128,#61129,#61130,#61131,#61132,#61133,#61134,
#61135,#61136,#61137,#61138),.UNSPECIFIED.,.F.,.F.,(4,3,3,3,3,3,3,3,3,3,
4),(202.185578535891,202.631437749303,203.629622171714,204.627806594124,
205.126898805329,205.625991016534,206.624175438945,207.12326765015,207.622359861355,
208.12145207256,208.46876384307),.UNSPECIFIED.);
#1039=B_SPLINE_CURVE_WITH_KNOTS('',3,(#61143,#61144,#61145,#61146,#61147,
#61148,#61149,#61150,#61151,#61152,#61153,#61154,#61155,#61156,#61157,#61158,
#61159,#61160,#61161,#61162,#61163,#61164,#61165,#61166,#61167,#61168,#61169,
#61170,#61171,#61172,#61173,#61174,#61175,#61176),.UNSPECIFIED.,.F.,.F.,
(4,3,3,3,3,3,3,3,3,3,3,4),(-217.721230864237,-217.604204085459,-216.606019663048,
-215.607835240638,-215.108743029433,-214.609650818227,-214.110558607022,
-213.611466395817,-212.613281973407,-212.114189762202,-211.615097550996,
-211.438045557057),.UNSPECIFIED.);
#1040=B_SPLINE_CURVE_WITH_KNOTS('',3,(#61177,#61178,#61179,#61180,#61181,
#61182,#61183,#61184,#61185,#61186,#61187,#61188,#61189,#61190,#61191,#61192,
#61193,#61194,#61195,#61196,#61197,#61198,#61199,#61200,#61201,#61202,#61203,
#61204,#61205,#61206,#61207),.UNSPECIFIED.,.F.,.F.,(4,3,3,3,3,3,3,3,3,3,
4),(208.46876384307,208.620544283765,209.618728706176,210.616913128586,
211.615097550996,212.114189762202,212.613281973407,213.611466395817,214.110558607022,
214.609650818228,214.75194915025),.UNSPECIFIED.);
#1041=B_SPLINE_CURVE_WITH_KNOTS('',3,(#61212,#61213,#61214,#61215,#61216,
#61217,#61218,#61219,#61220,#61221,#61222,#61223,#61224,#61225,#61226,#61227,
#61228,#61229,#61230,#61231,#61232,#61233,#61234,#61235,#61236,#61237,#61238,
#61239,#61240,#61241,#61242),.UNSPECIFIED.,.F.,.F.,(4,3,3,3,3,3,3,3,3,3,
4),(-224.004416171416,-223.593310619921,-222.59512619751,-222.096033986305,
-221.5969417751,-221.097849563895,-220.59875735269,-219.600572930279,-219.101480719074,
-218.602388507869,-217.721230864237),.UNSPECIFIED.);
#1042=B_SPLINE_CURVE_WITH_KNOTS('',3,(#61243,#61244,#61245,#61246,#61247,
#61248,#61249,#61250,#61251,#61252,#61253,#61254,#61255,#61256,#61257,#61258,
#61259,#61260,#61261,#61262,#61263,#61264,#61265,#61266,#61267,#61268,#61269,
#61270),.UNSPECIFIED.,.F.,.F.,(4,3,3,3,3,3,3,3,3,4),(214.75194915025,215.108743029433,
215.607835240638,216.606019663048,217.604204085459,218.602388507869,219.101480719074,
219.600572930279,220.59875735269,221.03513445743),.UNSPECIFIED.);
#1043=B_SPLINE_CURVE_WITH_KNOTS('',3,(#61275,#61276,#61277,#61278,#61279,
#61280,#61281,#61282,#61283,#61284,#61285,#61286,#61287,#61288,#61289,#61290,
#61291,#61292,#61293,#61294,#61295,#61296,#61297,#61298,#61299),
 .UNSPECIFIED.,.F.,.F.,(4,3,3,3,3,3,3,3,4),(-230.287601478596,-229.452684566701,
-228.617767654806,-227.782850742911,-226.947933831016,-226.113016919121,
-225.278100007226,-224.443183095332,-224.004416171416),.UNSPECIFIED.);
#1044=B_SPLINE_CURVE_WITH_KNOTS('',3,(#61300,#61301,#61302,#61303,#61304,
#61305,#61306,#61307,#61308,#61309,#61310,#61311,#61312,#61313,#61314,#61315,
#61316,#61317,#61318,#61319,#61320,#61321,#61322,#61323,#61324),
 .UNSPECIFIED.,.F.,.F.,(4,3,3,3,3,3,3,3,4),(221.03513445743,221.870051369324,
222.704968281219,223.539885193114,224.374802105009,225.209719016904,226.044635928799,
226.879552840694,227.318319764609),.UNSPECIFIED.);
#1045=B_SPLINE_CURVE_WITH_KNOTS('',3,(#61329,#61330,#61331,#61332,#61333,
#61334,#61335,#61336,#61337,#61338,#61339,#61340,#61341,#61342,#61343,#61344,
#61345,#61346,#61347,#61348,#61349,#61350,#61351,#61352,#61353,#61354,#61355,
#61356,#61357,#61358,#61359),.UNSPECIFIED.,.F.,.F.,(4,3,3,3,3,3,3,3,3,3,
4),(-236.570786785775,-236.07061590005,-235.571523688845,-235.07243147764,
-234.573339266435,-233.575154844024,-233.076062632819,-232.576970421614,
-231.578785999204,-230.580601576793,-230.287601478596),.UNSPECIFIED.);
#1046=B_SPLINE_CURVE_WITH_KNOTS('',3,(#61360,#61361,#61362,#61363,#61364,
#61365,#61366,#61367,#61368,#61369,#61370,#61371,#61372,#61373,#61374,#61375,
#61376,#61377,#61378,#61379,#61380,#61381,#61382,#61383,#61384),
 .UNSPECIFIED.,.F.,.F.,(4,3,3,3,3,3,3,3,4),(227.318319764609,228.153236676504,
228.988153588399,229.823070500294,230.657987412188,231.492904324083,232.327821235978,
233.162738147873,233.601505071789),.UNSPECIFIED.);
#1047=B_SPLINE_CURVE_WITH_KNOTS('',3,(#61389,#61390,#61391,#61392,#61393,
#61394,#61395,#61396,#61397,#61398,#61399,#61400,#61401,#61402,#61403,#61404,
#61405,#61406,#61407,#61408,#61409,#61410,#61411,#61412,#61413,#61414,#61415,
#61416),.UNSPECIFIED.,.F.,.F.,(4,3,3,3,3,3,3,3,3,4),(-242.853972092955,
-242.558814645718,-242.059722434512,-241.560630223307,-240.562445800897,
-240.063353589692,-239.564261378486,-238.566076956076,-237.567892533666,
-236.570786785775),.UNSPECIFIED.);
#1048=B_SPLINE_CURVE_WITH_KNOTS('',3,(#61417,#61418,#61419,#61420,#61421,
#61422,#61423,#61424,#61425,#61426,#61427,#61428,#61429,#61430,#61431,#61432,
#61433,#61434,#61435,#61436,#61437,#61438,#61439,#61440,#61441,#61442,#61443,
#61444),.UNSPECIFIED.,.F.,.F.,(4,3,3,3,3,3,3,3,3,4),(233.601505071789,234.573339266435,
235.07243147764,235.571523688845,236.07061590005,236.569708111256,237.567892533666,
238.566076956076,239.564261378487,239.884690378968),.UNSPECIFIED.);
#1049=B_SPLINE_CURVE_WITH_KNOTS('',3,(#61449,#61450,#61451,#61452,#61453,
#61454,#61455,#61456,#61457,#61458,#61459,#61460,#61461,#61462,#61463,#61464,
#61465,#61466,#61467,#61468,#61469,#61470,#61471,#61472,#61473),
 .UNSPECIFIED.,.F.,.F.,(4,3,3,3,3,3,3,3,4),(-249.137157400134,-248.302240488239,
-247.467323576345,-246.63240666445,-245.797489752555,-244.96257284066,-244.127655928765,
-243.29273901687,-242.853972092955),.UNSPECIFIED.);
#1050=B_SPLINE_CURVE_WITH_KNOTS('',3,(#61474,#61475,#61476,#61477,#61478,
#61479,#61480,#61481,#61482,#61483,#61484,#61485,#61486,#61487,#61488,#61489,
#61490,#61491,#61492,#61493,#61494,#61495,#61496,#61497,#61498,#61499,#61500,
#61501,#61502,#61503,#61504),.UNSPECIFIED.,.F.,.F.,(4,3,3,3,3,3,3,3,3,3,
4),(239.884690378968,240.063353589692,240.562445800897,241.560630223307,
242.059722434512,242.558814645718,243.057906856923,243.556999068128,244.555183490538,
245.553367912949,246.167875686148),.UNSPECIFIED.);
#1051=B_SPLINE_CURVE_WITH_KNOTS('',3,(#61509,#61510,#61511,#61512,#61513,
#61514,#61515,#61516,#61517,#61518,#61519,#61520,#61521,#61522,#61523,#61524,
#61525,#61526,#61527,#61528,#61529,#61530,#61531,#61532,#61533,#61534,#61535,
#61536),.UNSPECIFIED.,.F.,.F.,(4,3,3,3,3,3,3,3,3,4),(-255.420342707314,
-254.537027714642,-254.037935503437,-253.538843292232,-252.540658869821,
-251.542474447411,-250.544290025,-250.045197813795,-249.54610560259,-249.137157400134),
 .UNSPECIFIED.);
#1052=B_SPLINE_CURVE_WITH_KNOTS('',3,(#61537,#61538,#61539,#61540,#61541,
#61542,#61543,#61544,#61545,#61546,#61547,#61548,#61549,#61550,#61551,#61552,
#61553,#61554,#61555,#61556,#61557,#61558,#61559,#61560,#61561,#61562,#61563,
#61564,#61565,#61566,#61567),.UNSPECIFIED.,.F.,.F.,(4,3,3,3,3,3,3,3,3,3,
4),(246.167875686148,246.551552335359,247.050644546564,247.549736757769,
248.54792118018,249.047013391385,249.54610560259,250.045197813795,250.544290025001,
251.542474447411,252.451060993327),.UNSPECIFIED.);
#1053=B_SPLINE_CURVE_WITH_KNOTS('',3,(#61572,#61573,#61574,#61575,#61576,
#61577,#61578,#61579,#61580,#61581,#61582,#61583,#61584,#61585,#61586,#61587,
#61588,#61589,#61590,#61591,#61592,#61593,#61594,#61595,#61596),
 .UNSPECIFIED.,.F.,.F.,(4,3,3,3,3,3,3,3,4),(-261.703528014493,-260.868611102599,
-260.033694190704,-259.198777278809,-258.363860366914,-257.528943455019,
-256.694026543124,-255.859109631229,-255.420342707314),.UNSPECIFIED.);
#1054=B_SPLINE_CURVE_WITH_KNOTS('',3,(#61597,#61598,#61599,#61600,#61601,
#61602,#61603,#61604,#61605,#61606,#61607,#61608,#61609,#61610,#61611,#61612,
#61613,#61614,#61615,#61616,#61617,#61618,#61619,#61620,#61621),
 .UNSPECIFIED.,.F.,.F.,(4,3,3,3,3,3,3,3,4),(252.451060993327,253.285977905222,
254.120894817117,254.955811729012,255.790728640907,256.625645552802,257.460562464697,
258.295479376592,258.734246300507),.UNSPECIFIED.);
#1055=B_SPLINE_CURVE_WITH_KNOTS('',3,(#61626,#61627,#61628,#61629,#61630,
#61631,#61632,#61633,#61634,#61635,#61636,#61637,#61638,#61639,#61640,#61641,
#61642,#61643,#61644,#61645,#61646,#61647,#61648,#61649,#61650),
 .UNSPECIFIED.,.F.,.F.,(4,3,3,3,3,3,3,3,4),(-267.986713321673,-267.151796409778,
-266.316879497883,-265.481962585988,-264.647045674094,-263.812128762199,
-262.977211850304,-262.142294938409,-261.703528014493),.UNSPECIFIED.);
#1056=B_SPLINE_CURVE_WITH_KNOTS('',3,(#61651,#61652,#61653,#61654,#61655,
#61656,#61657,#61658,#61659,#61660,#61661,#61662,#61663,#61664,#61665,#61666,
#61667,#61668,#61669,#61670,#61671,#61672,#61673,#61674,#61675),
 .UNSPECIFIED.,.F.,.F.,(4,3,3,3,3,3,3,3,4),(258.734246300507,259.569163212402,
260.404080124297,261.238997036192,262.073913948086,262.908830859981,263.743747771876,
264.578664683771,265.017431607686),.UNSPECIFIED.);
#1057=B_SPLINE_CURVE_WITH_KNOTS('',3,(#61680,#61681,#61682,#61683,#61684,
#61685,#61686,#61687,#61688,#61689,#61690,#61691,#61692,#61693,#61694,#61695,
#61696,#61697,#61698,#61699,#61700,#61701,#61702,#61703,#61704,#61705,#61706,
#61707,#61708,#61709,#61710),.UNSPECIFIED.,.F.,.F.,(4,3,3,3,3,3,3,3,3,3,
4),(-274.269898628853,-273.502531740439,-272.504347318028,-271.506162895618,
-271.007070684413,-270.507978473208,-270.008886262002,-269.509794050797,
-268.511609628387,-268.012517417182,-267.986713321673),.UNSPECIFIED.);
#1058=B_SPLINE_CURVE_WITH_KNOTS('',3,(#61711,#61712,#61713,#61714,#61715,
#61716,#61717,#61718,#61719,#61720,#61721,#61722,#61723,#61724,#61725,#61726,
#61727,#61728,#61729,#61730,#61731,#61732,#61733,#61734,#61735,#61736,#61737,
#61738,#61739,#61740,#61741),.UNSPECIFIED.,.F.,.F.,(4,3,3,3,3,3,3,3,3,3,
4),(265.017431607686,265.517056361156,266.515240783566,267.513425205977,
268.012517417182,268.511609628387,269.509794050797,270.008886262003,270.507978473208,
271.007070684413,271.300616914866),.UNSPECIFIED.);
#1059=B_SPLINE_CURVE_WITH_KNOTS('',3,(#61746,#61747,#61748,#61749,#61750,
#61751,#61752,#61753,#61754,#61755,#61756,#61757,#61758,#61759,#61760,#61761,
#61762,#61763,#61764,#61765,#61766,#61767,#61768,#61769,#61770,#61771,#61772,
#61773,#61774,#61775,#61776,#61777,#61778,#61779),.UNSPECIFIED.,.F.,.F.,
(4,3,3,3,3,3,3,3,3,3,3,4),(-280.553083936032,-280.489822697311,-279.491638274901,
-278.493453852491,-277.994361641285,-277.49526943008,-276.996177218875,
-276.49708500767,-275.498900585259,-274.999808374054,-274.500716162849,
-274.269898628853),.UNSPECIFIED.);
#1060=B_SPLINE_CURVE_WITH_KNOTS('',3,(#61780,#61781,#61782,#61783,#61784,
#61785,#61786,#61787,#61788,#61789,#61790,#61791,#61792,#61793,#61794,#61795,
#61796,#61797,#61798,#61799,#61800,#61801,#61802,#61803,#61804,#61805,#61806,
#61807,#61808,#61809,#61810),.UNSPECIFIED.,.F.,.F.,(4,3,3,3,3,3,3,3,3,3,
4),(271.300616914866,271.506162895618,272.504347318028,273.502531740439,
274.500716162849,274.999808374054,275.498900585259,276.49708500767,276.996177218875,
277.49526943008,277.583802222046),.UNSPECIFIED.);
#1061=B_SPLINE_CURVE_WITH_KNOTS('',3,(#61815,#61816,#61817,#61818,#61819,
#61820,#61821,#61822,#61823,#61824,#61825,#61826,#61827,#61828,#61829,#61830,
#61831,#61832,#61833,#61834,#61835,#61836,#61837,#61838,#61839,#61840,#61841,
#61842,#61843,#61844,#61845),.UNSPECIFIED.,.F.,.F.,(4,3,3,3,3,3,3,3,3,3,
4),(-286.836269243212,-286.478929231773,-285.480744809363,-284.981652598158,
-284.482560386953,-283.983468175747,-283.484375964542,-282.486191542132,
-281.987099330927,-281.488007119722,-280.553083936032),.UNSPECIFIED.);
#1062=B_SPLINE_CURVE_WITH_KNOTS('',3,(#61846,#61847,#61848,#61849,#61850,
#61851,#61852,#61853,#61854,#61855,#61856,#61857,#61858,#61859,#61860,#61861,
#61862,#61863,#61864,#61865,#61866,#61867,#61868,#61869,#61870,#61871,#61872,
#61873),.UNSPECIFIED.,.F.,.F.,(4,3,3,3,3,3,3,3,3,4),(277.583802222046,277.994361641285,
278.493453852491,279.491638274901,280.489822697311,281.488007119722,281.987099330927,
282.486191542132,283.484375964542,283.866987529225),.UNSPECIFIED.);
#1063=B_SPLINE_CURVE_WITH_KNOTS('',3,(#61878,#61879,#61880,#61881,#61882,
#61883,#61884,#61885,#61886,#61887,#61888,#61889,#61890,#61891,#61892,#61893,
#61894,#61895,#61896,#61897,#61898,#61899,#61900,#61901,#61902),
 .UNSPECIFIED.,.F.,.F.,(4,3,3,3,3,3,3,3,4),(-293.119454550391,-292.284537638496,
-291.449620726602,-290.614703814707,-289.779786902812,-288.944869990917,
-288.109953079022,-287.275036167127,-286.836269243212),.UNSPECIFIED.);
#1064=B_SPLINE_CURVE_WITH_KNOTS('',3,(#61903,#61904,#61905,#61906,#61907,
#61908,#61909,#61910,#61911,#61912,#61913,#61914,#61915,#61916,#61917,#61918,
#61919,#61920,#61921,#61922,#61923,#61924,#61925,#61926,#61927),
 .UNSPECIFIED.,.F.,.F.,(4,3,3,3,3,3,3,3,4),(283.866987529225,284.70190444112,
285.536821353015,286.37173826491,287.206655176804,288.041572088699,288.876489000594,
289.711405912489,290.150172836405),.UNSPECIFIED.);
#1065=B_SPLINE_CURVE_WITH_KNOTS('',3,(#61932,#61933,#61934,#61935,#61936,
#61937,#61938,#61939,#61940,#61941,#61942,#61943,#61944,#61945,#61946,#61947,
#61948,#61949,#61950,#61951,#61952,#61953,#61954,#61955,#61956,#61957,#61958,
#61959,#61960,#61961,#61962),.UNSPECIFIED.,.F.,.F.,(4,3,3,3,3,3,3,3,3,3,
4),(-299.402639857571,-298.956234511903,-298.457142300698,-297.958050089493,
-297.458957878287,-296.460773455877,-295.961681244672,-295.462589033467,
-294.464404611056,-293.466220188646,-293.119454550391),.UNSPECIFIED.);
#1066=B_SPLINE_CURVE_WITH_KNOTS('',3,(#61963,#61964,#61965,#61966,#61967,
#61968,#61969,#61970,#61971,#61972,#61973,#61974,#61975,#61976,#61977,#61978,
#61979,#61980,#61981,#61982,#61983,#61984,#61985,#61986,#61987,#61988,#61989,
#61990,#61991,#61992,#61993),.UNSPECIFIED.,.F.,.F.,(4,3,3,3,3,3,3,3,3,3,
4),(290.150172836405,290.471666921415,290.97075913262,291.469851343825,
291.96894355503,292.468035766236,293.466220188646,294.464404611056,295.462589033467,
295.961681244672,296.433358143584),.UNSPECIFIED.);
#1067=B_SPLINE_CURVE_WITH_KNOTS('',3,(#61998,#61999,#62000,#62001,#62002,
#62003,#62004,#62005,#62006,#62007,#62008,#62009,#62010,#62011,#62012,#62013,
#62014,#62015,#62016,#62017,#62018,#62019,#62020,#62021,#62022,#62023,#62024,
#62025,#62026,#62027,#62028),.UNSPECIFIED.,.F.,.F.,(4,3,3,3,3,3,3,3,3,3,
4),(-305.68582516475,-305.44443325757,-304.945341046365,-304.44624883516,
-303.448064412749,-302.948972201544,-302.449879990339,-301.451695567929,
-300.453511145518,-299.455326723108,-299.402639857571),.UNSPECIFIED.);
#1068=B_SPLINE_CURVE_WITH_KNOTS('',3,(#62029,#62030,#62031,#62032,#62033,
#62034,#62035,#62036,#62037,#62038,#62039,#62040,#62041,#62042,#62043,#62044,
#62045,#62046,#62047,#62048,#62049,#62050,#62051,#62052,#62053,#62054,#62055,
#62056,#62057,#62058,#62059),.UNSPECIFIED.,.F.,.F.,(4,3,3,3,3,3,3,3,3,3,
4),(296.433358143584,296.460773455877,297.458957878287,297.958050089493,
298.457142300698,298.956234511903,299.455326723108,300.453511145519,301.451695567929,
302.449879990339,302.716543450764),.UNSPECIFIED.);
#1069=B_SPLINE_CURVE_WITH_KNOTS('',3,(#62064,#62065,#62066,#62067,#62068,
#62069,#62070,#62071,#62072,#62073,#62074,#62075,#62076,#62077,#62078,#62079,
#62080,#62081,#62082,#62083,#62084,#62085,#62086,#62087,#62088),
 .UNSPECIFIED.,.F.,.F.,(4,3,3,3,3,3,3,3,4),(-311.96901047193,-311.134093560035,
-310.29917664814,-309.464259736245,-308.62934282435,-307.794425912456,-306.959509000561,
-306.124592088666,-305.68582516475),.UNSPECIFIED.);
#1070=B_SPLINE_CURVE_WITH_KNOTS('',3,(#62089,#62090,#62091,#62092,#62093,
#62094,#62095,#62096,#62097,#62098,#62099,#62100,#62101,#62102,#62103,#62104,
#62105,#62106,#62107,#62108,#62109,#62110,#62111,#62112,#62113,#62114,#62115,
#62116,#62117,#62118,#62119),.UNSPECIFIED.,.F.,.F.,(4,3,3,3,3,3,3,3,3,3,
4),(302.716543450764,302.948972201544,303.44806441275,304.44624883516,304.945341046365,
305.44443325757,305.943525468776,306.442617679981,307.440802102391,308.438986524802,
308.999728757943),.UNSPECIFIED.);
#1071=B_SPLINE_CURVE_WITH_KNOTS('',3,(#62124,#62125,#62126,#62127,#62128,
#62129,#62130,#62131,#62132,#62133,#62134,#62135,#62136,#62137,#62138,#62139,
#62140,#62141,#62142,#62143,#62144,#62145,#62146,#62147,#62148),
 .UNSPECIFIED.,.F.,.F.,(4,3,3,3,3,3,3,3,4),(-318.25219577911,-317.417278867215,
-316.58236195532,-315.747445043425,-314.91252813153,-314.077611219635,-313.24269430774,
-312.407777395845,-311.96901047193),.UNSPECIFIED.);
#1072=B_SPLINE_CURVE_WITH_KNOTS('',3,(#62149,#62150,#62151,#62152,#62153,
#62154,#62155,#62156,#62157,#62158,#62159,#62160,#62161,#62162,#62163,#62164,
#62165,#62166,#62167,#62168,#62169,#62170,#62171,#62172,#62173,#62174,#62175,
#62176,#62177,#62178,#62179),.UNSPECIFIED.,.F.,.F.,(4,3,3,3,3,3,3,3,3,3,
4),(308.999728757943,309.437170947212,309.936263158417,310.435355369622,
311.433539792033,311.932632003238,312.431724214443,312.930816425648,313.429908636853,
314.428093059264,315.282914065123),.UNSPECIFIED.);
#1073=B_SPLINE_CURVE_WITH_KNOTS('',3,(#62184,#62185,#62186,#62187,#62188,
#62189,#62190,#62191,#62192,#62193,#62194,#62195,#62196,#62197,#62198,#62199,
#62200,#62201,#62202,#62203,#62204,#62205,#62206,#62207,#62208),
 .UNSPECIFIED.,.F.,.F.,(4,3,3,3,3,3,3,3,4),(-324.535381086289,-323.700464174394,
-322.865547262499,-322.030630350604,-321.19571343871,-320.360796526815,
-319.52587961492,-318.690962703025,-318.25219577911),.UNSPECIFIED.);
#1074=B_SPLINE_CURVE_WITH_KNOTS('',3,(#62209,#62210,#62211,#62212,#62213,
#62214,#62215,#62216,#62217,#62218,#62219,#62220,#62221,#62222,#62223,#62224,
#62225,#62226,#62227,#62228,#62229,#62230,#62231,#62232,#62233),
 .UNSPECIFIED.,.F.,.F.,(4,3,3,3,3,3,3,3,4),(315.282914065123,316.117830977018,
316.952747888913,317.787664800807,318.622581712702,319.457498624597,320.292415536492,
321.127332448387,321.566099372303),.UNSPECIFIED.);
#1075=B_SPLINE_CURVE_WITH_KNOTS('',3,(#62238,#62239,#62240,#62241,#62242,
#62243,#62244,#62245,#62246,#62247,#62248,#62249,#62250,#62251,#62252,#62253,
#62254,#62255,#62256,#62257,#62258,#62259,#62260,#62261,#62262,#62263,#62264,
#62265),.UNSPECIFIED.,.F.,.F.,(4,3,3,3,3,3,3,3,3,4),(-330.818566393469,
-330.399043817829,-329.400859395419,-328.402674973009,-327.404490550598,
-326.905398339393,-326.406306128188,-325.907213916983,-325.408121705777,
-324.535381086289),.UNSPECIFIED.);
#1076=B_SPLINE_CURVE_WITH_KNOTS('',3,(#62266,#62267,#62268,#62269,#62270,
#62271,#62272,#62273,#62274,#62275,#62276,#62277,#62278,#62279,#62280,#62281,
#62282,#62283,#62284,#62285,#62286,#62287,#62288,#62289,#62290),
 .UNSPECIFIED.,.F.,.F.,(4,3,3,3,3,3,3,3,4),(321.566099372303,322.401016284197,
323.235933196092,324.070850107987,324.905767019882,325.740683931777,326.575600843672,
327.410517755567,327.849284679482),.UNSPECIFIED.);
#1077=B_SPLINE_CURVE_WITH_KNOTS('',3,(#62295,#62296,#62297,#62298,#62299,
#62300,#62301,#62302,#62303,#62304,#62305,#62306,#62307,#62308,#62309,#62310,
#62311,#62312,#62313,#62314,#62315,#62316,#62317,#62318,#62319,#62320,#62321,
#62322,#62323,#62324,#62325),.UNSPECIFIED.,.F.,.F.,(4,3,3,3,3,3,3,3,3,3,
4),(-337.101751700648,-336.388150352291,-335.389965929881,-334.391781507471,
-333.892689296266,-333.39359708506,-332.894504873855,-332.39541266265,-331.39722824024,
-330.898136029034,-330.818566393469),.UNSPECIFIED.);
#1078=B_SPLINE_CURVE_WITH_KNOTS('',3,(#62326,#62327,#62328,#62329,#62330,
#62331,#62332,#62333,#62334,#62335,#62336,#62337,#62338,#62339,#62340,#62341,
#62342,#62343,#62344,#62345,#62346,#62347,#62348,#62349,#62350,#62351,#62352,
#62353,#62354,#62355,#62356),.UNSPECIFIED.,.F.,.F.,(4,3,3,3,3,3,3,3,3,3,
4),(327.849284679482,328.402674973009,329.400859395419,330.399043817829,
330.898136029035,331.39722824024,332.39541266265,332.894504873855,333.39359708506,
333.892689296266,334.132469986662),.UNSPECIFIED.);
#1079=B_SPLINE_CURVE_WITH_KNOTS('',3,(#62361,#62362,#62363,#62364,#62365,
#62366,#62367,#62368,#62369,#62370,#62371,#62372,#62373,#62374,#62375,#62376,
#62377,#62378,#62379,#62380,#62381,#62382,#62383,#62384,#62385,#62386,#62387,
#62388,#62389,#62390,#62391,#62392,#62393,#62394),.UNSPECIFIED.,.F.,.F.,
(4,3,3,3,3,3,3,3,3,3,3,4),(-343.384937007828,-343.375441309164,-342.377256886754,
-341.379072464343,-340.879980253138,-340.380888041933,-339.881795830728,
-339.382703619523,-338.384519197112,-337.885426985907,-337.386334774702,
-337.101751700648),.UNSPECIFIED.);
#1080=B_SPLINE_CURVE_WITH_KNOTS('',3,(#62395,#62396,#62397,#62398,#62399,
#62400,#62401,#62402,#62403,#62404,#62405,#62406,#62407,#62408,#62409,#62410,
#62411,#62412,#62413,#62414,#62415,#62416,#62417,#62418,#62419,#62420,#62421,
#62422,#62423,#62424,#62425),.UNSPECIFIED.,.F.,.F.,(4,3,3,3,3,3,3,3,3,3,
4),(334.132469986662,334.391781507471,335.389965929881,336.388150352292,
337.386334774702,337.885426985907,338.384519197112,339.382703619523,339.881795830728,
340.380888041933,340.415655293841),.UNSPECIFIED.);
#1081=B_SPLINE_CURVE_WITH_KNOTS('',3,(#62430,#62431,#62432,#62433,#62434,
#62435,#62436,#62437,#62438,#62439,#62440,#62441,#62442,#62443,#62444,#62445,
#62446,#62447,#62448,#62449,#62450,#62451,#62452,#62453,#62454,#62455,#62456,
#62457,#62458,#62459,#62460),.UNSPECIFIED.,.F.,.F.,(4,3,3,3,3,3,3,3,3,3,
4),(-349.668122315007,-349.364547843626,-348.366363421216,-347.867271210011,
-347.368178998805,-346.8690867876,-346.369994576395,-345.371810153985,-344.87271794278,
-344.373625731574,-343.384937007828),.UNSPECIFIED.);
#1082=B_SPLINE_CURVE_WITH_KNOTS('',3,(#62461,#62462,#62463,#62464,#62465,
#62466,#62467,#62468,#62469,#62470,#62471,#62472,#62473,#62474,#62475,#62476,
#62477,#62478,#62479,#62480,#62481,#62482,#62483,#62484,#62485,#62486,#62487,
#62488),.UNSPECIFIED.,.F.,.F.,(4,3,3,3,3,3,3,3,3,4),(340.415655293841,340.879980253138,
341.379072464343,342.377256886754,343.375441309164,344.373625731574,344.87271794278,
345.371810153985,346.369994576395,346.698840601021),.UNSPECIFIED.);
#1083=B_SPLINE_CURVE_WITH_KNOTS('',3,(#62493,#62494,#62495,#62496,#62497,
#62498,#62499,#62500,#62501,#62502,#62503,#62504,#62505,#62506,#62507,#62508,
#62509,#62510,#62511,#62512,#62513,#62514,#62515,#62516,#62517),
 .UNSPECIFIED.,.F.,.F.,(4,3,3,3,3,3,3,3,4),(-355.951307622187,-355.116390710292,
-354.281473798397,-353.446556886502,-352.611639974607,-351.776723062712,
-350.941806150817,-350.106889238922,-349.668122315007),.UNSPECIFIED.);
#1084=B_SPLINE_CURVE_WITH_KNOTS('',3,(#62518,#62519,#62520,#62521,#62522,
#62523,#62524,#62525,#62526,#62527,#62528,#62529,#62530,#62531,#62532,#62533,
#62534,#62535,#62536,#62537,#62538,#62539,#62540,#62541,#62542),
 .UNSPECIFIED.,.F.,.F.,(4,3,3,3,3,3,3,3,4),(346.698840601021,347.533757512916,
348.36867442481,349.203591336705,350.0385082486,350.873425160495,351.70834207239,
352.543258984285,352.9820259082),.UNSPECIFIED.);
#1085=B_SPLINE_CURVE_WITH_KNOTS('',3,(#62547,#62548,#62549,#62550,#62551,
#62552,#62553,#62554,#62555,#62556,#62557,#62558,#62559,#62560,#62561,#62562,
#62563,#62564,#62565,#62566,#62567,#62568,#62569,#62570,#62571,#62572,#62573,
#62574,#62575,#62576,#62577),.UNSPECIFIED.,.F.,.F.,(4,3,3,3,3,3,3,3,3,3,
4),(-362.234492929366,-361.841853123756,-361.34276091255,-360.843668701345,
-360.34457649014,-359.34639206773,-358.847299856525,-358.348207645319,-357.350023222909,
-356.351838800499,-355.951307622187),.UNSPECIFIED.);
#1086=B_SPLINE_CURVE_WITH_KNOTS('',3,(#62578,#62579,#62580,#62581,#62582,
#62583,#62584,#62585,#62586,#62587,#62588,#62589,#62590,#62591,#62592,#62593,
#62594,#62595,#62596,#62597,#62598,#62599,#62600,#62601,#62602,#62603,#62604,
#62605,#62606,#62607,#62608),.UNSPECIFIED.,.F.,.F.,(4,3,3,3,3,3,3,3,3,3,
4),(352.9820259082,353.357285533268,353.856377744473,354.355469955678,354.854562166883,
355.353654378088,356.351838800499,357.350023222909,358.348207645319,358.847299856525,
359.26521121538),.UNSPECIFIED.);
#1087=B_SPLINE_CURVE_WITH_KNOTS('',3,(#62613,#62614,#62615,#62616,#62617,
#62618,#62619,#62620,#62621,#62622,#62623,#62624,#62625,#62626,#62627,#62628,
#62629,#62630,#62631,#62632,#62633,#62634,#62635,#62636,#62637,#62638,#62639,
#62640,#62641,#62642,#62643),.UNSPECIFIED.,.F.,.F.,(4,3,3,3,3,3,3,3,3,3,
4),(-368.517678236546,-368.330051869423,-367.830959658218,-367.331867447013,
-366.333683024602,-365.834590813397,-365.335498602192,-364.337314179782,
-363.339129757371,-362.340945334961,-362.234492929366),.UNSPECIFIED.);
#1088=B_SPLINE_CURVE_WITH_KNOTS('',3,(#62644,#62645,#62646,#62647,#62648,
#62649,#62650,#62651,#62652,#62653,#62654,#62655,#62656,#62657,#62658,#62659,
#62660,#62661,#62662,#62663,#62664,#62665,#62666,#62667,#62668,#62669,#62670,
#62671,#62672,#62673,#62674),.UNSPECIFIED.,.F.,.F.,(4,3,3,3,3,3,3,3,3,3,
4),(359.26521121538,359.34639206773,360.34457649014,360.843668701345,361.342760912551,
361.841853123756,362.340945334961,363.339129757371,364.337314179782,365.335498602192,
365.54839652256),.UNSPECIFIED.);
#1089=B_SPLINE_CURVE_WITH_KNOTS('',3,(#62681,#62682,#62683,#62684,#62685,
#62686,#62687,#62688,#62689,#62690,#62691,#62692,#62693,#62694,#62695,#62696,
#62697,#62698,#62699,#62700,#62701,#62702),.UNSPECIFIED.,.F.,.F.,(4,3,3,
3,3,3,3,4),(-374.319158403885,-373.48424149199,-372.649324580095,-371.8144076682,
-370.979490756305,-370.14457384441,-369.309656932515,-368.517678236546),
 .UNSPECIFIED.);
#1090=B_SPLINE_CURVE_WITH_KNOTS('',3,(#62703,#62704,#62705,#62706,#62707,
#62708,#62709,#62710,#62711,#62712,#62713,#62714,#62715,#62716,#62717,#62718,
#62719,#62720,#62721,#62722,#62723,#62724,#62725,#62726,#62727,#62728,#62729,
#62730,#62731,#62732,#62733),.UNSPECIFIED.,.F.,.F.,(4,3,3,3,3,3,3,3,3,3,
4),(365.54839652256,365.834590813397,366.333683024602,367.331867447013,
367.830959658218,368.330051869423,368.829144080628,369.328236291833,370.326420714244,
371.324605136654,371.831581829739),.UNSPECIFIED.);
#1091=B_SPLINE_CURVE_WITH_KNOTS('',3,(#62739,#62740,#62741,#62742,#62743,
#62744,#62745,#62746,#62747,#62748,#62749,#62750,#62751,#62752,#62753,#62754),
 .UNSPECIFIED.,.F.,.F.,(4,3,3,3,3,4),(380.132711084365,380.584976729012,
381.45314130285,382.321305876688,383.189470450526,383.85920477902),
 .UNSPECIFIED.);
#1092=B_SPLINE_CURVE_WITH_KNOTS('',3,(#62757,#62758,#62759,#62760,#62761,
#62762,#62763,#62764),.UNSPECIFIED.,.F.,.F.,(4,1,1,1,1,4),(380.132711084365,
380.623918813691,381.123011024896,381.622103236102,382.121195447307,382.620287658512),
 .UNSPECIFIED.);
#1093=B_SPLINE_CURVE_WITH_KNOTS('',3,(#62769,#62770,#62771,#62772,#62773,
#62774,#62775,#62776,#62777,#62778,#62779,#62780,#62781),.UNSPECIFIED.,
 .F.,.F.,(4,1,1,1,1,1,1,1,1,1,4),(373.849525777185,373.95597818278,374.95416260519,
375.9523470276,376.950531450011,377.449623661216,377.948715872421,378.946900294831,
379.445992506037,379.945084717242,380.132711084365),.UNSPECIFIED.);
#1094=B_SPLINE_CURVE_WITH_KNOTS('',3,(#62782,#62783,#62784,#62785,#62786,
#62787,#62788,#62789,#62790,#62791,#62792,#62793,#62794),.UNSPECIFIED.,
 .F.,.F.,(4,1,1,1,1,1,1,1,1,1,4),(373.849525777185,374.135720068024,374.634812279229,
375.632996701639,376.132088912845,376.63118112405,377.130273335255,377.62936554646,
378.627549968871,379.625734391281,380.132711084365),.UNSPECIFIED.);
#1095=B_SPLINE_CURVE_WITH_KNOTS('',3,(#62799,#62800,#62801,#62802,#62803,
#62804,#62805,#62806,#62807,#62808,#62809,#62810,#62811),.UNSPECIFIED.,
 .F.,.F.,(4,1,1,1,1,1,1,1,1,1,4),(367.566340470006,367.966871648318,368.965056070728,
369.963240493138,370.462332704343,370.961424915549,371.959609337959,372.458701549164,
372.957793760369,373.456885971574,373.849525777185),.UNSPECIFIED.);
#1096=B_SPLINE_CURVE_WITH_KNOTS('',3,(#62812,#62813,#62814,#62815,#62816,
#62817,#62818,#62819,#62820,#62821,#62822,#62823,#62824),.UNSPECIFIED.,
 .F.,.F.,(4,1,1,1,1,1,1,1,1,1,4),(367.566340470006,367.647521322357,368.645705744767,
369.144797955972,369.643890167177,370.142982378382,370.642074589588,371.640259011998,
372.638443434408,373.636627856819,373.849525777185),.UNSPECIFIED.);
#1097=B_SPLINE_CURVE_WITH_KNOTS('',3,(#62829,#62830,#62831,#62832,#62833,
#62834,#62835,#62836,#62837,#62838,#62839,#62840,#62841,#62842,#62843,#62844,
#62845,#62846,#62847,#62848,#62849,#62850,#62851,#62852,#62853,#62854,#62855,
#62856),.UNSPECIFIED.,.F.,.F.,(4,3,3,3,3,3,3,3,3,4),(361.283155162826,361.485356104573,
362.353520678412,363.22168525225,364.089849826088,364.958014399926,365.826178973764,
366.694343547602,367.56250812144,367.566340470006),.UNSPECIFIED.);
#1098=B_SPLINE_CURVE_WITH_KNOTS('',3,(#62857,#62858,#62859,#62860,#62861,
#62862,#62863,#62864,#62865,#62866,#62867,#62868,#62869),.UNSPECIFIED.,
 .F.,.F.,(4,1,1,1,1,1,1,1,1,1,4),(361.283155162826,361.658414787894,362.1575069991,
362.656599210305,363.15569142151,363.654783632715,364.652968055125,365.651152477536,
366.649336899946,367.148429111151,367.566340470006),.UNSPECIFIED.);
#1099=B_SPLINE_CURVE_WITH_KNOTS('',3,(#62874,#62875,#62876,#62877,#62878,
#62879,#62880,#62881,#62882,#62883,#62884,#62885,#62886),.UNSPECIFIED.,
 .F.,.F.,(4,1,1,1,1,1,1,1,1,1,4),(354.999969855647,355.988658579393,356.487750790598,
356.986843001804,357.985027424214,358.484119635419,358.983211846624,359.48230405783,
359.981396269035,360.979580691445,361.283155162826),.UNSPECIFIED.);
#1100=B_SPLINE_CURVE_WITH_KNOTS('',3,(#62887,#62888,#62889,#62890,#62891,
#62892,#62893,#62894,#62895,#62896,#62897,#62898,#62899,#62900,#62901,#62902,
#62903,#62904,#62905,#62906,#62907,#62908,#62909,#62910,#62911,#62912,#62913,
#62914),.UNSPECIFIED.,.F.,.F.,(4,3,3,3,3,3,3,3,3,4),(354.999969855647,355.037451541037,
355.905616114875,356.773780688713,357.641945262551,358.510109836389,359.378274410227,
360.246438984065,361.114603557904,361.283155162826),.UNSPECIFIED.);
#1101=B_SPLINE_CURVE_WITH_KNOTS('',3,(#62919,#62920,#62921,#62922,#62923,
#62924,#62925,#62926,#62927,#62928,#62929,#62930,#62931,#62932),
 .UNSPECIFIED.,.F.,.F.,(4,1,1,1,1,1,1,1,1,1,1,4),(348.716784548467,349.001367622521,
349.500459833726,349.999552044931,350.997736467341,351.496828678547,351.995920889752,
352.495013100957,352.994105312162,353.992289734573,354.990474156983,354.999969855647),
 .UNSPECIFIED.);
#1102=B_SPLINE_CURVE_WITH_KNOTS('',3,(#62933,#62934,#62935,#62936,#62937,
#62938,#62939,#62940,#62941,#62942,#62943,#62944),.UNSPECIFIED.,.F.,.F.,
(4,1,1,1,1,1,1,1,1,4),(348.716784548467,349.181109507765,349.68020171897,
350.67838614138,351.676570563791,352.674754986201,353.173847197406,353.672939408612,
354.671123831022,354.999969855647),.UNSPECIFIED.);
#1103=B_SPLINE_CURVE_WITH_KNOTS('',3,(#62949,#62950,#62951,#62952,#62953,
#62954,#62955,#62956,#62957,#62958,#62959,#62960,#62961),.UNSPECIFIED.,
 .F.,.F.,(4,1,1,1,1,1,1,1,1,1,4),(342.433599241287,342.513168876853,343.012261088059,
344.010445510469,344.509537721674,345.008629932879,345.507722144084,346.00681435529,
347.0049987777,348.00318320011,348.716784548467),.UNSPECIFIED.);
#1104=B_SPLINE_CURVE_WITH_KNOTS('',3,(#62962,#62963,#62964,#62965,#62966,
#62967,#62968,#62969,#62970,#62971,#62972,#62973,#62974),.UNSPECIFIED.,
 .F.,.F.,(4,1,1,1,1,1,1,1,1,1,4),(342.433599241288,342.692910762098,343.691095184508,
344.689279606918,345.687464029329,346.186556240534,346.685648451739,347.683832874149,
348.182925085355,348.68201729656,348.716784548467),.UNSPECIFIED.);
#1105=B_SPLINE_CURVE_WITH_KNOTS('',3,(#62979,#62980,#62981,#62982,#62983,
#62984,#62985,#62986,#62987,#62988,#62989,#62990),.UNSPECIFIED.,.F.,.F.,
(4,1,1,1,1,1,1,1,1,4),(336.150413934108,337.023154553596,337.522246764802,
338.021338976007,338.520431187212,339.019523398417,340.017707820827,341.015892243238,
342.014076665648,342.433599241287),.UNSPECIFIED.);
#1106=B_SPLINE_CURVE_WITH_KNOTS('',3,(#62991,#62992,#62993,#62994,#62995,
#62996,#62997,#62998,#62999,#63000,#63001,#63002,#63003),.UNSPECIFIED.,
 .F.,.F.,(4,1,1,1,1,1,1,1,1,1,4),(336.150413934108,336.703804227635,337.701988650046,
338.700173072456,339.199265283661,339.698357494866,340.696541917277,341.195634128482,
341.694726339687,342.193818550892,342.433599241288),.UNSPECIFIED.);
#1107=B_SPLINE_CURVE_WITH_KNOTS('',3,(#63008,#63009,#63010,#63011,#63012,
#63013,#63014,#63015,#63016,#63017,#63018,#63019,#63020,#63021,#63022,#63023,
#63024,#63025,#63026,#63027,#63028,#63029,#63030,#63031,#63032),
 .UNSPECIFIED.,.F.,.F.,(4,3,3,3,3,3,3,3,4),(329.867228626928,330.231431446402,
331.09959602024,331.967760594078,332.835925167916,333.704089741754,334.572254315592,
335.44041888943,336.150413934108),.UNSPECIFIED.);
#1108=B_SPLINE_CURVE_WITH_KNOTS('',3,(#63033,#63034,#63035,#63036,#63037,
#63038,#63039,#63040,#63041,#63042,#63043,#63044,#63045),.UNSPECIFIED.,
 .F.,.F.,(4,1,1,1,1,1,1,1,1,1,4),(329.867228626928,330.714697693173,331.712882115584,
332.211974326789,332.711066537994,333.709250960404,334.208343171609,334.707435382815,
335.20652759402,335.705619805225,336.150413934108),.UNSPECIFIED.);
#1109=B_SPLINE_CURVE_WITH_KNOTS('',3,(#63050,#63051,#63052,#63053,#63054,
#63055,#63056,#63057,#63058,#63059,#63060,#63061),.UNSPECIFIED.,.F.,.F.,
(4,1,1,1,1,1,1,1,1,4),(323.584043319749,324.046757062262,324.545849273467,
325.044941484672,326.043125907082,327.041310329493,328.039494751903,328.538586963108,
329.037679174313,329.867228626928),.UNSPECIFIED.);
#1110=B_SPLINE_CURVE_WITH_KNOTS('',3,(#63062,#63063,#63064,#63065,#63066,
#63067,#63068,#63069,#63070,#63071,#63072,#63073,#63074,#63075),
 .UNSPECIFIED.,.F.,.F.,(4,1,1,1,1,1,1,1,1,1,1,4),(323.584043319749,323.727406736301,
324.725591158711,325.224683369916,325.723775581121,326.721960003532,327.221052214737,
327.720144425942,328.219236637147,328.718328848352,329.716513270763,329.867228626928),
 .UNSPECIFIED.);
#1111=B_SPLINE_CURVE_WITH_KNOTS('',3,(#63080,#63081,#63082,#63083,#63084,
#63085,#63086,#63087,#63088,#63089,#63090,#63091,#63092,#63093,#63094,#63095,
#63096,#63097,#63098,#63099,#63100,#63101,#63102,#63103,#63104),
 .UNSPECIFIED.,.F.,.F.,(4,3,3,3,3,3,3,3,4),(317.300858012569,318.077127412668,
318.945291986507,319.813456560345,320.681621134183,321.549785708021,322.417950281859,
323.286114855697,323.584043319749),.UNSPECIFIED.);
#1112=B_SPLINE_CURVE_WITH_KNOTS('',3,(#63105,#63106,#63107,#63108,#63109,
#63110,#63111,#63112,#63113,#63114,#63115,#63116,#63117),.UNSPECIFIED.,
 .F.,.F.,(4,1,1,1,1,1,1,1,1,1,4),(317.300858012569,317.738300201839,318.237392413044,
318.736484624249,319.734669046659,320.233761257864,320.73285346907,321.231945680275,
321.73103789148,322.72922231389,323.584043319749),.UNSPECIFIED.);
#1113=B_SPLINE_CURVE_WITH_KNOTS('',3,(#63122,#63123,#63124,#63125,#63126,
#63127,#63128,#63129,#63130,#63131,#63132,#63133,#63134),.UNSPECIFIED.,
 .F.,.F.,(4,1,1,1,1,1,1,1,1,1,4),(311.01767270539,311.070359570927,312.068543993337,
313.066728415748,314.064912838158,314.564005049363,315.063097260568,316.061281682979,
316.560373894184,317.059466105389,317.300858012569),.UNSPECIFIED.);
#1114=B_SPLINE_CURVE_WITH_KNOTS('',3,(#63135,#63136,#63137,#63138,#63139,
#63140,#63141,#63142,#63143,#63144,#63145,#63146,#63147),.UNSPECIFIED.,
 .F.,.F.,(4,1,1,1,1,1,1,1,1,1,4),(311.01767270539,311.250101456171,311.749193667376,
312.747378089787,313.246470300992,313.745562512197,314.244654723402,314.743746934607,
315.741931357018,316.740115779428,317.300858012569),.UNSPECIFIED.);
#1115=B_SPLINE_CURVE_WITH_KNOTS('',3,(#63152,#63153,#63154,#63155,#63156,
#63157,#63158,#63159,#63160,#63161,#63162,#63163,#63164),.UNSPECIFIED.,
 .F.,.F.,(4,1,1,1,1,1,1,1,1,1,4),(304.73448739821,305.081253036465,306.079437458875,
307.077621881286,307.576714092491,308.075806303696,309.073990726106,309.573082937311,
310.072175148517,310.571267359722,311.01767270539),.UNSPECIFIED.);
#1116=B_SPLINE_CURVE_WITH_KNOTS('',3,(#63165,#63166,#63167,#63168,#63169,
#63170,#63171,#63172,#63173,#63174,#63175,#63176,#63177),.UNSPECIFIED.,
 .F.,.F.,(4,1,1,1,1,1,1,1,1,1,4),(304.73448739821,304.761902710504,305.760087132914,
306.259179344119,306.758271555325,307.25736376653,307.756455977735,308.754640400145,
309.752824822556,310.751009244966,311.01767270539),.UNSPECIFIED.);
#1117=B_SPLINE_CURVE_WITH_KNOTS('',3,(#63182,#63183,#63184,#63185,#63186,
#63187,#63188,#63189,#63190,#63191,#63192,#63193,#63194,#63195,#63196,#63197,
#63198,#63199,#63200,#63201,#63202,#63203,#63204,#63205,#63206),
 .UNSPECIFIED.,.F.,.F.,(4,3,3,3,3,3,3,3,4),(298.451302091031,298.97750678823,
299.845671362068,300.713835935906,301.582000509745,302.450165083583,303.318329657421,
304.186494231259,304.73448739821),.UNSPECIFIED.);
#1118=B_SPLINE_CURVE_WITH_KNOTS('',3,(#63207,#63208,#63209,#63210,#63211,
#63212,#63213,#63214,#63215,#63216,#63217,#63218,#63219),.UNSPECIFIED.,
 .F.,.F.,(4,1,1,1,1,1,1,1,1,1,4),(298.451302091031,298.772796176042,299.271888387247,
299.770980598452,300.270072809657,300.769165020862,301.767349443273,302.765533865683,
303.763718288094,304.262810499299,304.73448739821),.UNSPECIFIED.);
#1119=B_SPLINE_CURVE_WITH_KNOTS('',3,(#63224,#63225,#63226,#63227,#63228,
#63229,#63230,#63231,#63232,#63233,#63234,#63235,#63236),.UNSPECIFIED.,
 .F.,.F.,(4,1,1,1,1,1,1,1,1,1,4),(292.168116783851,293.103039967541,293.602132178746,
294.101224389951,295.099408812361,295.598501023566,296.097593234772,296.596685445977,
297.095777657182,298.093962079592,298.451302091031),.UNSPECIFIED.);
#1120=B_SPLINE_CURVE_WITH_KNOTS('',3,(#63237,#63238,#63239,#63240,#63241,
#63242,#63243,#63244,#63245,#63246,#63247,#63248,#63249,#63250,#63251,#63252,
#63253,#63254,#63255,#63256,#63257,#63258,#63259,#63260,#63261),
 .UNSPECIFIED.,.F.,.F.,(4,3,3,3,3,3,3,3,4),(292.168116783851,292.529602224694,
293.397766798532,294.26593137237,295.134095946208,296.002260520046,296.870425093884,
297.738589667722,298.451302091031),.UNSPECIFIED.);
#1121=B_SPLINE_CURVE_WITH_KNOTS('',3,(#63266,#63267,#63268,#63269,#63270,
#63271,#63272,#63273,#63274,#63275,#63276,#63277,#63278,#63279),
 .UNSPECIFIED.,.F.,.F.,(4,1,1,1,1,1,1,1,1,1,1,4),(285.884931476671,286.115749010668,
286.614841221873,287.113933433078,288.112117855489,288.611210066694,289.110302277899,
289.609394489104,290.108486700309,291.10667112272,292.10485554513,292.168116783851),
 .UNSPECIFIED.);
#1122=B_SPLINE_CURVE_WITH_KNOTS('',3,(#63280,#63281,#63282,#63283,#63284,
#63285,#63286,#63287,#63288,#63289,#63290,#63291),.UNSPECIFIED.,.F.,.F.,
(4,1,1,1,1,1,1,1,1,4),(285.884931476671,286.295490895912,286.794583107117,
287.792767529528,288.790951951938,289.789136374348,290.288228585554,290.787320796759,
291.785505219169,292.168116783851),.UNSPECIFIED.);
#1123=B_SPLINE_CURVE_WITH_KNOTS('',3,(#63296,#63297,#63298,#63299,#63300,
#63301,#63302,#63303,#63304,#63305,#63306,#63307,#63308),.UNSPECIFIED.,
 .F.,.F.,(4,1,1,1,1,1,1,1,1,1,4),(279.601746169492,279.627550265001,280.126642476206,
281.124826898616,281.623919109821,282.123011321027,282.622103532232,283.121195743437,
284.119380165847,285.117564588258,285.884931476671),.UNSPECIFIED.);
#1124=B_SPLINE_CURVE_WITH_KNOTS('',3,(#63309,#63310,#63311,#63312,#63313,
#63314,#63315,#63316,#63317,#63318,#63319,#63320,#63321),.UNSPECIFIED.,
 .F.,.F.,(4,1,1,1,1,1,1,1,1,1,4),(279.601746169492,279.807292150245,280.805476572655,
281.803660995066,282.801845417476,283.300937628681,283.800029839886,284.798214262297,
285.297306473502,285.796398684707,285.884931476671),.UNSPECIFIED.);
#1125=B_SPLINE_CURVE_WITH_KNOTS('',3,(#63326,#63327,#63328,#63329,#63330,
#63331,#63332,#63333,#63334,#63335,#63336,#63337,#63338,#63339,#63340,#63341,
#63342,#63343,#63344,#63345,#63346,#63347,#63348,#63349,#63350),
 .UNSPECIFIED.,.F.,.F.,(4,3,3,3,3,3,3,3,4),(273.318560862312,273.800734146925,
274.668898720763,275.537063294602,276.40522786844,277.273392442278,278.141557016116,
279.009721589954,279.601746169492),.UNSPECIFIED.);
#1126=B_SPLINE_CURVE_WITH_KNOTS('',3,(#63351,#63352,#63353,#63354,#63355,
#63356,#63357,#63358,#63359,#63360,#63361,#63362,#63363),.UNSPECIFIED.,
 .F.,.F.,(4,1,1,1,1,1,1,1,1,1,4),(273.318560862312,273.818185615783,274.816370038193,
275.814554460603,276.313646671809,276.812738883014,277.810923305424,278.310015516629,
278.809107727834,279.30819993904,279.601746169492),.UNSPECIFIED.);
#1127=B_SPLINE_CURVE_WITH_KNOTS('',3,(#63368,#63369,#63370,#63371,#63372,
#63373,#63374,#63375,#63376,#63377,#63378,#63379,#63380,#63381,#63382,#63383,
#63384,#63385,#63386,#63387,#63388,#63389,#63390,#63391,#63392),
 .UNSPECIFIED.,.F.,.F.,(4,3,3,3,3,3,3,3,4),(267.035375555133,267.723582130059,
268.591746703897,269.459911277735,270.328075851573,271.196240425411,272.064404999249,
272.932569573087,273.318560862312),.UNSPECIFIED.);
#1128=B_SPLINE_CURVE_WITH_KNOTS('',3,(#63393,#63394,#63395,#63396,#63397,
#63398,#63399,#63400,#63401,#63402,#63403,#63404,#63405,#63406,#63407,#63408,
#63409,#63410,#63411,#63412,#63413,#63414,#63415,#63416,#63417),
 .UNSPECIFIED.,.F.,.F.,(4,3,3,3,3,3,3,3,4),(267.035375555133,267.352829583389,
268.220994157227,269.089158731065,269.957323304903,270.825487878741,271.693652452579,
272.561817026417,273.318560862312),.UNSPECIFIED.);
#1129=B_SPLINE_CURVE_WITH_KNOTS('',3,(#63422,#63423,#63424,#63425,#63426,
#63427,#63428,#63429,#63430,#63431,#63432,#63433),.UNSPECIFIED.,.F.,.F.,
(4,1,1,1,1,1,1,1,1,4),(260.752190247953,261.161138450409,261.660230661614,
262.159322872819,263.15750729523,264.15569171764,265.15387614005,265.652968351256,
266.152060562461,267.035375555133),.UNSPECIFIED.);
#1130=B_SPLINE_CURVE_WITH_KNOTS('',3,(#63434,#63435,#63436,#63437,#63438,
#63439,#63440,#63441,#63442,#63443,#63444,#63445,#63446,#63447),
 .UNSPECIFIED.,.F.,.F.,(4,1,1,1,1,1,1,1,1,1,1,4),(260.752190247953,260.841788124448,
261.839972546858,262.339064758064,262.838156969269,263.836341391679,264.335433602884,
264.834525814089,265.333618025295,265.8327102365,266.83089465891,267.035375555133),
 .UNSPECIFIED.);
#1131=B_SPLINE_CURVE_WITH_KNOTS('',3,(#63452,#63453,#63454,#63455,#63456,
#63457,#63458,#63459,#63460,#63461,#63462,#63463,#63464,#63465,#63466,#63467,
#63468,#63469,#63470,#63471,#63472,#63473,#63474,#63475,#63476),
 .UNSPECIFIED.,.F.,.F.,(4,3,3,3,3,3,3,3,4),(254.469004940774,254.701113522487,
255.569278096325,256.437442670163,257.305607244001,258.17377181784,259.041936391678,
259.910100965516,260.752190247953),.UNSPECIFIED.);
#1132=B_SPLINE_CURVE_WITH_KNOTS('',3,(#63477,#63478,#63479,#63480,#63481,
#63482,#63483,#63484,#63485,#63486,#63487,#63488,#63489),.UNSPECIFIED.,
 .F.,.F.,(4,1,1,1,1,1,1,1,1,1,4),(254.469004940774,254.852681589986,255.351773801191,
255.850866012396,256.849050434807,257.348142646012,257.847234857217,258.346327068422,
258.845419279627,259.843603702038,260.752190247953),.UNSPECIFIED.);
#1133=B_SPLINE_CURVE_WITH_KNOTS('',3,(#63494,#63495,#63496,#63497,#63498,
#63499,#63500,#63501,#63502,#63503,#63504,#63505),.UNSPECIFIED.,.F.,.F.,
(4,1,1,1,1,1,1,1,1,4),(248.185819633594,249.182925381485,250.181109803895,
251.179294226305,251.678386437511,252.177478648716,253.175663071126,253.674755282331,
254.173847493536,254.469004940774),.UNSPECIFIED.);
#1134=B_SPLINE_CURVE_WITH_KNOTS('',3,(#63506,#63507,#63508,#63509,#63510,
#63511,#63512,#63513,#63514,#63515,#63516,#63517,#63518),.UNSPECIFIED.,
 .F.,.F.,(4,1,1,1,1,1,1,1,1,1,4),(248.185819633594,248.364482844319,248.863575055524,
249.861759477934,250.360851689139,250.859943900344,251.35903611155,251.858128322755,
252.856312745165,253.854497167575,254.469004940774),.UNSPECIFIED.);
#1135=B_SPLINE_CURVE_WITH_KNOTS('',3,(#63523,#63524,#63525,#63526,#63527,
#63528,#63529,#63530,#63531,#63532,#63533,#63534,#63535,#63536),
 .UNSPECIFIED.,.F.,.F.,(4,1,1,1,1,1,1,1,1,1,1,4),(241.902634326414,242.195634424612,
243.193818847023,244.192003269433,244.691095480638,245.190187691843,246.188372114254,
246.687464325459,247.186556536664,247.685648747869,248.184740959074,248.185819633594),
 .UNSPECIFIED.);
#1136=B_SPLINE_CURVE_WITH_KNOTS('',3,(#63537,#63538,#63539,#63540,#63541,
#63542,#63543,#63544,#63545,#63546,#63547,#63548),.UNSPECIFIED.,.F.,.F.,
(4,1,1,1,1,1,1,1,1,4),(241.902634326415,242.874468521062,243.373560732267,
243.872652943472,244.371745154677,244.870837365882,245.869021788293,246.867206210703,
247.865390633113,248.185819633594),.UNSPECIFIED.);
#1137=B_SPLINE_CURVE_WITH_KNOTS('',3,(#63553,#63554,#63555,#63556,#63557,
#63558,#63559,#63560,#63561,#63562,#63563,#63564,#63565,#63566,#63567,#63568,
#63569,#63570,#63571,#63572,#63573,#63574,#63575,#63576,#63577),
 .UNSPECIFIED.,.F.,.F.,(4,3,3,3,3,3,3,3,4),(235.619449019235,236.469657471887,
237.337822045725,238.205986619563,239.074151193401,239.942315767239,240.810480341078,
241.678644914916,241.902634326414),.UNSPECIFIED.);
#1138=B_SPLINE_CURVE_WITH_KNOTS('',3,(#63578,#63579,#63580,#63581,#63582,
#63583,#63584,#63585,#63586,#63587,#63588,#63589,#63590,#63591),
 .UNSPECIFIED.,.F.,.F.,(4,1,1,1,1,1,1,1,1,1,1,4),(235.619449019235,235.887177564189,
236.386269775394,236.885361986599,237.384454197805,237.88354640901,238.88173083142,
239.87991525383,240.878099676241,241.377191887446,241.876284098651,241.902634326415),
 .UNSPECIFIED.);
#1139=B_SPLINE_CURVE_WITH_KNOTS('',3,(#63596,#63597,#63598,#63599,#63600,
#63601,#63602,#63603,#63604,#63605,#63606,#63607,#63608),.UNSPECIFIED.,
 .F.,.F.,(4,1,1,1,1,1,1,1,1,1,4),(229.336263712055,230.217421355688,230.716513566893,
231.215605778098,232.213790200509,232.712882411714,233.211974622919,233.711066834124,
234.210159045329,235.20834346774,235.619449019235),.UNSPECIFIED.);
#1140=B_SPLINE_CURVE_WITH_KNOTS('',3,(#63609,#63610,#63611,#63612,#63613,
#63614,#63615,#63616,#63617,#63618,#63619,#63620,#63621,#63622,#63623,#63624,
#63625,#63626,#63627,#63628,#63629,#63630,#63631,#63632,#63633),
 .UNSPECIFIED.,.F.,.F.,(4,3,3,3,3,3,3,3,4),(229.336263712055,230.02175290835,
230.889917482188,231.758082056027,232.626246629865,233.494411203703,234.362575777541,
235.230740351379,235.619449019235),.UNSPECIFIED.);
#1141=B_SPLINE_CURVE_WITH_KNOTS('',3,(#63638,#63639,#63640,#63641,#63642,
#63643,#63644,#63645,#63646,#63647,#63648,#63649,#63650,#63651),
 .UNSPECIFIED.,.F.,.F.,(4,1,1,1,1,1,1,1,1,1,1,4),(223.053078404876,223.230130398815,
223.72922261002,224.228314821226,225.226499243636,225.725591454841,226.224683666046,
226.723775877252,227.222868088457,228.221052510867,229.219236933277,229.336263712055),
 .UNSPECIFIED.);
#1142=B_SPLINE_CURVE_WITH_KNOTS('',3,(#63652,#63653,#63654,#63655,#63656,
#63657,#63658,#63659,#63660,#63661,#63662,#63663),.UNSPECIFIED.,.F.,.F.,
(4,1,1,1,1,1,1,1,1,4),(223.053078404876,223.40987228406,223.908964495265,
224.907148917675,225.905333340085,226.903517762496,227.402609973701,227.901702184906,
228.899886607316,229.336263712055),.UNSPECIFIED.);
#1143=B_SPLINE_CURVE_WITH_KNOTS('',3,(#63668,#63669,#63670,#63671,#63672,
#63673,#63674,#63675,#63676,#63677,#63678,#63679),.UNSPECIFIED.,.F.,.F.,
(4,1,1,1,1,1,1,1,1,4),(216.769893097696,217.241023864353,218.239208286764,
218.738300497969,219.237392709174,219.736484920379,220.235577131584,221.233761553995,
222.231945976405,223.053078404876),.UNSPECIFIED.);
#1144=B_SPLINE_CURVE_WITH_KNOTS('',3,(#63680,#63681,#63682,#63683,#63684,
#63685,#63686,#63687,#63688,#63689,#63690,#63691,#63692),.UNSPECIFIED.,
 .F.,.F.,(4,1,1,1,1,1,1,1,1,1,4),(216.769893097696,216.921673538392,217.919857960803,
218.918042383213,219.916226805623,220.415319016828,220.914411228034,221.912595650444,
222.411687861649,222.910780072854,223.053078404876),.UNSPECIFIED.);
#1145=B_SPLINE_CURVE_WITH_KNOTS('',3,(#63697,#63698,#63699,#63700,#63701,
#63702,#63703,#63704,#63705,#63706,#63707,#63708,#63709,#63710,#63711,#63712,
#63713,#63714,#63715,#63716,#63717,#63718,#63719,#63720,#63721),
 .UNSPECIFIED.,.F.,.F.,(4,3,3,3,3,3,3,3,4),(210.486707790517,211.292884830582,
212.16104940442,213.029213978258,213.897378552096,214.765543125934,215.633707699773,
216.501872273611,216.769893097696),.UNSPECIFIED.);
#1146=B_SPLINE_CURVE_WITH_KNOTS('',3,(#63722,#63723,#63724,#63725,#63726,
#63727,#63728,#63729,#63730,#63731,#63732,#63733,#63734),.UNSPECIFIED.,
 .F.,.F.,(4,1,1,1,1,1,1,1,1,1,4),(210.486707790517,210.93256700393,211.93075142634,
212.928935848751,213.428028059956,213.927120271161,214.925304693571,215.424396904777,
215.923489115982,216.422581327187,216.769893097696),.UNSPECIFIED.);
#1147=B_SPLINE_CURVE_WITH_KNOTS('',3,(#63739,#63740,#63741,#63742,#63743,
#63744,#63745,#63746,#63747,#63748,#63749,#63750,#63751,#63752,#63753,#63754,
#63755,#63756,#63757,#63758,#63759,#63760,#63761,#63762,#63763,#63764,#63765,
#63766),.UNSPECIFIED.,.F.,.F.,(4,3,3,3,3,3,3,3,3,4),(204.203522483337,204.347568239877,
205.215732813715,206.083897387553,206.952061961392,207.82022653523,208.688391109068,
209.556555682906,210.424720256744,210.486707790517),.UNSPECIFIED.);
#1148=B_SPLINE_CURVE_WITH_KNOTS('',3,(#63767,#63768,#63769,#63770,#63771,
#63772,#63773,#63774,#63775,#63776,#63777,#63778,#63779,#63780,#63781,#63782,
#63783,#63784,#63785,#63786,#63787,#63788,#63789,#63790,#63791),
 .UNSPECIFIED.,.F.,.F.,(4,3,3,3,3,3,3,3,4),(204.203522483337,204.844980267045,
205.713144840884,206.581309414722,207.44947398856,208.317638562398,209.185803136236,
210.053967710074,210.486707790517),.UNSPECIFIED.);
#1149=B_SPLINE_CURVE_WITH_KNOTS('',3,(#63796,#63797,#63798,#63799,#63800,
#63801,#63802,#63803,#63804,#63805,#63806),.UNSPECIFIED.,.F.,.F.,(4,1,1,
1,1,1,1,1,4),(197.920337176157,198.275519838556,199.273704260967,200.271888683377,
201.270073105787,202.268257528198,202.767349739403,203.266441950608,204.203522483337),
 .UNSPECIFIED.);
#1150=B_SPLINE_CURVE_WITH_KNOTS('',3,(#63807,#63808,#63809,#63810,#63811,
#63812,#63813,#63814,#63815,#63816,#63817,#63818,#63819,#63820),
 .UNSPECIFIED.,.F.,.F.,(4,1,1,1,1,1,1,1,1,1,1,4),(197.920337176158,197.956169512595,
198.954353935006,199.453446146211,199.952538357416,200.950722779826,201.449814991032,
201.948907202237,202.447999413442,202.947091624647,203.945276047057,204.203522483337),
 .UNSPECIFIED.);
#1151=B_SPLINE_CURVE_WITH_KNOTS('',3,(#63825,#63826,#63827,#63828,#63829,
#63830,#63831,#63832,#63833,#63834,#63835,#63836,#63837),.UNSPECIFIED.,
 .F.,.F.,(4,1,1,1,1,1,1,1,1,1,4),(191.637151868978,191.787321092889,192.286413304094,
192.785505515299,193.284597726505,194.282782148915,194.78187436012,195.280966571325,
196.279150993736,197.277335416146,197.920337176157),.UNSPECIFIED.);
#1152=B_SPLINE_CURVE_WITH_KNOTS('',3,(#63838,#63839,#63840,#63841,#63842,
#63843,#63844,#63845,#63846,#63847),.UNSPECIFIED.,.F.,.F.,(4,1,1,1,1,1,
1,4),(191.637151868978,191.967062978133,192.965247400543,193.963431822954,
194.961616245364,195.959800667775,196.957985090185,197.920337176158),
 .UNSPECIFIED.);
#1153=B_SPLINE_CURVE_WITH_KNOTS('',3,(#63852,#63853,#63854,#63855,#63856,
#63857,#63858,#63859,#63860,#63861,#63862,#63863),.UNSPECIFIED.,.F.,.F.,
(4,1,1,1,1,1,1,1,1,4),(185.353966561798,185.798214558427,186.297306769632,
187.295491192042,187.794583403248,188.293675614453,189.291860036863,190.290044459273,
191.288228881684,191.637151868978),.UNSPECIFIED.);
#1154=B_SPLINE_CURVE_WITH_KNOTS('',3,(#63864,#63865,#63866,#63867,#63868,
#63869,#63870,#63871,#63872,#63873,#63874,#63875,#63876),.UNSPECIFIED.,
 .F.,.F.,(4,1,1,1,1,1,1,1,1,1,4),(185.353966561798,185.977956443671,186.976140866081,
187.974325288492,188.473417499697,188.972509710902,189.471601922107,189.970694133312,
190.968878555723,191.467970766928,191.637151868978),.UNSPECIFIED.);
#1155=B_SPLINE_CURVE_WITH_KNOTS('',3,(#63881,#63882,#63883,#63884,#63885,
#63886,#63887,#63888,#63889,#63890,#63891,#63892,#63893,#63894,#63895,#63896,
#63897,#63898,#63899,#63900,#63901,#63902,#63903,#63904,#63905,#63906,#63907,
#63908),.UNSPECIFIED.,.F.,.F.,(4,3,3,3,3,3,3,3,3,4),(179.070781254619,179.170795598572,
180.03896017241,180.907124746249,181.775289320087,182.643453893925,183.511618467763,
184.379783041601,185.247947615439,185.353966561798),.UNSPECIFIED.);
#1156=B_SPLINE_CURVE_WITH_KNOTS('',3,(#63909,#63910,#63911,#63912,#63913,
#63914,#63915,#63916,#63917,#63918,#63919,#63920,#63921),.UNSPECIFIED.,
 .F.,.F.,(4,1,1,1,1,1,1,1,1,1,4),(179.070781254619,179.988849909209,180.987034331619,
181.486126542824,181.98521875403,182.484310965235,182.98340317644,183.98158759885,
184.480679810055,184.979772021261,185.353966561798),.UNSPECIFIED.);
#1157=B_SPLINE_CURVE_WITH_KNOTS('',3,(#63926,#63927,#63928,#63929,#63930,
#63931,#63932,#63933,#63934,#63935,#63936,#63937,#63938,#63939,#63940,#63941,
#63942,#63943,#63944,#63945,#63946,#63947,#63948,#63949,#63950),
 .UNSPECIFIED.,.F.,.F.,(4,3,3,3,3,3,3,3,4),(172.787595947439,173.093643581706,
173.961808155544,174.829972729382,175.69813730322,176.566301877058,177.434466450896,
178.302631024734,179.070781254619),.UNSPECIFIED.);
#1158=B_SPLINE_CURVE_WITH_KNOTS('',3,(#63951,#63952,#63953,#63954,#63955,
#63956,#63957,#63958,#63959,#63960,#63961,#63962,#63963,#63964),
 .UNSPECIFIED.,.F.,.F.,(4,1,1,1,1,1,1,1,1,1,1,4),(172.787595947439,173.001558952336,
173.999743374747,174.498835585952,174.997927797157,175.497020008362,175.996112219567,
176.994296641978,177.493388853183,177.992481064388,178.990665486798,179.070781254619),
 .UNSPECIFIED.);
#1159=B_SPLINE_CURVE_WITH_KNOTS('',3,(#63969,#63970,#63971,#63972,#63973,
#63974,#63975,#63976,#63977,#63978,#63979,#63980,#63981),.UNSPECIFIED.,
 .F.,.F.,(4,1,1,1,1,1,1,1,1,1,4),(166.50441064026,166.83271053263,167.331802743835,
168.329987166246,169.328171588656,170.326356011066,170.825448222271,171.324540433477,
171.823632644682,172.322724855887,172.787595947439),.UNSPECIFIED.);
#1160=B_SPLINE_CURVE_WITH_KNOTS('',3,(#63982,#63983,#63984,#63985,#63986,
#63987,#63988,#63989,#63990,#63991,#63992,#63993,#63994,#63995,#63996,#63997,
#63998,#63999,#64000,#64001,#64002,#64003,#64004,#64005,#64006,#64007,#64008,
#64009),.UNSPECIFIED.,.F.,.F.,(4,3,3,3,3,3,3,3,3,4),(166.50441064026,166.645739018169,
167.513903592007,168.382068165845,169.250232739683,170.118397313521,170.986561887359,
171.854726461198,172.722891035036,172.787595947439),.UNSPECIFIED.);
#1161=B_SPLINE_CURVE_WITH_KNOTS('',3,(#64014,#64015,#64016,#64017,#64018,
#64019,#64020,#64021,#64022,#64023,#64024,#64025,#64026),.UNSPECIFIED.,
 .F.,.F.,(4,1,1,1,1,1,1,1,1,1,4),(160.22122533308,160.344511786963,161.342696209373,
162.340880631783,163.339065054194,163.838157265399,164.337249476604,164.836341687809,
165.335433899014,166.333618321425,166.50441064026),.UNSPECIFIED.);
#1162=B_SPLINE_CURVE_WITH_KNOTS('',3,(#64027,#64028,#64029,#64030,#64031,
#64032,#64033,#64034,#64035,#64036,#64037,#64038,#64039),.UNSPECIFIED.,
 .F.,.F.,(4,1,1,1,1,1,1,1,1,1,4),(160.22122533308,160.524253672207,161.023345883412,
161.522438094617,162.021530305822,163.019714728233,163.518806939438,164.017899150643,
165.016083573053,166.014267995464,166.50441064026),.UNSPECIFIED.);
#1163=B_SPLINE_CURVE_WITH_KNOTS('',3,(#64044,#64045,#64046,#64047,#64048,
#64049,#64050,#64051,#64052,#64053,#64054,#64055,#64056),.UNSPECIFIED.,
 .F.,.F.,(4,1,1,1,1,1,1,1,1,1,4),(153.938040025901,154.3554052525,155.353589674911,
156.351774097321,156.850866308526,157.349958519732,157.849050730937,158.348142942142,
159.346327364552,159.845419575757,160.22122533308),.UNSPECIFIED.);
#1164=B_SPLINE_CURVE_WITH_KNOTS('',3,(#64057,#64058,#64059,#64060,#64061,
#64062,#64063,#64064,#64065,#64066,#64067,#64068,#64069),.UNSPECIFIED.,
 .F.,.F.,(4,1,1,1,1,1,1,1,1,1,4),(153.938040025901,154.036054926539,154.535147137745,
155.03423934895,156.03242377136,156.531515982565,157.030608193771,158.028792616181,
159.026977038591,160.025161461002,160.22122533308),.UNSPECIFIED.);
#1165=B_SPLINE_CURVE_WITH_KNOTS('',3,(#64074,#64075,#64076,#64077,#64078,
#64079,#64080,#64081,#64082,#64083,#64084,#64085,#64086),.UNSPECIFIED.,
 .F.,.F.,(4,1,1,1,1,1,1,1,1,1,4),(147.654854718721,148.366298718038,149.364483140449,
149.863575351654,150.362667562859,150.861759774064,151.360851985269,152.35903640768,
152.858128618885,153.35722083009,153.938040025901),.UNSPECIFIED.);
#1166=B_SPLINE_CURVE_WITH_KNOTS('',3,(#64087,#64088,#64089,#64090,#64091,
#64092,#64093,#64094,#64095,#64096,#64097,#64098),.UNSPECIFIED.,.F.,.F.,
(4,1,1,1,1,1,1,1,1,4),(147.654854718721,148.046948392077,149.045132814488,
149.544225025693,150.043317236898,151.041501659308,152.039686081719,153.037870504129,
153.536962715334,153.938040025901),.UNSPECIFIED.);
#1167=B_SPLINE_CURVE_WITH_KNOTS('',3,(#64103,#64104,#64105,#64106,#64107,
#64108,#64109,#64110,#64111,#64112,#64113,#64114,#64115,#64116),
 .UNSPECIFIED.,.F.,.F.,(4,1,1,1,1,1,1,1,1,1,1,4),(141.371669411541,141.379007761166,
142.377192183576,142.876284394781,143.375376605987,143.874468817192,144.373561028397,
145.371745450807,145.870837662012,146.369929873218,147.368114295628,147.654854718721),
 .UNSPECIFIED.);
#1168=B_SPLINE_CURVE_WITH_KNOTS('',3,(#64117,#64118,#64119,#64120,#64121,
#64122,#64123,#64124,#64125,#64126,#64127,#64128,#64129,#64130,#64131,#64132,
#64133,#64134,#64135,#64136,#64137,#64138,#64139,#64140,#64141,#64142,#64143,
#64144),.UNSPECIFIED.,.F.,.F.,(4,3,3,3,3,3,3,3,3,4),(141.371669411542,141.468966376864,
142.337130950702,143.20529552454,144.073460098378,144.941624672216,145.809789246055,
146.677953819893,147.546118393731,147.654854718721),.UNSPECIFIED.);
#1169=B_SPLINE_CURVE_WITH_KNOTS('',3,(#64149,#64150,#64151,#64152,#64153,
#64154,#64155,#64156,#64157,#64158,#64159,#64160,#64161),.UNSPECIFIED.,
 .F.,.F.,(4,1,1,1,1,1,1,1,1,1,4),(135.088484104362,135.389901226704,135.888993437909,
136.388085649114,136.887177860319,137.386270071524,138.384454493935,138.88354670514,
139.382638916345,140.380823338755,141.371669411541),.UNSPECIFIED.);
#1170=B_SPLINE_CURVE_WITH_KNOTS('',3,(#64162,#64163,#64164,#64165,#64166,
#64167,#64168,#64169,#64170,#64171,#64172,#64173,#64174),.UNSPECIFIED.,
 .F.,.F.,(4,1,1,1,1,1,1,1,1,1,4),(135.088484104362,135.569643111948,136.068735323153,
137.066919745563,138.065104167974,139.063288590384,139.562380801589,140.061473012794,
140.560565224,141.059657435205,141.371669411542),.UNSPECIFIED.);
#1171=B_SPLINE_CURVE_WITH_KNOTS('',3,(#64179,#64180,#64181,#64182,#64183,
#64184,#64185,#64186,#64187,#64188,#64189,#64190,#64191),.UNSPECIFIED.,
 .F.,.F.,(4,1,1,1,1,1,1,1,1,1,4),(128.805298797182,128.901702481036,129.400794692241,
129.899886903447,130.398979114652,131.397163537062,131.896255748267,132.395347959473,
133.393532381883,134.391716804293,135.088484104362),.UNSPECIFIED.);
#1172=B_SPLINE_CURVE_WITH_KNOTS('',3,(#64192,#64193,#64194,#64195,#64196,
#64197,#64198,#64199,#64200,#64201,#64202,#64203,#64204),.UNSPECIFIED.,
 .F.,.F.,(4,1,1,1,1,1,1,1,1,1,4),(128.805298797182,129.08144436628,130.079628788691,
131.077813211101,132.075997633511,132.575089844717,133.074182055922,133.573274267127,
134.072366478332,135.070550900743,135.088484104362),.UNSPECIFIED.);
#1173=B_SPLINE_CURVE_WITH_KNOTS('',3,(#64209,#64210,#64211,#64212,#64213,
#64214,#64215,#64216,#64217,#64218,#64219,#64220),.UNSPECIFIED.,.F.,.F.,
(4,1,1,1,1,1,1,1,1,4),(122.522113490003,122.912595946574,123.411688157779,
124.40987258019,124.908964791395,125.4080570026,126.40624142501,127.404425847421,
128.402610269831,128.805298797182),.UNSPECIFIED.);
#1174=B_SPLINE_CURVE_WITH_KNOTS('',3,(#64221,#64222,#64223,#64224,#64225,
#64226,#64227,#64228,#64229,#64230,#64231,#64232,#64233),.UNSPECIFIED.,
 .F.,.F.,(4,1,1,1,1,1,1,1,1,1,4),(122.522113490003,123.092337831818,124.090522254229,
125.088706676639,125.587798887844,126.086891099049,126.585983310255,127.08507552146,
128.08325994387,128.582352155075,128.805298797182),.UNSPECIFIED.);
#1175=B_SPLINE_CURVE_WITH_KNOTS('',3,(#64238,#64239,#64240,#64241,#64242,
#64243,#64244,#64245,#64246,#64247,#64248,#64249,#64250,#64251,#64252,#64253,
#64254,#64255,#64256,#64257,#64258,#64259,#64260,#64261,#64262),
 .UNSPECIFIED.,.F.,.F.,(4,3,3,3,3,3,3,3,4),(116.238928182823,116.662946282229,
117.531110856067,118.399275429905,119.267440003743,120.135604577582,121.00376915142,
121.871933725258,122.522113490003),.UNSPECIFIED.);
#1176=B_SPLINE_CURVE_WITH_KNOTS('',3,(#64263,#64264,#64265,#64266,#64267,
#64268,#64269,#64270,#64271,#64272,#64273,#64274,#64275),.UNSPECIFIED.,
 .F.,.F.,(4,1,1,1,1,1,1,1,1,1,4),(116.238928182823,117.103231297356,118.101415719766,
118.600507930972,119.099600142177,119.598692353382,120.097784564587,121.095968986998,
121.595061198203,122.094153409408,122.522113490003),.UNSPECIFIED.);
#1177=B_SPLINE_CURVE_WITH_KNOTS('',3,(#64280,#64281,#64282,#64283,#64284,
#64285,#64286,#64287,#64288,#64289,#64290,#64291,#64292,#64293,#64294,#64295,
#64296,#64297,#64298,#64299,#64300,#64301,#64302,#64303,#64304),
 .UNSPECIFIED.,.F.,.F.,(4,3,3,3,3,3,3,3,4),(109.955742875643,110.585794265362,
111.453958839201,112.322123413039,113.190287986877,114.058452560715,114.926617134553,
115.794781708391,116.238928182823),.UNSPECIFIED.);
#1178=B_SPLINE_CURVE_WITH_KNOTS('',3,(#64305,#64306,#64307,#64308,#64309,
#64310,#64311,#64312,#64313,#64314,#64315,#64316,#64317,#64318),
 .UNSPECIFIED.,.F.,.F.,(4,1,1,1,1,1,1,1,1,1,1,4),(109.955742875644,110.115940340484,
111.114124762894,111.613216974099,112.112309185304,112.611401396509,113.110493607715,
114.108678030125,114.60777024133,115.106862452535,116.105046874946,116.238928182823),
 .UNSPECIFIED.);
#1179=B_SPLINE_CURVE_WITH_KNOTS('',3,(#64323,#64324,#64325,#64326,#64327,
#64328,#64329,#64330,#64331,#64332,#64333,#64334,#64335,#64336,#64337,#64338,
#64339,#64340,#64341,#64342,#64343,#64344,#64345,#64346,#64347),
 .UNSPECIFIED.,.F.,.F.,(4,3,3,3,3,3,3,3,4),(103.672557568464,104.508642248496,
105.376806822334,106.244971396172,107.11313597001,107.981300543848,108.849465117686,
109.717629691524,109.955742875643),.UNSPECIFIED.);
#1180=B_SPLINE_CURVE_WITH_KNOTS('',3,(#64348,#64349,#64350,#64351,#64352,
#64353,#64354,#64355,#64356,#64357,#64358,#64359,#64360),.UNSPECIFIED.,
 .F.,.F.,(4,1,1,1,1,1,1,1,1,1,4),(103.672557568464,104.126833806021,104.625926017227,
105.125018228432,105.624110439637,106.123202650842,107.121387073252,107.620479284458,
108.119571495663,109.117755918073,109.955742875644),.UNSPECIFIED.);
#1181=B_SPLINE_CURVE_WITH_KNOTS('',3,(#64365,#64366,#64367,#64368,#64369,
#64370,#64371,#64372,#64373,#64374,#64375,#64376,#64377),.UNSPECIFIED.,
 .F.,.F.,(4,1,1,1,1,1,1,1,1,1,4),(97.3893722612843,97.4588931751099,98.4570775975203,
99.4552620199306,100.453446442341,100.952538653546,101.451630864751,101.950723075957,
102.449815287162,103.447999709572,103.672557568464),.UNSPECIFIED.);
#1182=B_SPLINE_CURVE_WITH_KNOTS('',3,(#64378,#64379,#64380,#64381,#64382,
#64383,#64384,#64385,#64386,#64387,#64388,#64389,#64390),.UNSPECIFIED.,
 .F.,.F.,(4,1,1,1,1,1,1,1,1,1,4),(97.3893722612844,97.638635060354,98.1377272715592,
98.6368194827644,99.1359116939696,100.13409611638,100.633188327585,101.13228053879,
102.130464961201,103.128649383611,103.672557568464),.UNSPECIFIED.);
#1183=B_SPLINE_CURVE_WITH_KNOTS('',3,(#64395,#64396,#64397,#64398,#64399,
#64400,#64401,#64402,#64403,#64404,#64405,#64406,#64407),.UNSPECIFIED.,
 .F.,.F.,(4,1,1,1,1,1,1,1,1,1,4),(91.1061869541047,91.4697866406478,92.4679710630581,
93.4661554854685,93.9652476966737,94.4643399078788,94.963432119084,95.4625243302892,
96.4607087526996,96.9598009639047,97.3893722612843),.UNSPECIFIED.);
#1184=B_SPLINE_CURVE_WITH_KNOTS('',3,(#64408,#64409,#64410,#64411,#64412,
#64413,#64414,#64415,#64416,#64417,#64418,#64419,#64420),.UNSPECIFIED.,
 .F.,.F.,(4,1,1,1,1,1,1,1,1,1,4),(91.1061869541048,91.1504363146867,91.6495285258919,
92.1486207370971,93.1468051595074,93.6458973707126,94.1449895819178,95.1431740043281,
96.1413584267385,97.1395428491489,97.3893722612844),.UNSPECIFIED.);
#1185=B_SPLINE_CURVE_WITH_KNOTS('',3,(#64425,#64426,#64427,#64428,#64429,
#64430,#64431,#64432,#64433,#64434,#64435,#64436,#64437),.UNSPECIFIED.,
 .F.,.F.,(4,1,1,1,1,1,1,1,1,1,4),(84.8230016469251,85.4806801061856,86.4788645285959,
86.9779567398011,87.4770489510063,87.9761411622115,88.4752333734167,89.473417795827,
89.9725100070322,90.4716022182374,91.1061869541047),.UNSPECIFIED.);
#1186=B_SPLINE_CURVE_WITH_KNOTS('',3,(#64438,#64439,#64440,#64441,#64442,
#64443,#64444,#64445,#64446,#64447,#64448,#64449),.UNSPECIFIED.,.F.,.F.,
(4,1,1,1,1,1,1,1,1,4),(84.8230016469252,85.1613297802245,86.1595142026349,
86.6586064138401,87.1576986250453,88.1558830474556,89.154067469866,90.1522518922763,
90.6513441034815,91.1061869541048),.UNSPECIFIED.);
#1187=B_SPLINE_CURVE_WITH_KNOTS('',3,(#64454,#64455,#64456,#64457,#64458,
#64459,#64460,#64461,#64462,#64463,#64464,#64465,#64466),.UNSPECIFIED.,
 .F.,.F.,(4,1,1,1,1,1,1,1,1,1,4),(78.5398163397456,79.4915735717234,79.9906657829286,
80.4897579941338,80.988850205339,81.4879424165442,82.4861268389545,82.9852190501597,
83.4843112613649,84.4824956837752,84.8230016469251),.UNSPECIFIED.);
#1188=B_SPLINE_CURVE_WITH_KNOTS('',3,(#64467,#64468,#64469,#64470,#64471,
#64472,#64473,#64474,#64475,#64476,#64477,#64478,#64479,#64480,#64481,#64482,
#64483,#64484,#64485,#64486,#64487,#64488,#64489,#64490,#64491),
 .UNSPECIFIED.,.F.,.F.,(4,3,3,3,3,3,3,3,4),(78.5398163397456,78.9611170605208,
79.8292816343589,80.697446208197,81.5656107820351,82.4337753558732,83.3019399297113,
84.1701045035494,84.8230016469252),.UNSPECIFIED.);
#1189=B_SPLINE_CURVE_WITH_KNOTS('',3,(#64496,#64497,#64498,#64499,#64500,
#64501,#64502,#64503,#64504,#64505,#64506,#64507,#64508,#64509),
 .UNSPECIFIED.,.F.,.F.,(4,1,1,1,1,1,1,1,1,1,1,4),(72.2566310325659,72.5042826148509,
73.0033748260561,73.5024670372613,74.0015592484665,74.5006514596716,75.498835882082,
75.9979280932872,76.4970203044924,77.4952047269027,78.4933891493131,78.5398163397456),
 .UNSPECIFIED.);
#1190=B_SPLINE_CURVE_WITH_KNOTS('',3,(#64510,#64511,#64512,#64513,#64514,
#64515,#64516,#64517,#64518,#64519,#64520,#64521,#64522),.UNSPECIFIED.,
 .F.,.F.,(4,1,1,1,1,1,1,1,1,1,4),(72.256631032566,72.684024500095,73.1831167113002,
74.1813011337106,75.1794855561209,76.1776699785313,76.6767621897365,77.1758544009417,
77.6749466121468,78.174038823352,78.5398163397456),.UNSPECIFIED.);
#1191=B_SPLINE_CURVE_WITH_KNOTS('',3,(#64527,#64528,#64529,#64530,#64531,
#64532,#64533,#64534,#64535,#64536,#64537,#64538,#64539),.UNSPECIFIED.,
 .F.,.F.,(4,1,1,1,1,1,1,1,1,1,4),(65.9734457253863,66.0160838691836,66.5151760803888,
67.0142682915939,67.5133605027991,68.5115449252095,69.0106371364147,69.5097293476198,
70.5079137700302,71.5060981924406,72.2566310325659),.UNSPECIFIED.);
#1192=B_SPLINE_CURVE_WITH_KNOTS('',3,(#64540,#64541,#64542,#64543,#64544,
#64545,#64546,#64547,#64548,#64549,#64550,#64551,#64552),.UNSPECIFIED.,
 .F.,.F.,(4,1,1,1,1,1,1,1,1,1,4),(65.9734457253865,66.1958257544277,67.194010176838,
68.1921945992484,69.1903790216588,69.689471232864,70.1885634440691,70.6876556552743,
71.1867478664795,72.1849322888899,72.256631032566),.UNSPECIFIED.);
#1193=B_SPLINE_CURVE_WITH_KNOTS('',3,(#64557,#64558,#64559,#64560,#64561,
#64562,#64563,#64564,#64565,#64566,#64567,#64568,#64569,#64570,#64571,#64572,
#64573,#64574,#64575,#64576,#64577,#64578,#64579,#64580,#64581),
 .UNSPECIFIED.,.F.,.F.,(4,3,3,3,3,3,3,3,4),(59.6902604182067,60.2322489827526,
61.1004135565907,61.9685781304288,62.8367427042669,63.704907278105,64.5730718519431,
65.4412364257812,65.9734457253863),.UNSPECIFIED.);
#1194=B_SPLINE_CURVE_WITH_KNOTS('',3,(#64582,#64583,#64584,#64585,#64586,
#64587,#64588,#64589,#64590,#64591,#64592,#64593,#64594),.UNSPECIFIED.,
 .F.,.F.,(4,1,1,1,1,1,1,1,1,1,4),(59.6902604182069,60.2067192199655,61.2049036423759,
62.2030880647862,62.7021802759914,63.2012724871966,63.7003646984018,64.199456909607,
65.1976413320173,65.6967335432225,65.9734457253865),.UNSPECIFIED.);
#1195=B_SPLINE_CURVE_WITH_KNOTS('',3,(#64599,#64600,#64601,#64602,#64603,
#64604,#64605,#64606,#64607,#64608,#64609,#64610,#64611,#64612,#64613,#64614,
#64615,#64616,#64617,#64618,#64619,#64620,#64621,#64622,#64623),
 .UNSPECIFIED.,.F.,.F.,(4,3,3,3,3,3,3,3,4),(53.4070751110271,54.1550969658859,
55.023261539724,55.8914261135621,56.7595906874002,57.6277552612383,58.4959198350764,
59.3640844089145,59.6902604182067),.UNSPECIFIED.);
#1196=B_SPLINE_CURVE_WITH_KNOTS('',3,(#64624,#64625,#64626,#64627,#64628,
#64629,#64630,#64631,#64632,#64633,#64634,#64635,#64636),.UNSPECIFIED.,
 .F.,.F.,(4,1,1,1,1,1,1,1,1,1,4),(53.4070751110272,54.2176126855034,55.2157971079137,
55.7148893191189,56.2139815303241,56.7130737415293,57.2121659527344,58.2103503751448,
58.70944258635,59.2085347975552,59.6902604182069),.UNSPECIFIED.);
#1197=B_SPLINE_CURVE_WITH_KNOTS('',3,(#64641,#64642,#64643,#64644,#64645,
#64646,#64647,#64648,#64649,#64650,#64651,#64652,#64653),.UNSPECIFIED.,
 .F.,.F.,(4,1,1,1,1,1,1,1,1,1,4),(47.1238898038476,47.5496720545919,48.0487642657971,
48.5478564770023,49.5460408994126,50.544225321823,51.5424097442334,52.0415019554385,
52.5405941666437,53.0396863778489,53.4070751110271),.UNSPECIFIED.);
#1198=B_SPLINE_CURVE_WITH_KNOTS('',3,(#64654,#64655,#64656,#64657,#64658,
#64659,#64660,#64661,#64662,#64663,#64664,#64665,#64666,#64667),
 .UNSPECIFIED.,.F.,.F.,(4,1,1,1,1,1,1,1,1,1,1,4),(47.1238898038477,47.2303217286308,
48.2285061510412,48.7275983622464,49.2266905734515,49.7257827846567,50.2248749958619,
51.2230594182723,51.7221516294775,52.2212438406826,53.219428263093,53.4070751110272),
 .UNSPECIFIED.);
#1199=B_SPLINE_CURVE_WITH_KNOTS('',3,(#64672,#64673,#64674,#64675,#64676,
#64677,#64678,#64679,#64680,#64681,#64682,#64683,#64684,#64685,#64686,#64687,
#64688,#64689,#64690,#64691,#64692,#64693,#64694,#64695,#64696),
 .UNSPECIFIED.,.F.,.F.,(4,3,3,3,3,3,3,3,4),(40.8407044966679,41.1326283583144,
42.0007929321525,42.8689575059906,43.7371220798287,44.6052866536668,45.4734512275049,
46.341615801343,47.1238898038476),.UNSPECIFIED.);
#1200=B_SPLINE_CURVE_WITH_KNOTS('',3,(#64697,#64698,#64699,#64700,#64701,
#64702,#64703,#64704,#64705,#64706,#64707,#64708,#64709),.UNSPECIFIED.,
 .F.,.F.,(4,1,1,1,1,1,1,1,1,1,4),(40.8407044966681,41.2412151941687,41.7403074053738,
42.239399616579,42.7384918277842,43.2375840389894,44.2357684613998,44.7348606726049,
45.2339528838101,46.2321373062205,47.1238898038477),.UNSPECIFIED.);
#1201=B_SPLINE_CURVE_WITH_KNOTS('',3,(#64714,#64715,#64716,#64717,#64718,
#64719,#64720,#64721,#64722,#64723,#64724,#64725,#64726),.UNSPECIFIED.,
 .F.,.F.,(4,1,1,1,1,1,1,1,1,1,4),(34.5575191894884,34.5732745632572,35.5714589856676,
36.569643408078,37.5678278304883,38.0669200416935,38.5660122528987,39.0651044641039,
39.564196675309,40.5623810977194,40.8407044966679),.UNSPECIFIED.);
#1202=B_SPLINE_CURVE_WITH_KNOTS('',3,(#64727,#64728,#64729,#64730,#64731,
#64732,#64733,#64734,#64735,#64736,#64737,#64738,#64739),.UNSPECIFIED.,
 .F.,.F.,(4,1,1,1,1,1,1,1,1,1,4),(34.5575191894885,34.7530164485013,35.2521086597065,
35.7512008709117,36.2502930821169,37.2484775045272,37.7475697157324,38.2466619269376,
39.2448463493479,40.2430307717583,40.8407044966681),.UNSPECIFIED.);
#1203=B_SPLINE_CURVE_WITH_KNOTS('',3,(#64744,#64745,#64746,#64747,#64748,
#64749,#64750,#64751,#64752,#64753,#64754,#64755,#64756),.UNSPECIFIED.,
 .F.,.F.,(4,1,1,1,1,1,1,1,1,1,4),(28.2743338823088,28.5841680287951,29.5823524512054,
30.5805368736158,31.079629084821,31.5787212960261,32.0778135072313,32.5769057184365,
33.5750901408469,34.074182352052,34.5575191894884),.UNSPECIFIED.);
#1204=B_SPLINE_CURVE_WITH_KNOTS('',3,(#64757,#64758,#64759,#64760,#64761,
#64762,#64763,#64764,#64765,#64766,#64767,#64768),.UNSPECIFIED.,.F.,.F.,
(4,1,1,1,1,1,1,1,1,4),(28.2743338823089,28.7639099140392,29.2630021252443,
30.2611865476547,30.7602787588599,31.2593709700651,32.2575553924754,33.2557398148858,
34.2539242372961,34.5575191894885),.UNSPECIFIED.);
#1205=B_SPLINE_CURVE_WITH_KNOTS('',3,(#64773,#64774,#64775,#64776,#64777,
#64778,#64779,#64780,#64781,#64782,#64783,#64784,#64785),.UNSPECIFIED.,
 .F.,.F.,(4,1,1,1,1,1,1,1,1,1,4),(21.9911485751292,22.5950614943329,23.5932459167433,
24.0923381279484,24.5914303391536,25.0905225503588,25.589614761564,26.5877991839743,
27.0868913951795,27.5859836063847,28.2743338823088),.UNSPECIFIED.);
#1206=B_SPLINE_CURVE_WITH_KNOTS('',3,(#64786,#64787,#64788,#64789,#64790,
#64791,#64792,#64793,#64794,#64795,#64796,#64797,#64798),.UNSPECIFIED.,
 .F.,.F.,(4,1,1,1,1,1,1,1,1,1,4),(21.9911485751293,22.2757111683718,23.2738955907822,
23.7729878019874,24.2720800131925,25.2702644356029,26.2684488580133,27.2666332804236,
27.7657254916288,28.264817702834,28.2743338823089),.UNSPECIFIED.);
#1207=B_SPLINE_CURVE_WITH_KNOTS('',3,(#64803,#64804,#64805,#64806,#64807,
#64808,#64809,#64810,#64811,#64812,#64813,#64814,#64815),.UNSPECIFIED.,
 .F.,.F.,(4,1,1,1,1,1,1,1,1,1,4),(15.7079632679496,16.6059549598707,17.1050471710759,
17.6041393822811,18.1032315934863,18.6023238046915,19.6005082271018,20.099600438307,
20.5986926495122,21.5968770719225,21.9911485751292),.UNSPECIFIED.);
#1208=B_SPLINE_CURVE_WITH_KNOTS('',3,(#64816,#64817,#64818,#64819,#64820,
#64821,#64822,#64823,#64824,#64825,#64826,#64827,#64828,#64829,#64830,#64831,
#64832,#64833,#64834,#64835,#64836,#64837,#64838,#64839,#64840),
 .UNSPECIFIED.,.F.,.F.,(4,3,3,3,3,3,3,3,4),(15.7079632679497,16.4532677441776,
17.3214323180157,18.1895968918538,19.0577614656919,19.92592603953,20.7940906133681,
21.6622551872062,21.9911485751293),.UNSPECIFIED.);
#1209=B_SPLINE_CURVE_WITH_KNOTS('',2,(#64849,#64850,#64851),
 .UNSPECIFIED.,.F.,.F.,(3,3),(0.,1.),.UNSPECIFIED.);
#1210=B_SPLINE_CURVE_WITH_KNOTS('',2,(#64855,#64856,#64857),
 .UNSPECIFIED.,.F.,.F.,(3,3),(0.,1.),.UNSPECIFIED.);
#1211=B_SPLINE_CURVE_WITH_KNOTS('',2,(#64866,#64867,#64868),
 .UNSPECIFIED.,.F.,.F.,(3,3),(0.,1.),.UNSPECIFIED.);
#1212=B_SPLINE_CURVE_WITH_KNOTS('',2,(#64871,#64872,#64873),
 .UNSPECIFIED.,.F.,.F.,(3,3),(0.,1.),.UNSPECIFIED.);
#1213=B_SPLINE_CURVE_WITH_KNOTS('',2,(#64881,#64882,#64883),
 .UNSPECIFIED.,.F.,.F.,(3,3),(0.,1.),.UNSPECIFIED.);
#1214=B_SPLINE_CURVE_WITH_KNOTS('',2,(#64886,#64887,#64888),
 .UNSPECIFIED.,.F.,.F.,(3,3),(0.,1.),.UNSPECIFIED.);
#1215=B_SPLINE_CURVE_WITH_KNOTS('',2,(#64896,#64897,#64898),
 .UNSPECIFIED.,.F.,.F.,(3,3),(0.,1.),.UNSPECIFIED.);
#1216=B_SPLINE_CURVE_WITH_KNOTS('',2,(#64901,#64902,#64903),
 .UNSPECIFIED.,.F.,.F.,(3,3),(0.,1.),.UNSPECIFIED.);
#1217=B_SPLINE_CURVE_WITH_KNOTS('',2,(#64911,#64912,#64913),
 .UNSPECIFIED.,.F.,.F.,(3,3),(0.,1.),.UNSPECIFIED.);
#1218=B_SPLINE_CURVE_WITH_KNOTS('',2,(#64916,#64917,#64918),
 .UNSPECIFIED.,.F.,.F.,(3,3),(0.,1.),.UNSPECIFIED.);
#1219=B_SPLINE_CURVE_WITH_KNOTS('',2,(#64926,#64927,#64928),
 .UNSPECIFIED.,.F.,.F.,(3,3),(0.,1.),.UNSPECIFIED.);
#1220=B_SPLINE_CURVE_WITH_KNOTS('',2,(#64931,#64932,#64933),
 .UNSPECIFIED.,.F.,.F.,(3,3),(0.,1.),.UNSPECIFIED.);
#1221=B_SPLINE_CURVE_WITH_KNOTS('',2,(#64941,#64942,#64943),
 .UNSPECIFIED.,.F.,.F.,(3,3),(0.,1.),.UNSPECIFIED.);
#1222=B_SPLINE_CURVE_WITH_KNOTS('',2,(#64946,#64947,#64948),
 .UNSPECIFIED.,.F.,.F.,(3,3),(0.,1.),.UNSPECIFIED.);
#1223=B_SPLINE_CURVE_WITH_KNOTS('',2,(#64956,#64957,#64958),
 .UNSPECIFIED.,.F.,.F.,(3,3),(0.,1.),.UNSPECIFIED.);
#1224=B_SPLINE_CURVE_WITH_KNOTS('',2,(#64961,#64962,#64963),
 .UNSPECIFIED.,.F.,.F.,(3,3),(0.,1.),.UNSPECIFIED.);
#1225=B_SPLINE_CURVE_WITH_KNOTS('',2,(#64970,#64971,#64972),
 .UNSPECIFIED.,.F.,.F.,(3,3),(0.,1.),.UNSPECIFIED.);
#1226=B_SPLINE_CURVE_WITH_KNOTS('',2,(#64973,#64974,#64975),
 .UNSPECIFIED.,.F.,.F.,(3,3),(0.,1.),.UNSPECIFIED.);
#1227=B_SPLINE_CURVE_WITH_KNOTS('',2,(#64984,#64985,#64986),
 .UNSPECIFIED.,.F.,.F.,(3,3),(0.,1.),.UNSPECIFIED.);
#1228=B_SPLINE_CURVE_WITH_KNOTS('',2,(#64990,#64991,#64992),
 .UNSPECIFIED.,.F.,.F.,(3,3),(0.,1.),.UNSPECIFIED.);
#1229=B_SPLINE_CURVE_WITH_KNOTS('',2,(#65001,#65002,#65003),
 .UNSPECIFIED.,.F.,.F.,(3,3),(0.,1.),.UNSPECIFIED.);
#1230=B_SPLINE_CURVE_WITH_KNOTS('',2,(#65006,#65007,#65008),
 .UNSPECIFIED.,.F.,.F.,(3,3),(0.,1.),.UNSPECIFIED.);
#1231=B_SPLINE_CURVE_WITH_KNOTS('',2,(#65016,#65017,#65018),
 .UNSPECIFIED.,.F.,.F.,(3,3),(0.,1.),.UNSPECIFIED.);
#1232=B_SPLINE_CURVE_WITH_KNOTS('',2,(#65021,#65022,#65023),
 .UNSPECIFIED.,.F.,.F.,(3,3),(0.,1.),.UNSPECIFIED.);
#1233=B_SPLINE_CURVE_WITH_KNOTS('',2,(#65031,#65032,#65033),
 .UNSPECIFIED.,.F.,.F.,(3,3),(0.,1.),.UNSPECIFIED.);
#1234=B_SPLINE_CURVE_WITH_KNOTS('',2,(#65036,#65037,#65038),
 .UNSPECIFIED.,.F.,.F.,(3,3),(0.,1.),.UNSPECIFIED.);
#1235=B_SPLINE_CURVE_WITH_KNOTS('',2,(#65046,#65047,#65048),
 .UNSPECIFIED.,.F.,.F.,(3,3),(0.,1.),.UNSPECIFIED.);
#1236=B_SPLINE_CURVE_WITH_KNOTS('',2,(#65051,#65052,#65053),
 .UNSPECIFIED.,.F.,.F.,(3,3),(0.,1.),.UNSPECIFIED.);
#1237=B_SPLINE_CURVE_WITH_KNOTS('',2,(#65061,#65062,#65063),
 .UNSPECIFIED.,.F.,.F.,(3,3),(0.,1.),.UNSPECIFIED.);
#1238=B_SPLINE_CURVE_WITH_KNOTS('',2,(#65066,#65067,#65068),
 .UNSPECIFIED.,.F.,.F.,(3,3),(0.,1.),.UNSPECIFIED.);
#1239=B_SPLINE_CURVE_WITH_KNOTS('',2,(#65076,#65077,#65078),
 .UNSPECIFIED.,.F.,.F.,(3,3),(0.,1.),.UNSPECIFIED.);
#1240=B_SPLINE_CURVE_WITH_KNOTS('',2,(#65081,#65082,#65083),
 .UNSPECIFIED.,.F.,.F.,(3,3),(0.,1.),.UNSPECIFIED.);
#1241=B_SPLINE_CURVE_WITH_KNOTS('',2,(#65090,#65091,#65092),
 .UNSPECIFIED.,.F.,.F.,(3,3),(0.,1.),.UNSPECIFIED.);
#1242=B_SPLINE_CURVE_WITH_KNOTS('',2,(#65093,#65094,#65095),
 .UNSPECIFIED.,.F.,.F.,(3,3),(0.,1.),.UNSPECIFIED.);
#1243=B_SPLINE_CURVE_WITH_KNOTS('',2,(#65104,#65105,#65106),
 .UNSPECIFIED.,.F.,.F.,(3,3),(0.,1.),.UNSPECIFIED.);
#1244=B_SPLINE_CURVE_WITH_KNOTS('',2,(#65110,#65111,#65112),
 .UNSPECIFIED.,.F.,.F.,(3,3),(0.,1.),.UNSPECIFIED.);
#1245=B_SPLINE_CURVE_WITH_KNOTS('',2,(#65121,#65122,#65123),
 .UNSPECIFIED.,.F.,.F.,(3,3),(0.,1.),.UNSPECIFIED.);
#1246=B_SPLINE_CURVE_WITH_KNOTS('',2,(#65126,#65127,#65128),
 .UNSPECIFIED.,.F.,.F.,(3,3),(0.,1.),.UNSPECIFIED.);
#1247=B_SPLINE_CURVE_WITH_KNOTS('',2,(#65136,#65137,#65138),
 .UNSPECIFIED.,.F.,.F.,(3,3),(0.,1.),.UNSPECIFIED.);
#1248=B_SPLINE_CURVE_WITH_KNOTS('',2,(#65141,#65142,#65143),
 .UNSPECIFIED.,.F.,.F.,(3,3),(0.,1.),.UNSPECIFIED.);
#1249=B_SPLINE_CURVE_WITH_KNOTS('',2,(#65151,#65152,#65153),
 .UNSPECIFIED.,.F.,.F.,(3,3),(0.,1.),.UNSPECIFIED.);
#1250=B_SPLINE_CURVE_WITH_KNOTS('',2,(#65156,#65157,#65158),
 .UNSPECIFIED.,.F.,.F.,(3,3),(0.,1.),.UNSPECIFIED.);
#1251=B_SPLINE_CURVE_WITH_KNOTS('',2,(#65166,#65167,#65168),
 .UNSPECIFIED.,.F.,.F.,(3,3),(0.,1.),.UNSPECIFIED.);
#1252=B_SPLINE_CURVE_WITH_KNOTS('',2,(#65171,#65172,#65173),
 .UNSPECIFIED.,.F.,.F.,(3,3),(0.,1.),.UNSPECIFIED.);
#1253=B_SPLINE_CURVE_WITH_KNOTS('',2,(#65181,#65182,#65183),
 .UNSPECIFIED.,.F.,.F.,(3,3),(0.,1.),.UNSPECIFIED.);
#1254=B_SPLINE_CURVE_WITH_KNOTS('',2,(#65186,#65187,#65188),
 .UNSPECIFIED.,.F.,.F.,(3,3),(0.,1.),.UNSPECIFIED.);
#1255=B_SPLINE_CURVE_WITH_KNOTS('',2,(#65196,#65197,#65198),
 .UNSPECIFIED.,.F.,.F.,(3,3),(0.,1.),.UNSPECIFIED.);
#1256=B_SPLINE_CURVE_WITH_KNOTS('',2,(#65201,#65202,#65203),
 .UNSPECIFIED.,.F.,.F.,(3,3),(0.,1.),.UNSPECIFIED.);
#1257=B_SPLINE_CURVE_WITH_KNOTS('',2,(#65211,#65212,#65213),
 .UNSPECIFIED.,.F.,.F.,(3,3),(0.,1.),.UNSPECIFIED.);
#1258=B_SPLINE_CURVE_WITH_KNOTS('',2,(#65216,#65217,#65218),
 .UNSPECIFIED.,.F.,.F.,(3,3),(0.,1.),.UNSPECIFIED.);
#1259=B_SPLINE_CURVE_WITH_KNOTS('',2,(#65226,#65227,#65228),
 .UNSPECIFIED.,.F.,.F.,(3,3),(0.,1.),.UNSPECIFIED.);
#1260=B_SPLINE_CURVE_WITH_KNOTS('',2,(#65231,#65232,#65233),
 .UNSPECIFIED.,.F.,.F.,(3,3),(0.,1.),.UNSPECIFIED.);
#1261=B_SPLINE_CURVE_WITH_KNOTS('',2,(#65241,#65242,#65243),
 .UNSPECIFIED.,.F.,.F.,(3,3),(0.,1.),.UNSPECIFIED.);
#1262=B_SPLINE_CURVE_WITH_KNOTS('',2,(#65246,#65247,#65248),
 .UNSPECIFIED.,.F.,.F.,(3,3),(0.,1.),.UNSPECIFIED.);
#1263=B_SPLINE_CURVE_WITH_KNOTS('',2,(#65256,#65257,#65258),
 .UNSPECIFIED.,.F.,.F.,(3,3),(0.,1.),.UNSPECIFIED.);
#1264=B_SPLINE_CURVE_WITH_KNOTS('',2,(#65261,#65262,#65263),
 .UNSPECIFIED.,.F.,.F.,(3,3),(0.,1.),.UNSPECIFIED.);
#1265=B_SPLINE_CURVE_WITH_KNOTS('',2,(#65271,#65272,#65273),
 .UNSPECIFIED.,.F.,.F.,(3,3),(0.,1.),.UNSPECIFIED.);
#1266=B_SPLINE_CURVE_WITH_KNOTS('',2,(#65276,#65277,#65278),
 .UNSPECIFIED.,.F.,.F.,(3,3),(0.,1.),.UNSPECIFIED.);
#1267=B_SPLINE_CURVE_WITH_KNOTS('',2,(#65286,#65287,#65288),
 .UNSPECIFIED.,.F.,.F.,(3,3),(0.,1.),.UNSPECIFIED.);
#1268=B_SPLINE_CURVE_WITH_KNOTS('',2,(#65291,#65292,#65293),
 .UNSPECIFIED.,.F.,.F.,(3,3),(0.,1.),.UNSPECIFIED.);
#1269=B_SPLINE_CURVE_WITH_KNOTS('',2,(#65301,#65302,#65303),
 .UNSPECIFIED.,.F.,.F.,(3,3),(0.,1.),.UNSPECIFIED.);
#1270=B_SPLINE_CURVE_WITH_KNOTS('',2,(#65306,#65307,#65308),
 .UNSPECIFIED.,.F.,.F.,(3,3),(0.,1.),.UNSPECIFIED.);
#1271=B_SPLINE_CURVE_WITH_KNOTS('',2,(#65316,#65317,#65318),
 .UNSPECIFIED.,.F.,.F.,(3,3),(0.,1.),.UNSPECIFIED.);
#1272=B_SPLINE_CURVE_WITH_KNOTS('',2,(#65321,#65322,#65323),
 .UNSPECIFIED.,.F.,.F.,(3,3),(0.,1.),.UNSPECIFIED.);
#1273=B_SPLINE_CURVE_WITH_KNOTS('',2,(#65330,#65331,#65332),
 .UNSPECIFIED.,.F.,.F.,(3,3),(0.,1.),.UNSPECIFIED.);
#1274=B_SPLINE_CURVE_WITH_KNOTS('',2,(#65333,#65334,#65335),
 .UNSPECIFIED.,.F.,.F.,(3,3),(0.,1.),.UNSPECIFIED.);
#1275=B_SPLINE_CURVE_WITH_KNOTS('',2,(#65370,#65371,#65372),
 .UNSPECIFIED.,.F.,.F.,(3,3),(0.,1.),.UNSPECIFIED.);
#1276=B_SPLINE_CURVE_WITH_KNOTS('',2,(#65376,#65377,#65378),
 .UNSPECIFIED.,.F.,.F.,(3,3),(0.,1.),.UNSPECIFIED.);
#1277=B_SPLINE_CURVE_WITH_KNOTS('',2,(#65387,#65388,#65389),
 .UNSPECIFIED.,.F.,.F.,(3,3),(0.,1.),.UNSPECIFIED.);
#1278=B_SPLINE_CURVE_WITH_KNOTS('',2,(#65392,#65393,#65394),
 .UNSPECIFIED.,.F.,.F.,(3,3),(0.,1.),.UNSPECIFIED.);
#1279=B_SPLINE_CURVE_WITH_KNOTS('',2,(#65402,#65403,#65404),
 .UNSPECIFIED.,.F.,.F.,(3,3),(0.,1.),.UNSPECIFIED.);
#1280=B_SPLINE_CURVE_WITH_KNOTS('',2,(#65407,#65408,#65409),
 .UNSPECIFIED.,.F.,.F.,(3,3),(0.,1.),.UNSPECIFIED.);
#1281=B_SPLINE_CURVE_WITH_KNOTS('',2,(#65417,#65418,#65419),
 .UNSPECIFIED.,.F.,.F.,(3,3),(0.,1.),.UNSPECIFIED.);
#1282=B_SPLINE_CURVE_WITH_KNOTS('',2,(#65422,#65423,#65424),
 .UNSPECIFIED.,.F.,.F.,(3,3),(0.,1.),.UNSPECIFIED.);
#1283=B_SPLINE_CURVE_WITH_KNOTS('',2,(#65432,#65433,#65434),
 .UNSPECIFIED.,.F.,.F.,(3,3),(0.,1.),.UNSPECIFIED.);
#1284=B_SPLINE_CURVE_WITH_KNOTS('',2,(#65437,#65438,#65439),
 .UNSPECIFIED.,.F.,.F.,(3,3),(0.,1.),.UNSPECIFIED.);
#1285=B_SPLINE_CURVE_WITH_KNOTS('',2,(#65447,#65448,#65449),
 .UNSPECIFIED.,.F.,.F.,(3,3),(0.,1.),.UNSPECIFIED.);
#1286=B_SPLINE_CURVE_WITH_KNOTS('',2,(#65452,#65453,#65454),
 .UNSPECIFIED.,.F.,.F.,(3,3),(0.,1.),.UNSPECIFIED.);
#1287=B_SPLINE_CURVE_WITH_KNOTS('',2,(#65462,#65463,#65464),
 .UNSPECIFIED.,.F.,.F.,(3,3),(0.,1.),.UNSPECIFIED.);
#1288=B_SPLINE_CURVE_WITH_KNOTS('',2,(#65467,#65468,#65469),
 .UNSPECIFIED.,.F.,.F.,(3,3),(0.,1.),.UNSPECIFIED.);
#1289=B_SPLINE_CURVE_WITH_KNOTS('',2,(#65477,#65478,#65479),
 .UNSPECIFIED.,.F.,.F.,(3,3),(0.,1.),.UNSPECIFIED.);
#1290=B_SPLINE_CURVE_WITH_KNOTS('',2,(#65482,#65483,#65484),
 .UNSPECIFIED.,.F.,.F.,(3,3),(0.,1.),.UNSPECIFIED.);
#1291=B_SPLINE_CURVE_WITH_KNOTS('',2,(#65491,#65492,#65493),
 .UNSPECIFIED.,.F.,.F.,(3,3),(0.,1.),.UNSPECIFIED.);
#1292=B_SPLINE_CURVE_WITH_KNOTS('',2,(#65494,#65495,#65496),
 .UNSPECIFIED.,.F.,.F.,(3,3),(0.,1.),.UNSPECIFIED.);
#1293=B_SPLINE_CURVE_WITH_KNOTS('',2,(#65505,#65506,#65507),
 .UNSPECIFIED.,.F.,.F.,(3,3),(0.,1.),.UNSPECIFIED.);
#1294=B_SPLINE_CURVE_WITH_KNOTS('',2,(#65511,#65512,#65513),
 .UNSPECIFIED.,.F.,.F.,(3,3),(0.,1.),.UNSPECIFIED.);
#1295=B_SPLINE_CURVE_WITH_KNOTS('',2,(#65522,#65523,#65524),
 .UNSPECIFIED.,.F.,.F.,(3,3),(0.,1.),.UNSPECIFIED.);
#1296=B_SPLINE_CURVE_WITH_KNOTS('',2,(#65527,#65528,#65529),
 .UNSPECIFIED.,.F.,.F.,(3,3),(0.,1.),.UNSPECIFIED.);
#1297=B_SPLINE_CURVE_WITH_KNOTS('',2,(#65537,#65538,#65539),
 .UNSPECIFIED.,.F.,.F.,(3,3),(0.,1.),.UNSPECIFIED.);
#1298=B_SPLINE_CURVE_WITH_KNOTS('',2,(#65542,#65543,#65544),
 .UNSPECIFIED.,.F.,.F.,(3,3),(0.,1.),.UNSPECIFIED.);
#1299=B_SPLINE_CURVE_WITH_KNOTS('',2,(#65552,#65553,#65554),
 .UNSPECIFIED.,.F.,.F.,(3,3),(0.,1.),.UNSPECIFIED.);
#1300=B_SPLINE_CURVE_WITH_KNOTS('',2,(#65557,#65558,#65559),
 .UNSPECIFIED.,.F.,.F.,(3,3),(0.,1.),.UNSPECIFIED.);
#1301=B_SPLINE_CURVE_WITH_KNOTS('',2,(#65567,#65568,#65569),
 .UNSPECIFIED.,.F.,.F.,(3,3),(0.,1.),.UNSPECIFIED.);
#1302=B_SPLINE_CURVE_WITH_KNOTS('',2,(#65572,#65573,#65574),
 .UNSPECIFIED.,.F.,.F.,(3,3),(0.,1.),.UNSPECIFIED.);
#1303=B_SPLINE_CURVE_WITH_KNOTS('',2,(#65582,#65583,#65584),
 .UNSPECIFIED.,.F.,.F.,(3,3),(0.,1.),.UNSPECIFIED.);
#1304=B_SPLINE_CURVE_WITH_KNOTS('',2,(#65587,#65588,#65589),
 .UNSPECIFIED.,.F.,.F.,(3,3),(0.,1.),.UNSPECIFIED.);
#1305=B_SPLINE_CURVE_WITH_KNOTS('',2,(#65597,#65598,#65599),
 .UNSPECIFIED.,.F.,.F.,(3,3),(0.,1.),.UNSPECIFIED.);
#1306=B_SPLINE_CURVE_WITH_KNOTS('',2,(#65602,#65603,#65604),
 .UNSPECIFIED.,.F.,.F.,(3,3),(0.,1.),.UNSPECIFIED.);
#1307=B_SPLINE_CURVE_WITH_KNOTS('',2,(#65611,#65612,#65613),
 .UNSPECIFIED.,.F.,.F.,(3,3),(0.,1.),.UNSPECIFIED.);
#1308=B_SPLINE_CURVE_WITH_KNOTS('',2,(#65614,#65615,#65616),
 .UNSPECIFIED.,.F.,.F.,(3,3),(0.,1.),.UNSPECIFIED.);
#1309=B_SPLINE_CURVE_WITH_KNOTS('',2,(#65625,#65626,#65627),
 .UNSPECIFIED.,.F.,.F.,(3,3),(0.,1.),.UNSPECIFIED.);
#1310=B_SPLINE_CURVE_WITH_KNOTS('',2,(#65631,#65632,#65633),
 .UNSPECIFIED.,.F.,.F.,(3,3),(0.,1.),.UNSPECIFIED.);
#1311=B_SPLINE_CURVE_WITH_KNOTS('',2,(#65642,#65643,#65644),
 .UNSPECIFIED.,.F.,.F.,(3,3),(0.,1.),.UNSPECIFIED.);
#1312=B_SPLINE_CURVE_WITH_KNOTS('',2,(#65647,#65648,#65649),
 .UNSPECIFIED.,.F.,.F.,(3,3),(0.,1.),.UNSPECIFIED.);
#1313=B_SPLINE_CURVE_WITH_KNOTS('',2,(#65657,#65658,#65659),
 .UNSPECIFIED.,.F.,.F.,(3,3),(0.,1.),.UNSPECIFIED.);
#1314=B_SPLINE_CURVE_WITH_KNOTS('',2,(#65662,#65663,#65664),
 .UNSPECIFIED.,.F.,.F.,(3,3),(0.,1.),.UNSPECIFIED.);
#1315=B_SPLINE_CURVE_WITH_KNOTS('',2,(#65672,#65673,#65674),
 .UNSPECIFIED.,.F.,.F.,(3,3),(0.,1.),.UNSPECIFIED.);
#1316=B_SPLINE_CURVE_WITH_KNOTS('',2,(#65677,#65678,#65679),
 .UNSPECIFIED.,.F.,.F.,(3,3),(0.,1.),.UNSPECIFIED.);
#1317=B_SPLINE_CURVE_WITH_KNOTS('',2,(#65687,#65688,#65689),
 .UNSPECIFIED.,.F.,.F.,(3,3),(0.,1.),.UNSPECIFIED.);
#1318=B_SPLINE_CURVE_WITH_KNOTS('',2,(#65692,#65693,#65694),
 .UNSPECIFIED.,.F.,.F.,(3,3),(0.,1.),.UNSPECIFIED.);
#1319=B_SPLINE_CURVE_WITH_KNOTS('',2,(#65702,#65703,#65704),
 .UNSPECIFIED.,.F.,.F.,(3,3),(0.,1.),.UNSPECIFIED.);
#1320=B_SPLINE_CURVE_WITH_KNOTS('',2,(#65707,#65708,#65709),
 .UNSPECIFIED.,.F.,.F.,(3,3),(0.,1.),.UNSPECIFIED.);
#1321=B_SPLINE_CURVE_WITH_KNOTS('',2,(#65717,#65718,#65719),
 .UNSPECIFIED.,.F.,.F.,(3,3),(0.,1.),.UNSPECIFIED.);
#1322=B_SPLINE_CURVE_WITH_KNOTS('',2,(#65722,#65723,#65724),
 .UNSPECIFIED.,.F.,.F.,(3,3),(0.,1.),.UNSPECIFIED.);
#1323=B_SPLINE_CURVE_WITH_KNOTS('',2,(#65732,#65733,#65734),
 .UNSPECIFIED.,.F.,.F.,(3,3),(0.,1.),.UNSPECIFIED.);
#1324=B_SPLINE_CURVE_WITH_KNOTS('',2,(#65737,#65738,#65739),
 .UNSPECIFIED.,.F.,.F.,(3,3),(0.,1.),.UNSPECIFIED.);
#1325=B_SPLINE_CURVE_WITH_KNOTS('',2,(#65747,#65748,#65749),
 .UNSPECIFIED.,.F.,.F.,(3,3),(0.,1.),.UNSPECIFIED.);
#1326=B_SPLINE_CURVE_WITH_KNOTS('',2,(#65752,#65753,#65754),
 .UNSPECIFIED.,.F.,.F.,(3,3),(0.,1.),.UNSPECIFIED.);
#1327=B_SPLINE_CURVE_WITH_KNOTS('',2,(#65762,#65763,#65764),
 .UNSPECIFIED.,.F.,.F.,(3,3),(0.,1.),.UNSPECIFIED.);
#1328=B_SPLINE_CURVE_WITH_KNOTS('',2,(#65767,#65768,#65769),
 .UNSPECIFIED.,.F.,.F.,(3,3),(0.,1.),.UNSPECIFIED.);
#1329=B_SPLINE_CURVE_WITH_KNOTS('',2,(#65777,#65778,#65779),
 .UNSPECIFIED.,.F.,.F.,(3,3),(0.,1.),.UNSPECIFIED.);
#1330=B_SPLINE_CURVE_WITH_KNOTS('',2,(#65782,#65783,#65784),
 .UNSPECIFIED.,.F.,.F.,(3,3),(0.,1.),.UNSPECIFIED.);
#1331=B_SPLINE_CURVE_WITH_KNOTS('',2,(#65792,#65793,#65794),
 .UNSPECIFIED.,.F.,.F.,(3,3),(0.,1.),.UNSPECIFIED.);
#1332=B_SPLINE_CURVE_WITH_KNOTS('',2,(#65797,#65798,#65799),
 .UNSPECIFIED.,.F.,.F.,(3,3),(0.,1.),.UNSPECIFIED.);
#1333=B_SPLINE_CURVE_WITH_KNOTS('',2,(#65807,#65808,#65809),
 .UNSPECIFIED.,.F.,.F.,(3,3),(0.,1.),.UNSPECIFIED.);
#1334=B_SPLINE_CURVE_WITH_KNOTS('',2,(#65812,#65813,#65814),
 .UNSPECIFIED.,.F.,.F.,(3,3),(0.,1.),.UNSPECIFIED.);
#1335=B_SPLINE_CURVE_WITH_KNOTS('',2,(#65822,#65823,#65824),
 .UNSPECIFIED.,.F.,.F.,(3,3),(0.,1.),.UNSPECIFIED.);
#1336=B_SPLINE_CURVE_WITH_KNOTS('',2,(#65827,#65828,#65829),
 .UNSPECIFIED.,.F.,.F.,(3,3),(0.,1.),.UNSPECIFIED.);
#1337=B_SPLINE_CURVE_WITH_KNOTS('',2,(#65837,#65838,#65839),
 .UNSPECIFIED.,.F.,.F.,(3,3),(0.,1.),.UNSPECIFIED.);
#1338=B_SPLINE_CURVE_WITH_KNOTS('',2,(#65842,#65843,#65844),
 .UNSPECIFIED.,.F.,.F.,(3,3),(0.,1.),.UNSPECIFIED.);
#1339=B_SPLINE_CURVE_WITH_KNOTS('',2,(#65851,#65852,#65853),
 .UNSPECIFIED.,.F.,.F.,(3,3),(0.,1.),.UNSPECIFIED.);
#1340=B_SPLINE_CURVE_WITH_KNOTS('',2,(#65854,#65855,#65856),
 .UNSPECIFIED.,.F.,.F.,(3,3),(0.,1.),.UNSPECIFIED.);
#1341=B_SPLINE_CURVE_WITH_KNOTS('',3,(#65863,#65864,#65865,#65866,#65867,
#65868,#65869,#65870,#65871,#65872,#65873,#65874,#65875,#65876,#65877,#65878,
#65879,#65880,#65881,#65882,#65883,#65884,#65885,#65886,#65887,#65888,#65889,
#65890,#65891,#65892,#65893,#65894,#65895,#65896,#65897,#65898,#65899,#65900,
#65901,#65902,#65903,#65904,#65905,#65906,#65907,#65908,#65909,#65910,#65911,
#65912,#65913,#65914,#65915,#65916,#65917,#65918,#65919,#65920,#65921,#65922,
#65923,#65924,#65925,#65926,#65927,#65928,#65929,#65930,#65931,#65932,#65933,
#65934,#65935),.UNSPECIFIED.,.F.,.F.,(4,3,3,3,3,3,3,3,3,3,3,3,3,3,3,3,3,
3,3,3,3,3,3,3,4),(-1.53373699248747,-1.47998259246901,-1.39266174048304,
-1.36022791806051,-1.33444301006683,-1.23257109729599,-1.16841771032442,
-1.14505420412193,-1.13069918452514,-1.02732007613362,-0.923657890223372,
-0.893957590402323,-0.872515155528604,-0.767248151591737,-0.672999266808395,
-0.620634679909978,-0.597605365315507,-0.48985421101852,-0.390252612458368,
-0.338746494543295,-0.311332063159986,-0.288956015137301,-0.179727021085193,
-0.0696390475340457,0.),.UNSPECIFIED.);
#1342=B_SPLINE_CURVE_WITH_KNOTS('',3,(#65940,#65941,#65942,#65943,#65944,
#65945,#65946,#65947,#65948,#65949,#65950,#65951,#65952,#65953,#65954,#65955,
#65956,#65957,#65958,#65959,#65960,#65961,#65962,#65963,#65964,#65965,#65966,
#65967,#65968,#65969,#65970,#65971,#65972,#65973,#65974,#65975,#65976,#65977,
#65978,#65979,#65980,#65981,#65982,#65983,#65984,#65985,#65986,#65987,#65988,
#65989,#65990,#65991,#65992,#65993,#65994,#65995,#65996,#65997,#65998,#65999,
#66000,#66001,#66002,#66003,#66004,#66005,#66006,#66007,#66008,#66009,#66010,
#66011,#66012,#66013,#66014,#66015),.UNSPECIFIED.,.F.,.F.,(4,3,3,3,3,3,
3,3,3,3,3,3,3,3,3,3,3,3,3,3,3,3,3,3,3,4),(-1.52870610664506,-1.46664447796478,
-1.3700636136821,-1.32344222320383,-1.2949393095723,-1.18763016520319,-1.12106166313349,
-1.09619363797947,-1.08032102083408,-0.973278106620055,-0.867444501613014,
-0.829257794374334,-0.806280268847329,-0.706769958895532,-0.616721647432219,
-0.570817503182251,-0.543589420844949,-0.522682905689514,-0.420869349973873,
-0.346576713042279,-0.298085656104414,-0.273538172108159,-0.252565316088657,
-0.152507693175629,-0.0540854058072747,0.),.UNSPECIFIED.);
#1343=B_SPLINE_CURVE_WITH_KNOTS('',3,(#68168,#68169,#68170,#68171),
 .UNSPECIFIED.,.F.,.F.,(4,4),(371.831581829739,372.244171931201),
 .UNSPECIFIED.);
#1344=B_SPLINE_CURVE_WITH_KNOTS('',3,(#68173,#68174,#68175,#68176,#68177,
#68178,#68179,#68180,#68181,#68182,#68183,#68184,#68185,#68186,#68187,#68188,
#68189,#68190,#68191,#68192,#68193,#68194,#68195,#68196,#68197,#68198,#68199,
#68200,#68201,#68202,#68203,#68204,#68205,#68206,#68207,#68208,#68209,#68210,
#68211,#68212,#68213,#68214,#68215,#68216,#68217,#68218,#68219,#68220,#68221,
#68222,#68223,#68224,#68225,#68226,#68227,#68228,#68229,#68230,#68231,#68232,
#68233,#68234,#68235,#68236,#68237,#68238,#68239,#68240,#68241,#68242,#68243,
#68244,#68245),.UNSPECIFIED.,.F.,.F.,(4,3,3,3,3,3,3,3,3,3,3,3,3,3,3,3,3,
3,3,3,3,3,3,3,4),(-1.53373699248741,-1.47998259246889,-1.39266174048294,
-1.36022791797891,-1.33444300979088,-1.23257109715798,-1.16841771016461,
-1.14505420410101,-1.13069918452509,-1.02732007613401,-0.923657890214898,
-0.893957590232833,-0.872515155439738,-0.767248151591644,-0.672999266808298,
-0.620634679898911,-0.597605365440628,-0.489854211146256,-0.39025261245826,
-0.338746494550714,-0.31133206291671,-0.288956014985721,-0.179727020905079,
-0.069639047355687,0.),.UNSPECIFIED.);
#1345=B_SPLINE_CURVE_WITH_KNOTS('',3,(#68246,#68247,#68248,#68249,#68250,
#68251,#68252,#68253,#68254,#68255,#68256),.UNSPECIFIED.,.F.,.F.,(4,1,1,
1,1,1,1,1,4),(10.3761157273109,11.2956825218578,12.2938669442682,13.2920513666786,
13.7911435778838,14.2902357890889,14.7893280002941,15.2884202114993,15.7079632679497),
 .UNSPECIFIED.);
#1346=B_SPLINE_CURVE_WITH_KNOTS('',3,(#68262,#68263,#68264,#68265,#68266,
#68267,#68268,#68269,#68270,#68271,#68272,#68273,#68274,#68275,#68276,#68277,
#68278,#68279,#68280,#68281,#68282,#68283,#68284,#68285,#68286,#68287,#68288,
#68289,#68290,#68291,#68292,#68293,#68294,#68295,#68296,#68297,#68298,#68299,
#68300,#68301,#68302,#68303,#68304,#68305,#68306,#68307,#68308,#68309,#68310,
#68311,#68312,#68313,#68314,#68315,#68316,#68317,#68318,#68319,#68320,#68321,
#68322,#68323,#68324,#68325,#68326,#68327,#68328,#68329,#68330,#68331,#68332,
#68333,#68334,#68335,#68336,#68337),.UNSPECIFIED.,.F.,.F.,(4,3,3,3,3,3,
3,3,3,3,3,3,3,3,3,3,3,3,3,3,3,3,3,3,3,4),(-1.52870610664519,-1.46664447796486,
-1.37006361368218,-1.32344222320996,-1.29493930957835,-1.18763016520624,
-1.12106166311689,-1.09619363797475,-1.08032102083414,-0.973278106621115,
-0.867444501594008,-0.829257794543526,-0.806280268864396,-0.706769958895627,
-0.616721647432272,-0.570817503170463,-0.54358942061174,-0.52268290565152,
-0.420869349933775,-0.346576713042208,-0.29808565610603,-0.273538172313205,
-0.252565316556387,-0.152507693644889,-0.0540854062652702,0.),
 .UNSPECIFIED.);
#1347=B_SPLINE_CURVE_WITH_KNOTS('',3,(#68340,#68341,#68342,#68343,#68344,
#68345,#68346,#68347,#68348,#68349),.UNSPECIFIED.,.F.,.F.,(4,1,1,1,1,1,
1,4),(11.6150328478189,12.1141250590241,12.6132172702293,13.1123094814345,
13.6114016926397,14.60958611505,15.6077705374604,15.7079632679496),
 .UNSPECIFIED.);
#1348=B_SPLINE_SURFACE_WITH_KNOTS('',3,3,((#37899,#37900,#37901,#37902,
#37903,#37904,#37905,#37906,#37907),(#37908,#37909,#37910,#37911,#37912,
#37913,#37914,#37915,#37916),(#37917,#37918,#37919,#37920,#37921,#37922,
#37923,#37924,#37925),(#37926,#37927,#37928,#37929,#37930,#37931,#37932,
#37933,#37934)),.UNSPECIFIED.,.F.,.F.,.F.,(4,4),(4,1,1,1,2,4),(0.,1.),(1.61732157627536,
1.83434749782276,2.05137341937016,2.26839934091757,2.70245118401238,2.76222327472562),
 .UNSPECIFIED.);
#1349=B_SPLINE_SURFACE_WITH_KNOTS('',3,3,((#37959,#37960,#37961,#37962),
(#37963,#37964,#37965,#37966),(#37967,#37968,#37969,#37970),(#37971,#37972,
#37973,#37974)),.UNSPECIFIED.,.F.,.F.,.F.,(4,4),(4,4),(0.,1.),(-2.03375105473527,
-1.90569248523429),.UNSPECIFIED.);
#1350=B_SPLINE_SURFACE_WITH_KNOTS('',3,3,((#37983,#37984,#37985,#37986),
(#37987,#37988,#37989,#37990),(#37991,#37992,#37993,#37994),(#37995,#37996,
#37997,#37998)),.UNSPECIFIED.,.F.,.F.,.F.,(4,4),(4,4),(0.,1.),(-1.2359001683555,
-1.10784159885376),.UNSPECIFIED.);
#1351=B_SPLINE_SURFACE_WITH_KNOTS('',3,3,((#38516,#38517,#38518,#38519,
#38520,#38521,#38522,#38523,#38524,#38525,#38526),(#38527,#38528,#38529,
#38530,#38531,#38532,#38533,#38534,#38535,#38536,#38537),(#38538,#38539,
#38540,#38541,#38542,#38543,#38544,#38545,#38546,#38547,#38548),(#38549,
#38550,#38551,#38552,#38553,#38554,#38555,#38556,#38557,#38558,#38559)),
 .UNSPECIFIED.,.F.,.F.,.F.,(4,4),(4,2,1,1,1,2,4),(0.,1.),(1.61732157627537,
1.67709366698862,2.08723667379813,2.39484392890525,2.49737968060763,2.70245118401238,
2.76222327472563),.UNSPECIFIED.);
#1352=B_SPLINE_SURFACE_WITH_KNOTS('',3,3,((#38575,#38576,#38577,#38578),
(#38579,#38580,#38581,#38582),(#38583,#38584,#38585,#38586),(#38587,#38588,
#38589,#38590)),.UNSPECIFIED.,.F.,.F.,.F.,(4,4),(4,4),(0.,1.),(1.10784159885453,
1.2359001683555),.UNSPECIFIED.);
#1353=B_SPLINE_SURFACE_WITH_KNOTS('',3,3,((#38595,#38596,#38597,#38598),
(#38599,#38600,#38601,#38602),(#38603,#38604,#38605,#38606),(#38607,#38608,
#38609,#38610)),.UNSPECIFIED.,.F.,.F.,.F.,(4,4),(4,4),(0.,1.),(1.9056924852343,
2.03375105473601),.UNSPECIFIED.);
#1354=B_SPLINE_SURFACE_WITH_KNOTS('',3,3,((#38671,#38672,#38673,#38674,
#38675,#38676,#38677,#38678,#38679,#38680),(#38681,#38682,#38683,#38684,
#38685,#38686,#38687,#38688,#38689,#38690),(#38691,#38692,#38693,#38694,
#38695,#38696,#38697,#38698,#38699,#38700),(#38701,#38702,#38703,#38704,
#38705,#38706,#38707,#38708,#38709,#38710)),.UNSPECIFIED.,.F.,.F.,.F.,(4,
4),(4,1,1,1,1,2,4),(0.,1.),(1.61732157627536,1.83434749782276,2.05137341937017,
2.26839934091757,2.48542526246498,2.70245118401238,2.76222327472564),
 .UNSPECIFIED.);
#1355=B_SPLINE_SURFACE_WITH_KNOTS('',3,3,((#38725,#38726,#38727,#38728),
(#38729,#38730,#38731,#38732),(#38733,#38734,#38735,#38736),(#38737,#38738,
#38739,#38740)),.UNSPECIFIED.,.F.,.F.,.F.,(4,4),(4,4),(0.,1.),(-2.03375105473527,
-1.90569248523429),.UNSPECIFIED.);
#1356=B_SPLINE_SURFACE_WITH_KNOTS('',3,3,((#38745,#38746,#38747,#38748),
(#38749,#38750,#38751,#38752),(#38753,#38754,#38755,#38756),(#38757,#38758,
#38759,#38760)),.UNSPECIFIED.,.F.,.F.,.F.,(4,4),(4,4),(0.,1.),(-1.2359001683555,
-1.10784159885378),.UNSPECIFIED.);
#1357=B_SPLINE_SURFACE_WITH_KNOTS('',3,3,((#38972,#38973,#38974,#38975,
#38976,#38977,#38978,#38979,#38980,#38981,#38982,#38983,#38984,#38985,#38986,
#38987,#38988,#38989,#38990,#38991),(#38992,#38993,#38994,#38995,#38996,
#38997,#38998,#38999,#39000,#39001,#39002,#39003,#39004,#39005,#39006,#39007,
#39008,#39009,#39010,#39011),(#39012,#39013,#39014,#39015,#39016,#39017,
#39018,#39019,#39020,#39021,#39022,#39023,#39024,#39025,#39026,#39027,#39028,
#39029,#39030,#39031),(#39032,#39033,#39034,#39035,#39036,#39037,#39038,
#39039,#39040,#39041,#39042,#39043,#39044,#39045,#39046,#39047,#39048,#39049,
#39050,#39051)),.UNSPECIFIED.,.F.,.F.,.F.,(4,4),(4,2,2,1,2,2,2,2,2,1,4),
(0.,1.),(0.779480614358526,0.806562617083009,0.843388556026078,1.45419115408482,
1.6577920201044,1.72690435024433,1.76021140268278,1.89936032175267,2.0015894299973,
2.60016813064741,2.79969436419745),.UNSPECIFIED.);
#1358=B_SPLINE_SURFACE_WITH_KNOTS('',3,3,((#39057,#39058,#39059,#39060),
(#39061,#39062,#39063,#39064),(#39065,#39066,#39067,#39068),(#39069,#39070,
#39071,#39072)),.UNSPECIFIED.,.F.,.F.,.F.,(4,4),(4,4),(0.,1.),(-0.985110783337743,
-0.90995102981447),.UNSPECIFIED.);
#1359=B_SPLINE_SURFACE_WITH_KNOTS('',3,3,((#39073,#39074,#39075,#39076),
(#39077,#39078,#39079,#39080),(#39081,#39082,#39083,#39084),(#39085,#39086,
#39087,#39088)),.UNSPECIFIED.,.F.,.F.,.F.,(4,4),(4,4),(0.,1.),(-2.23164162261785,
-2.15648187025204),.UNSPECIFIED.);
#1360=B_SPLINE_SURFACE_WITH_KNOTS('',3,3,((#39214,#39215,#39216,#39217,
#39218,#39219,#39220,#39221,#39222,#39223,#39224,#39225,#39226,#39227,#39228,
#39229,#39230,#39231,#39232,#39233,#39234),(#39235,#39236,#39237,#39238,
#39239,#39240,#39241,#39242,#39243,#39244,#39245,#39246,#39247,#39248,#39249,
#39250,#39251,#39252,#39253,#39254,#39255),(#39256,#39257,#39258,#39259,
#39260,#39261,#39262,#39263,#39264,#39265,#39266,#39267,#39268,#39269,#39270,
#39271,#39272,#39273,#39274,#39275,#39276),(#39277,#39278,#39279,#39280,
#39281,#39282,#39283,#39284,#39285,#39286,#39287,#39288,#39289,#39290,#39291,
#39292,#39293,#39294,#39295,#39296,#39297)),.UNSPECIFIED.,.F.,.F.,.F.,(4,
4),(4,2,2,1,2,1,2,1,2,1,2,1,4),(0.,1.),(0.779480614358288,0.806562617082741,
0.843388556025833,1.28514645313502,1.7269043502442,1.73523111335382,1.76021140268269,
1.82978586221579,1.89936032174889,1.95047487587308,2.00158942999727,2.60016813064741,
2.79969436419745),.UNSPECIFIED.);
#1361=B_SPLINE_SURFACE_WITH_KNOTS('',3,3,((#39303,#39304,#39305,#39306),
(#39307,#39308,#39309,#39310),(#39311,#39312,#39313,#39314),(#39315,#39316,
#39317,#39318)),.UNSPECIFIED.,.F.,.F.,.F.,(4,4),(4,4),(0.,1.),(2.15648187025205,
2.23164162377532),.UNSPECIFIED.);
#1362=B_SPLINE_SURFACE_WITH_KNOTS('',3,3,((#39319,#39320,#39321,#39322),
(#39323,#39324,#39325,#39326),(#39327,#39328,#39329,#39330),(#39331,#39332,
#39333,#39334)),.UNSPECIFIED.,.F.,.F.,.F.,(4,4),(4,4),(0.,1.),(0.90995103097194,
0.98511078333776),.UNSPECIFIED.);
#1363=B_SPLINE_SURFACE_WITH_KNOTS('',3,3,((#39335,#39336,#39337,#39338,
#39339,#39340,#39341,#39342,#39343,#39344,#39345,#39346,#39347,#39348,#39349,
#39350,#39351,#39352,#39353,#39354,#39355,#39356,#39357,#39358),(#39359,
#39360,#39361,#39362,#39363,#39364,#39365,#39366,#39367,#39368,#39369,#39370,
#39371,#39372,#39373,#39374,#39375,#39376,#39377,#39378,#39379,#39380,#39381,
#39382),(#39383,#39384,#39385,#39386,#39387,#39388,#39389,#39390,#39391,
#39392,#39393,#39394,#39395,#39396,#39397,#39398,#39399,#39400,#39401,#39402,
#39403,#39404,#39405,#39406),(#39407,#39408,#39409,#39410,#39411,#39412,
#39413,#39414,#39415,#39416,#39417,#39418,#39419,#39420,#39421,#39422,#39423,
#39424,#39425,#39426,#39427,#39428,#39429,#39430)),.UNSPECIFIED.,.F.,.F.,
 .F.,(4,4),(4,2,2,2,2,2,2,2,2,2,1,1,4),(0.,1.),(0.77948061435851,0.806562617082946,
0.843388556025962,1.50301394602541,1.65779202010408,1.72690435024419,1.76021140268274,
1.89936032174962,2.00158942999736,2.12581957279538,2.46275696849641,2.63122566634693,
2.79969436419745),.UNSPECIFIED.);
#1364=B_SPLINE_SURFACE_WITH_KNOTS('',3,3,((#39436,#39437,#39438,#39439),
(#39440,#39441,#39442,#39443),(#39444,#39445,#39446,#39447),(#39448,#39449,
#39450,#39451)),.UNSPECIFIED.,.F.,.F.,.F.,(4,4),(4,4),(0.,1.),(2.15648187025205,
2.23164162377532),.UNSPECIFIED.);
#1365=B_SPLINE_SURFACE_WITH_KNOTS('',3,3,((#39452,#39453,#39454,#39455),
(#39456,#39457,#39458,#39459),(#39460,#39461,#39462,#39463),(#39464,#39465,
#39466,#39467)),.UNSPECIFIED.,.F.,.F.,.F.,(4,4),(4,4),(0.,1.),(0.90995103097194,
0.985110783337756),.UNSPECIFIED.);
#1366=B_SPLINE_SURFACE_WITH_KNOTS('',3,3,((#39476,#39477,#39478,#39479,
#39480,#39481,#39482,#39483,#39484,#39485),(#39486,#39487,#39488,#39489,
#39490,#39491,#39492,#39493,#39494,#39495),(#39496,#39497,#39498,#39499,
#39500,#39501,#39502,#39503,#39504,#39505),(#39506,#39507,#39508,#39509,
#39510,#39511,#39512,#39513,#39514,#39515)),.UNSPECIFIED.,.F.,.F.,.F.,(4,
4),(4,2,1,1,2,4),(0.,1.),(1.61732157627537,1.67709366698862,2.08723667379812,
2.29230817720287,2.70245118401238,2.76222327472564),.UNSPECIFIED.);
#1367=B_SPLINE_SURFACE_WITH_KNOTS('',3,3,((#39530,#39531,#39532,#39533),
(#39534,#39535,#39536,#39537),(#39538,#39539,#39540,#39541),(#39542,#39543,
#39544,#39545)),.UNSPECIFIED.,.F.,.F.,.F.,(4,4),(4,4),(0.,1.),(1.10784159885453,
1.2359001683555),.UNSPECIFIED.);
#1368=B_SPLINE_SURFACE_WITH_KNOTS('',3,3,((#39550,#39551,#39552,#39553),
(#39554,#39555,#39556,#39557),(#39558,#39559,#39560,#39561),(#39562,#39563,
#39564,#39565)),.UNSPECIFIED.,.F.,.F.,.F.,(4,4),(4,4),(0.,1.),(1.9056924852343,
2.03375105473602),.UNSPECIFIED.);
#1369=B_SPLINE_SURFACE_WITH_KNOTS('',3,3,((#39618,#39619,#39620,#39621,
#39622,#39623,#39624,#39625,#39626,#39627,#39628,#39629,#39630,#39631,#39632,
#39633,#39634,#39635),(#39636,#39637,#39638,#39639,#39640,#39641,#39642,
#39643,#39644,#39645,#39646,#39647,#39648,#39649,#39650,#39651,#39652,#39653),
(#39654,#39655,#39656,#39657,#39658,#39659,#39660,#39661,#39662,#39663,
#39664,#39665,#39666,#39667,#39668,#39669,#39670,#39671),(#39672,#39673,
#39674,#39675,#39676,#39677,#39678,#39679,#39680,#39681,#39682,#39683,#39684,
#39685,#39686,#39687,#39688,#39689)),.UNSPECIFIED.,.F.,.F.,.F.,(4,4),(4,
2,2,1,1,2,2,2,1,1,4),(0.,1.),(0.779480614358544,0.806562617082991,0.843388556026153,
1.28514645313595,1.50602540169085,1.72690435024575,1.76021140268327,1.89936032175298,
2.57461085358633,2.68715260889189,2.79969436419745),.UNSPECIFIED.);
#1370=B_SPLINE_SURFACE_WITH_KNOTS('',3,3,((#39695,#39696,#39697,#39698),
(#39699,#39700,#39701,#39702),(#39703,#39704,#39705,#39706),(#39707,#39708,
#39709,#39710)),.UNSPECIFIED.,.F.,.F.,.F.,(4,4),(4,4),(0.,1.),(-0.985110783337744,
-0.909951029814477),.UNSPECIFIED.);
#1371=B_SPLINE_SURFACE_WITH_KNOTS('',3,3,((#39711,#39712,#39713,#39714),
(#39715,#39716,#39717,#39718),(#39719,#39720,#39721,#39722),(#39723,#39724,
#39725,#39726)),.UNSPECIFIED.,.F.,.F.,.F.,(4,4),(4,4),(0.,1.),(-2.23164162261785,
-2.15648187025204),.UNSPECIFIED.);
#1372=B_SPLINE_SURFACE_WITH_KNOTS('',3,3,((#39967,#39968,#39969,#39970,
#39971,#39972,#39973,#39974,#39975,#39976),(#39977,#39978,#39979,#39980,
#39981,#39982,#39983,#39984,#39985,#39986),(#39987,#39988,#39989,#39990,
#39991,#39992,#39993,#39994,#39995,#39996),(#39997,#39998,#39999,#40000,
#40001,#40002,#40003,#40004,#40005,#40006)),.UNSPECIFIED.,.F.,.F.,.F.,(4,
4),(4,2,1,1,2,4),(0.,1.),(1.61732157627537,1.67709366698862,2.08723667379812,
2.29230817720287,2.70245118401238,2.76222327472564),.UNSPECIFIED.);
#1373=B_SPLINE_SURFACE_WITH_KNOTS('',3,3,((#40029,#40030,#40031,#40032),
(#40033,#40034,#40035,#40036),(#40037,#40038,#40039,#40040),(#40041,#40042,
#40043,#40044)),.UNSPECIFIED.,.F.,.F.,.F.,(4,4),(4,4),(0.,1.),(1.9056924852343,
2.03375105473599),.UNSPECIFIED.);
#1374=B_SPLINE_SURFACE_WITH_KNOTS('',3,3,((#40049,#40050,#40051,#40052),
(#40053,#40054,#40055,#40056),(#40057,#40058,#40059,#40060),(#40061,#40062,
#40063,#40064)),.UNSPECIFIED.,.F.,.F.,.F.,(4,4),(4,4),(0.,1.),(1.10784159885453,
1.23590016835551),.UNSPECIFIED.);
#1375=B_SPLINE_SURFACE_WITH_KNOTS('',3,3,((#40386,#40387,#40388,#40389,
#40390,#40391,#40392,#40393,#40394,#40395,#40396,#40397,#40398,#40399,#40400,
#40401,#40402,#40403,#40404,#40405),(#40406,#40407,#40408,#40409,#40410,
#40411,#40412,#40413,#40414,#40415,#40416,#40417,#40418,#40419,#40420,#40421,
#40422,#40423,#40424,#40425),(#40426,#40427,#40428,#40429,#40430,#40431,
#40432,#40433,#40434,#40435,#40436,#40437,#40438,#40439,#40440,#40441,#40442,
#40443,#40444,#40445),(#40446,#40447,#40448,#40449,#40450,#40451,#40452,
#40453,#40454,#40455,#40456,#40457,#40458,#40459,#40460,#40461,#40462,#40463,
#40464,#40465)),.UNSPECIFIED.,.F.,.F.,.F.,(4,4),(4,2,2,1,1,2,2,2,2,1,1,
4),(0.,1.),(0.779480614358656,0.806562617083063,0.843388556026148,1.28514645313547,
1.50602540169013,1.7269043502448,1.76021140268296,1.82544138032945,1.89936032174889,
2.57461085358531,2.68715260889138,2.79969436419745),.UNSPECIFIED.);
#1376=B_SPLINE_SURFACE_WITH_KNOTS('',3,3,((#40471,#40472,#40473,#40474),
(#40475,#40476,#40477,#40478),(#40479,#40480,#40481,#40482),(#40483,#40484,
#40485,#40486)),.UNSPECIFIED.,.F.,.F.,.F.,(4,4),(4,4),(0.,1.),(-0.985110783337744,
-0.909951029814477),.UNSPECIFIED.);
#1377=B_SPLINE_SURFACE_WITH_KNOTS('',3,3,((#40487,#40488,#40489,#40490),
(#40491,#40492,#40493,#40494),(#40495,#40496,#40497,#40498),(#40499,#40500,
#40501,#40502)),.UNSPECIFIED.,.F.,.F.,.F.,(4,4),(4,4),(0.,1.),(-2.23164162261785,
-2.15648187025204),.UNSPECIFIED.);
#1378=B_SPLINE_SURFACE_WITH_KNOTS('',3,3,((#40511,#40512,#40513,#40514,
#40515,#40516,#40517,#40518,#40519,#40520),(#40521,#40522,#40523,#40524,
#40525,#40526,#40527,#40528,#40529,#40530),(#40531,#40532,#40533,#40534,
#40535,#40536,#40537,#40538,#40539,#40540),(#40541,#40542,#40543,#40544,
#40545,#40546,#40547,#40548,#40549,#40550)),.UNSPECIFIED.,.F.,.F.,.F.,(4,
4),(4,2,1,1,2,4),(0.,1.),(1.61732157627537,1.67709366698862,2.08723667379812,
2.29230817720288,2.70245118401238,2.76222327472563),.UNSPECIFIED.);
#1379=B_SPLINE_SURFACE_WITH_KNOTS('',3,3,((#40565,#40566,#40567,#40568),
(#40569,#40570,#40571,#40572),(#40573,#40574,#40575,#40576),(#40577,#40578,
#40579,#40580)),.UNSPECIFIED.,.F.,.F.,.F.,(4,4),(4,4),(0.,1.),(-2.03375105473527,
-1.90569248523429),.UNSPECIFIED.);
#1380=B_SPLINE_SURFACE_WITH_KNOTS('',3,3,((#40585,#40586,#40587,#40588),
(#40589,#40590,#40591,#40592),(#40593,#40594,#40595,#40596),(#40597,#40598,
#40599,#40600)),.UNSPECIFIED.,.F.,.F.,.F.,(4,4),(4,4),(0.,1.),(-1.2359001683555,
-1.10784159885378),.UNSPECIFIED.);
#1381=B_SPLINE_SURFACE_WITH_KNOTS('',3,3,((#40653,#40654,#40655,#40656,
#40657,#40658,#40659,#40660,#40661,#40662,#40663,#40664,#40665,#40666,#40667,
#40668,#40669,#40670,#40671,#40672),(#40673,#40674,#40675,#40676,#40677,
#40678,#40679,#40680,#40681,#40682,#40683,#40684,#40685,#40686,#40687,#40688,
#40689,#40690,#40691,#40692),(#40693,#40694,#40695,#40696,#40697,#40698,
#40699,#40700,#40701,#40702,#40703,#40704,#40705,#40706,#40707,#40708,#40709,
#40710,#40711,#40712),(#40713,#40714,#40715,#40716,#40717,#40718,#40719,
#40720,#40721,#40722,#40723,#40724,#40725,#40726,#40727,#40728,#40729,#40730,
#40731,#40732)),.UNSPECIFIED.,.F.,.F.,.F.,(4,4),(4,2,2,1,2,2,2,2,2,1,4),
(0.,1.),(0.77948061435839,0.806562617082694,0.843388556025742,1.45419115408438,
1.65779202010392,1.72690435024413,1.76021140268269,1.89936032174878,2.00158942999731,
2.60016813064743,2.79969436419747),.UNSPECIFIED.);
#1382=B_SPLINE_SURFACE_WITH_KNOTS('',3,3,((#40738,#40739,#40740,#40741),
(#40742,#40743,#40744,#40745),(#40746,#40747,#40748,#40749),(#40750,#40751,
#40752,#40753)),.UNSPECIFIED.,.F.,.F.,.F.,(4,4),(4,4),(0.,1.),(2.15648187025205,
2.23164162377532),.UNSPECIFIED.);
#1383=B_SPLINE_SURFACE_WITH_KNOTS('',3,3,((#40754,#40755,#40756,#40757),
(#40758,#40759,#40760,#40761),(#40762,#40763,#40764,#40765),(#40766,#40767,
#40768,#40769)),.UNSPECIFIED.,.F.,.F.,.F.,(4,4),(4,4),(0.,1.),(0.90995103097194,
0.985110783337756),.UNSPECIFIED.);
#1384=B_SPLINE_SURFACE_WITH_KNOTS('',3,3,((#40770,#40771,#40772,#40773,
#40774,#40775,#40776,#40777,#40778,#40779,#40780),(#40781,#40782,#40783,
#40784,#40785,#40786,#40787,#40788,#40789,#40790,#40791),(#40792,#40793,
#40794,#40795,#40796,#40797,#40798,#40799,#40800,#40801,#40802),(#40803,
#40804,#40805,#40806,#40807,#40808,#40809,#40810,#40811,#40812,#40813)),
 .UNSPECIFIED.,.F.,.F.,.F.,(4,4),(4,2,1,1,1,2,4),(0.,1.),(1.61732157627537,
1.67709366698862,2.08723667379813,2.39484392890525,2.49737968060763,2.70245118401238,
2.76222327472563),.UNSPECIFIED.);
#1385=B_SPLINE_SURFACE_WITH_KNOTS('',3,3,((#40837,#40838,#40839,#40840),
(#40841,#40842,#40843,#40844),(#40845,#40846,#40847,#40848),(#40849,#40850,
#40851,#40852)),.UNSPECIFIED.,.F.,.F.,.F.,(4,4),(4,4),(0.,1.),(1.9056924852343,
2.03375105473601),.UNSPECIFIED.);
#1386=B_SPLINE_SURFACE_WITH_KNOTS('',3,3,((#40857,#40858,#40859,#40860),
(#40861,#40862,#40863,#40864),(#40865,#40866,#40867,#40868),(#40869,#40870,
#40871,#40872)),.UNSPECIFIED.,.F.,.F.,.F.,(4,4),(4,4),(0.,1.),(1.10784159885453,
1.2359001683555),.UNSPECIFIED.);
#1387=B_SPLINE_SURFACE_WITH_KNOTS('',3,3,((#40925,#40926,#40927,#40928,
#40929,#40930,#40931,#40932,#40933,#40934,#40935,#40936,#40937,#40938,#40939,
#40940,#40941,#40942,#40943,#40944,#40945),(#40946,#40947,#40948,#40949,
#40950,#40951,#40952,#40953,#40954,#40955,#40956,#40957,#40958,#40959,#40960,
#40961,#40962,#40963,#40964,#40965,#40966),(#40967,#40968,#40969,#40970,
#40971,#40972,#40973,#40974,#40975,#40976,#40977,#40978,#40979,#40980,#40981,
#40982,#40983,#40984,#40985,#40986,#40987),(#40988,#40989,#40990,#40991,
#40992,#40993,#40994,#40995,#40996,#40997,#40998,#40999,#41000,#41001,#41002,
#41003,#41004,#41005,#41006,#41007,#41008)),.UNSPECIFIED.,.F.,.F.,.F.,(4,
4),(4,2,2,2,2,2,2,2,2,1,4),(0.,1.),(0.779480614358366,0.806562617082747,
0.84338855602576,1.65779202010374,1.72690435024399,1.76021140268264,1.82544138032896,
1.89936032174887,2.00158942999732,2.60016813064742,2.79969436419746),
 .UNSPECIFIED.);
#1388=B_SPLINE_SURFACE_WITH_KNOTS('',3,3,((#41014,#41015,#41016,#41017),
(#41018,#41019,#41020,#41021),(#41022,#41023,#41024,#41025),(#41026,#41027,
#41028,#41029)),.UNSPECIFIED.,.F.,.F.,.F.,(4,4),(4,4),(0.,1.),(-0.985110783337743,
-0.90995102981447),.UNSPECIFIED.);
#1389=B_SPLINE_SURFACE_WITH_KNOTS('',3,3,((#41030,#41031,#41032,#41033),
(#41034,#41035,#41036,#41037),(#41038,#41039,#41040,#41041),(#41042,#41043,
#41044,#41045)),.UNSPECIFIED.,.F.,.F.,.F.,(4,4),(4,4),(0.,1.),(-2.23164162261785,
-2.15648187025204),.UNSPECIFIED.);
#1390=B_SPLINE_SURFACE_WITH_KNOTS('',3,3,((#41054,#41055,#41056,#41057,
#41058,#41059,#41060,#41061,#41062,#41063),(#41064,#41065,#41066,#41067,
#41068,#41069,#41070,#41071,#41072,#41073),(#41074,#41075,#41076,#41077,
#41078,#41079,#41080,#41081,#41082,#41083),(#41084,#41085,#41086,#41087,
#41088,#41089,#41090,#41091,#41092,#41093)),.UNSPECIFIED.,.F.,.F.,.F.,(4,
4),(4,2,1,1,2,4),(0.,1.),(1.61732157627537,1.67709366698862,2.08723667379812,
2.29230817720287,2.70245118401238,2.76222327472562),.UNSPECIFIED.);
#1391=B_SPLINE_SURFACE_WITH_KNOTS('',3,3,((#41108,#41109,#41110,#41111),
(#41112,#41113,#41114,#41115),(#41116,#41117,#41118,#41119),(#41120,#41121,
#41122,#41123)),.UNSPECIFIED.,.F.,.F.,.F.,(4,4),(4,4),(0.,1.),(-2.03375105473527,
-1.90569248523429),.UNSPECIFIED.);
#1392=B_SPLINE_SURFACE_WITH_KNOTS('',3,3,((#41128,#41129,#41130,#41131),
(#41132,#41133,#41134,#41135),(#41136,#41137,#41138,#41139),(#41140,#41141,
#41142,#41143)),.UNSPECIFIED.,.F.,.F.,.F.,(4,4),(4,4),(0.,1.),(-1.23590016835549,
-1.10784159885377),.UNSPECIFIED.);
#1393=B_SPLINE_SURFACE_WITH_KNOTS('',3,3,((#41196,#41197,#41198,#41199,
#41200,#41201,#41202,#41203,#41204,#41205,#41206,#41207,#41208,#41209,#41210,
#41211,#41212,#41213,#41214,#41215),(#41216,#41217,#41218,#41219,#41220,
#41221,#41222,#41223,#41224,#41225,#41226,#41227,#41228,#41229,#41230,#41231,
#41232,#41233,#41234,#41235),(#41236,#41237,#41238,#41239,#41240,#41241,
#41242,#41243,#41244,#41245,#41246,#41247,#41248,#41249,#41250,#41251,#41252,
#41253,#41254,#41255),(#41256,#41257,#41258,#41259,#41260,#41261,#41262,
#41263,#41264,#41265,#41266,#41267,#41268,#41269,#41270,#41271,#41272,#41273,
#41274,#41275)),.UNSPECIFIED.,.F.,.F.,.F.,(4,4),(4,2,2,2,2,2,2,2,1,1,4),
(0.,1.),(0.779480614358288,0.806562617082717,0.843388556025879,1.65779202010542,
1.72690435024458,1.76021140268281,1.8254413803293,1.89936032174935,2.57461085358543,
2.68715260889144,2.79969436419745),.UNSPECIFIED.);
#1394=B_SPLINE_SURFACE_WITH_KNOTS('',3,3,((#41281,#41282,#41283,#41284),
(#41285,#41286,#41287,#41288),(#41289,#41290,#41291,#41292),(#41293,#41294,
#41295,#41296)),.UNSPECIFIED.,.F.,.F.,.F.,(4,4),(4,4),(0.,1.),(2.15648187025205,
2.23164162377533),.UNSPECIFIED.);
#1395=B_SPLINE_SURFACE_WITH_KNOTS('',3,3,((#41297,#41298,#41299,#41300),
(#41301,#41302,#41303,#41304),(#41305,#41306,#41307,#41308),(#41309,#41310,
#41311,#41312)),.UNSPECIFIED.,.F.,.F.,.F.,(4,4),(4,4),(0.,1.),(0.90995103097194,
0.985110783337753),.UNSPECIFIED.);
#1396=B_SPLINE_SURFACE_WITH_KNOTS('',2,1,((#41344,#41345),(#41346,#41347),
(#41348,#41349)),.UNSPECIFIED.,.F.,.F.,.F.,(3,3),(2,2),(0.,1.),(0.,0.0999999999999996),
 .UNSPECIFIED.);
#1397=B_SPLINE_SURFACE_WITH_KNOTS('',2,1,((#41362,#41363),(#41364,#41365),
(#41366,#41367)),.UNSPECIFIED.,.F.,.F.,.F.,(3,3),(2,2),(0.,1.),(0.,0.0999999999999996),
 .UNSPECIFIED.);
#1398=B_SPLINE_SURFACE_WITH_KNOTS('',2,1,((#41377,#41378),(#41379,#41380),
(#41381,#41382)),.UNSPECIFIED.,.F.,.F.,.F.,(3,3),(2,2),(0.,1.),(0.,0.0999999999999996),
 .UNSPECIFIED.);
#1399=B_SPLINE_SURFACE_WITH_KNOTS('',2,1,((#41392,#41393),(#41394,#41395),
(#41396,#41397)),.UNSPECIFIED.,.F.,.F.,.F.,(3,3),(2,2),(0.,1.),(0.,0.0999999999999996),
 .UNSPECIFIED.);
#1400=B_SPLINE_SURFACE_WITH_KNOTS('',2,1,((#41407,#41408),(#41409,#41410),
(#41411,#41412)),.UNSPECIFIED.,.F.,.F.,.F.,(3,3),(2,2),(0.,1.),(0.,0.0999999999999996),
 .UNSPECIFIED.);
#1401=B_SPLINE_SURFACE_WITH_KNOTS('',2,1,((#41422,#41423),(#41424,#41425),
(#41426,#41427)),.UNSPECIFIED.,.F.,.F.,.F.,(3,3),(2,2),(0.,1.),(0.,0.0999999999999996),
 .UNSPECIFIED.);
#1402=B_SPLINE_SURFACE_WITH_KNOTS('',2,1,((#41437,#41438),(#41439,#41440),
(#41441,#41442)),.UNSPECIFIED.,.F.,.F.,.F.,(3,3),(2,2),(0.,1.),(0.,0.0999999999999996),
 .UNSPECIFIED.);
#1403=B_SPLINE_SURFACE_WITH_KNOTS('',2,1,((#41452,#41453),(#41454,#41455),
(#41456,#41457)),.UNSPECIFIED.,.F.,.F.,.F.,(3,3),(2,2),(0.,1.),(0.,0.0999999999999996),
 .UNSPECIFIED.);
#1404=B_SPLINE_SURFACE_WITH_KNOTS('',2,1,((#41464,#41465),(#41466,#41467),
(#41468,#41469)),.UNSPECIFIED.,.F.,.F.,.F.,(3,3),(2,2),(0.,1.),(0.,0.0999999999999996),
 .UNSPECIFIED.);
#1405=B_SPLINE_SURFACE_WITH_KNOTS('',2,1,((#41477,#41478),(#41479,#41480),
(#41481,#41482)),.UNSPECIFIED.,.F.,.F.,.F.,(3,3),(2,2),(0.,1.),(0.,0.0999999999999996),
 .UNSPECIFIED.);
#1406=B_SPLINE_SURFACE_WITH_KNOTS('',2,1,((#41488,#41489),(#41490,#41491),
(#41492,#41493)),.UNSPECIFIED.,.F.,.F.,.F.,(3,3),(2,2),(0.,1.),(0.,0.0999999999999996),
 .UNSPECIFIED.);
#1407=B_SPLINE_SURFACE_WITH_KNOTS('',2,1,((#41499,#41500),(#41501,#41502),
(#41503,#41504)),.UNSPECIFIED.,.F.,.F.,.F.,(3,3),(2,2),(0.,1.),(0.,0.0999999999999996),
 .UNSPECIFIED.);
#1408=B_SPLINE_SURFACE_WITH_KNOTS('',2,1,((#41510,#41511),(#41512,#41513),
(#41514,#41515)),.UNSPECIFIED.,.F.,.F.,.F.,(3,3),(2,2),(0.,1.),(0.,0.0999999999999996),
 .UNSPECIFIED.);
#1409=B_SPLINE_SURFACE_WITH_KNOTS('',2,1,((#41521,#41522),(#41523,#41524),
(#41525,#41526)),.UNSPECIFIED.,.F.,.F.,.F.,(3,3),(2,2),(0.,1.),(0.,0.0999999999999996),
 .UNSPECIFIED.);
#1410=B_SPLINE_SURFACE_WITH_KNOTS('',2,1,((#41532,#41533),(#41534,#41535),
(#41536,#41537)),.UNSPECIFIED.,.F.,.F.,.F.,(3,3),(2,2),(0.,1.),(0.,0.0999999999999996),
 .UNSPECIFIED.);
#1411=B_SPLINE_SURFACE_WITH_KNOTS('',2,1,((#41543,#41544),(#41545,#41546),
(#41547,#41548)),.UNSPECIFIED.,.F.,.F.,.F.,(3,3),(2,2),(0.,1.),(0.,0.0999999999999996),
 .UNSPECIFIED.);
#1412=B_SPLINE_SURFACE_WITH_KNOTS('',2,1,((#41554,#41555),(#41556,#41557),
(#41558,#41559)),.UNSPECIFIED.,.F.,.F.,.F.,(3,3),(2,2),(0.,1.),(0.,0.0999999999999996),
 .UNSPECIFIED.);
#1413=B_SPLINE_SURFACE_WITH_KNOTS('',2,1,((#41565,#41566),(#41567,#41568),
(#41569,#41570)),.UNSPECIFIED.,.F.,.F.,.F.,(3,3),(2,2),(0.,1.),(0.,0.0999999999999996),
 .UNSPECIFIED.);
#1414=B_SPLINE_SURFACE_WITH_KNOTS('',2,1,((#41608,#41609),(#41610,#41611),
(#41612,#41613)),.UNSPECIFIED.,.F.,.F.,.F.,(3,3),(2,2),(0.,1.),(0.,0.0999999999999996),
 .UNSPECIFIED.);
#1415=B_SPLINE_SURFACE_WITH_KNOTS('',2,1,((#41626,#41627),(#41628,#41629),
(#41630,#41631)),.UNSPECIFIED.,.F.,.F.,.F.,(3,3),(2,2),(0.,1.),(0.,0.0999999999999996),
 .UNSPECIFIED.);
#1416=B_SPLINE_SURFACE_WITH_KNOTS('',2,1,((#41641,#41642),(#41643,#41644),
(#41645,#41646)),.UNSPECIFIED.,.F.,.F.,.F.,(3,3),(2,2),(0.,1.),(0.,0.0999999999999996),
 .UNSPECIFIED.);
#1417=B_SPLINE_SURFACE_WITH_KNOTS('',2,1,((#41656,#41657),(#41658,#41659),
(#41660,#41661)),.UNSPECIFIED.,.F.,.F.,.F.,(3,3),(2,2),(0.,1.),(0.,0.0999999999999996),
 .UNSPECIFIED.);
#1418=B_SPLINE_SURFACE_WITH_KNOTS('',2,1,((#41671,#41672),(#41673,#41674),
(#41675,#41676)),.UNSPECIFIED.,.F.,.F.,.F.,(3,3),(2,2),(0.,1.),(0.,0.0999999999999996),
 .UNSPECIFIED.);
#1419=B_SPLINE_SURFACE_WITH_KNOTS('',2,1,((#41686,#41687),(#41688,#41689),
(#41690,#41691)),.UNSPECIFIED.,.F.,.F.,.F.,(3,3),(2,2),(0.,1.),(0.,0.0999999999999996),
 .UNSPECIFIED.);
#1420=B_SPLINE_SURFACE_WITH_KNOTS('',2,1,((#41701,#41702),(#41703,#41704),
(#41705,#41706)),.UNSPECIFIED.,.F.,.F.,.F.,(3,3),(2,2),(0.,1.),(0.,0.0999999999999996),
 .UNSPECIFIED.);
#1421=B_SPLINE_SURFACE_WITH_KNOTS('',2,1,((#41716,#41717),(#41718,#41719),
(#41720,#41721)),.UNSPECIFIED.,.F.,.F.,.F.,(3,3),(2,2),(0.,1.),(0.,0.0999999999999996),
 .UNSPECIFIED.);
#1422=B_SPLINE_SURFACE_WITH_KNOTS('',2,1,((#41731,#41732),(#41733,#41734),
(#41735,#41736)),.UNSPECIFIED.,.F.,.F.,.F.,(3,3),(2,2),(0.,1.),(0.,0.0999999999999996),
 .UNSPECIFIED.);
#1423=B_SPLINE_SURFACE_WITH_KNOTS('',2,1,((#41743,#41744),(#41745,#41746),
(#41747,#41748)),.UNSPECIFIED.,.F.,.F.,.F.,(3,3),(2,2),(0.,1.),(0.,0.0999999999999996),
 .UNSPECIFIED.);
#1424=B_SPLINE_SURFACE_WITH_KNOTS('',2,1,((#41756,#41757),(#41758,#41759),
(#41760,#41761)),.UNSPECIFIED.,.F.,.F.,.F.,(3,3),(2,2),(0.,1.),(0.,0.0999999999999996),
 .UNSPECIFIED.);
#1425=B_SPLINE_SURFACE_WITH_KNOTS('',2,1,((#41767,#41768),(#41769,#41770),
(#41771,#41772)),.UNSPECIFIED.,.F.,.F.,.F.,(3,3),(2,2),(0.,1.),(0.,0.0999999999999996),
 .UNSPECIFIED.);
#1426=B_SPLINE_SURFACE_WITH_KNOTS('',2,1,((#41778,#41779),(#41780,#41781),
(#41782,#41783)),.UNSPECIFIED.,.F.,.F.,.F.,(3,3),(2,2),(0.,1.),(0.,0.0999999999999996),
 .UNSPECIFIED.);
#1427=B_SPLINE_SURFACE_WITH_KNOTS('',2,1,((#41789,#41790),(#41791,#41792),
(#41793,#41794)),.UNSPECIFIED.,.F.,.F.,.F.,(3,3),(2,2),(0.,1.),(0.,0.0999999999999996),
 .UNSPECIFIED.);
#1428=B_SPLINE_SURFACE_WITH_KNOTS('',2,1,((#41800,#41801),(#41802,#41803),
(#41804,#41805)),.UNSPECIFIED.,.F.,.F.,.F.,(3,3),(2,2),(0.,1.),(0.,0.0999999999999996),
 .UNSPECIFIED.);
#1429=B_SPLINE_SURFACE_WITH_KNOTS('',2,1,((#41811,#41812),(#41813,#41814),
(#41815,#41816)),.UNSPECIFIED.,.F.,.F.,.F.,(3,3),(2,2),(0.,1.),(0.,0.0999999999999996),
 .UNSPECIFIED.);
#1430=B_SPLINE_SURFACE_WITH_KNOTS('',2,1,((#41822,#41823),(#41824,#41825),
(#41826,#41827)),.UNSPECIFIED.,.F.,.F.,.F.,(3,3),(2,2),(0.,1.),(0.,0.0999999999999996),
 .UNSPECIFIED.);
#1431=B_SPLINE_SURFACE_WITH_KNOTS('',2,1,((#41833,#41834),(#41835,#41836),
(#41837,#41838)),.UNSPECIFIED.,.F.,.F.,.F.,(3,3),(2,2),(0.,1.),(0.,0.0999999999999996),
 .UNSPECIFIED.);
#1432=B_SPLINE_SURFACE_WITH_KNOTS('',2,1,((#41844,#41845),(#41846,#41847),
(#41848,#41849)),.UNSPECIFIED.,.F.,.F.,.F.,(3,3),(2,2),(0.,1.),(0.,0.0999999999999996),
 .UNSPECIFIED.);
#1433=B_SPLINE_SURFACE_WITH_KNOTS('',2,1,((#41855,#41856),(#41857,#41858),
(#41859,#41860)),.UNSPECIFIED.,.F.,.F.,.F.,(3,3),(2,2),(0.,1.),(0.,0.0999999999999996),
 .UNSPECIFIED.);
#1434=B_SPLINE_SURFACE_WITH_KNOTS('',2,1,((#41866,#41867),(#41868,#41869),
(#41870,#41871)),.UNSPECIFIED.,.F.,.F.,.F.,(3,3),(2,2),(0.,1.),(0.,0.0999999999999996),
 .UNSPECIFIED.);
#1435=B_SPLINE_SURFACE_WITH_KNOTS('',2,1,((#41877,#41878),(#41879,#41880),
(#41881,#41882)),.UNSPECIFIED.,.F.,.F.,.F.,(3,3),(2,2),(0.,1.),(0.,0.0999999999999996),
 .UNSPECIFIED.);
#1436=B_SPLINE_SURFACE_WITH_KNOTS('',2,1,((#41893,#41894),(#41895,#41896),
(#41897,#41898)),.UNSPECIFIED.,.F.,.F.,.F.,(3,3),(2,2),(0.,1.),(0.,0.0999999999999996),
 .UNSPECIFIED.);
#1437=B_SPLINE_SURFACE_WITH_KNOTS('',2,1,((#41904,#41905),(#41906,#41907),
(#41908,#41909)),.UNSPECIFIED.,.F.,.F.,.F.,(3,3),(2,2),(0.,1.),(0.,0.0999999999999996),
 .UNSPECIFIED.);
#1438=B_SPLINE_SURFACE_WITH_KNOTS('',2,1,((#41915,#41916),(#41917,#41918),
(#41919,#41920)),.UNSPECIFIED.,.F.,.F.,.F.,(3,3),(2,2),(0.,1.),(0.,0.0999999999999996),
 .UNSPECIFIED.);
#1439=B_SPLINE_SURFACE_WITH_KNOTS('',2,1,((#41926,#41927),(#41928,#41929),
(#41930,#41931)),.UNSPECIFIED.,.F.,.F.,.F.,(3,3),(2,2),(0.,1.),(0.,0.0999999999999996),
 .UNSPECIFIED.);
#1440=B_SPLINE_SURFACE_WITH_KNOTS('',2,1,((#41937,#41938),(#41939,#41940),
(#41941,#41942)),.UNSPECIFIED.,.F.,.F.,.F.,(3,3),(2,2),(0.,1.),(0.,0.0999999999999996),
 .UNSPECIFIED.);
#1441=B_SPLINE_SURFACE_WITH_KNOTS('',2,1,((#41948,#41949),(#41950,#41951),
(#41952,#41953)),.UNSPECIFIED.,.F.,.F.,.F.,(3,3),(2,2),(0.,1.),(0.,0.0999999999999996),
 .UNSPECIFIED.);
#1442=B_SPLINE_SURFACE_WITH_KNOTS('',2,1,((#41959,#41960),(#41961,#41962),
(#41963,#41964)),.UNSPECIFIED.,.F.,.F.,.F.,(3,3),(2,2),(0.,1.),(0.,0.0999999999999996),
 .UNSPECIFIED.);
#1443=B_SPLINE_SURFACE_WITH_KNOTS('',2,1,((#41970,#41971),(#41972,#41973),
(#41974,#41975)),.UNSPECIFIED.,.F.,.F.,.F.,(3,3),(2,2),(0.,1.),(0.,0.0999999999999996),
 .UNSPECIFIED.);
#1444=B_SPLINE_SURFACE_WITH_KNOTS('',2,1,((#41981,#41982),(#41983,#41984),
(#41985,#41986)),.UNSPECIFIED.,.F.,.F.,.F.,(3,3),(2,2),(0.,1.),(0.,0.0999999999999996),
 .UNSPECIFIED.);
#1445=B_SPLINE_SURFACE_WITH_KNOTS('',2,1,((#41992,#41993),(#41994,#41995),
(#41996,#41997)),.UNSPECIFIED.,.F.,.F.,.F.,(3,3),(2,2),(0.,1.),(0.,0.0999999999999996),
 .UNSPECIFIED.);
#1446=B_SPLINE_SURFACE_WITH_KNOTS('',2,1,((#42007,#42008),(#42009,#42010),
(#42011,#42012)),.UNSPECIFIED.,.F.,.F.,.F.,(3,3),(2,2),(0.,1.),(0.,0.0999999999999996),
 .UNSPECIFIED.);
#1447=B_SPLINE_SURFACE_WITH_KNOTS('',2,1,((#42018,#42019),(#42020,#42021),
(#42022,#42023)),.UNSPECIFIED.,.F.,.F.,.F.,(3,3),(2,2),(0.,1.),(0.,0.0999999999999996),
 .UNSPECIFIED.);
#1448=B_SPLINE_SURFACE_WITH_KNOTS('',2,1,((#42029,#42030),(#42031,#42032),
(#42033,#42034)),.UNSPECIFIED.,.F.,.F.,.F.,(3,3),(2,2),(0.,1.),(0.,0.0999999999999996),
 .UNSPECIFIED.);
#1449=B_SPLINE_SURFACE_WITH_KNOTS('',2,1,((#42040,#42041),(#42042,#42043),
(#42044,#42045)),.UNSPECIFIED.,.F.,.F.,.F.,(3,3),(2,2),(0.,1.),(0.,0.0999999999999996),
 .UNSPECIFIED.);
#1450=B_SPLINE_SURFACE_WITH_KNOTS('',2,1,((#42051,#42052),(#42053,#42054),
(#42055,#42056)),.UNSPECIFIED.,.F.,.F.,.F.,(3,3),(2,2),(0.,1.),(0.,0.0999999999999996),
 .UNSPECIFIED.);
#1451=B_SPLINE_SURFACE_WITH_KNOTS('',2,1,((#42062,#42063),(#42064,#42065),
(#42066,#42067)),.UNSPECIFIED.,.F.,.F.,.F.,(3,3),(2,2),(0.,1.),(0.,0.0999999999999996),
 .UNSPECIFIED.);
#1452=B_SPLINE_SURFACE_WITH_KNOTS('',2,1,((#42073,#42074),(#42075,#42076),
(#42077,#42078)),.UNSPECIFIED.,.F.,.F.,.F.,(3,3),(2,2),(0.,1.),(0.,0.0999999999999996),
 .UNSPECIFIED.);
#1453=B_SPLINE_SURFACE_WITH_KNOTS('',2,1,((#42084,#42085),(#42086,#42087),
(#42088,#42089)),.UNSPECIFIED.,.F.,.F.,.F.,(3,3),(2,2),(0.,1.),(0.,0.0999999999999996),
 .UNSPECIFIED.);
#1454=B_SPLINE_SURFACE_WITH_KNOTS('',3,3,((#45133,#45134,#45135,#45136,
#45137,#45138,#45139,#45140,#45141,#45142,#45143,#45144,#45145,#45146,#45147,
#45148,#45149,#45150,#45151,#45152,#45153,#45154,#45155,#45156,#45157,#45158,
#45159,#45160,#45161,#45162,#45163,#45164,#45165,#45166,#45167,#45168,#45169,
#45170,#45171,#45172,#45173,#45174,#45175,#45176,#45177,#45178,#45179,#45180,
#45181,#45182,#45183,#45184,#45185,#45186,#45187,#45188,#45189,#45190,#45191,
#45192,#45193,#45194,#45195),(#45196,#45197,#45198,#45199,#45200,#45201,
#45202,#45203,#45204,#45205,#45206,#45207,#45208,#45209,#45210,#45211,#45212,
#45213,#45214,#45215,#45216,#45217,#45218,#45219,#45220,#45221,#45222,#45223,
#45224,#45225,#45226,#45227,#45228,#45229,#45230,#45231,#45232,#45233,#45234,
#45235,#45236,#45237,#45238,#45239,#45240,#45241,#45242,#45243,#45244,#45245,
#45246,#45247,#45248,#45249,#45250,#45251,#45252,#45253,#45254,#45255,#45256,
#45257,#45258),(#45259,#45260,#45261,#45262,#45263,#45264,#45265,#45266,
#45267,#45268,#45269,#45270,#45271,#45272,#45273,#45274,#45275,#45276,#45277,
#45278,#45279,#45280,#45281,#45282,#45283,#45284,#45285,#45286,#45287,#45288,
#45289,#45290,#45291,#45292,#45293,#45294,#45295,#45296,#45297,#45298,#45299,
#45300,#45301,#45302,#45303,#45304,#45305,#45306,#45307,#45308,#45309,#45310,
#45311,#45312,#45313,#45314,#45315,#45316,#45317,#45318,#45319,#45320,#45321),
(#45322,#45323,#45324,#45325,#45326,#45327,#45328,#45329,#45330,#45331,
#45332,#45333,#45334,#45335,#45336,#45337,#45338,#45339,#45340,#45341,#45342,
#45343,#45344,#45345,#45346,#45347,#45348,#45349,#45350,#45351,#45352,#45353,
#45354,#45355,#45356,#45357,#45358,#45359,#45360,#45361,#45362,#45363,#45364,
#45365,#45366,#45367,#45368,#45369,#45370,#45371,#45372,#45373,#45374,#45375,
#45376,#45377,#45378,#45379,#45380,#45381,#45382,#45383,#45384)),
 .UNSPECIFIED.,.F.,.F.,.F.,(4,4),(4,1,1,1,1,1,1,1,1,1,1,1,1,1,1,1,1,1,1,
1,1,1,1,1,1,1,1,1,1,1,1,1,1,1,1,1,1,1,1,1,1,1,1,1,1,1,1,1,1,1,1,1,1,1,1,
1,1,1,1,1,4),(0.,0.231084445243146),(8.30203615430838,8.78540525698952,
9.26877435967066,9.7521434623518,10.2355125650329,10.7188816677141,11.2022507703952,
11.6856198730764,12.1689889757575,12.6523580784387,13.1357271811198,13.6190962838009,
14.1024653864821,14.5858344891632,15.0692035918444,15.5525726945255,16.0359417972066,
16.5193108998878,17.0026800025689,17.4860491052501,17.9694182079312,18.4527873106123,
18.9361564132935,19.4195255159746,19.9028946186558,20.3862637213369,20.8696328240181,
21.3530019266992,21.8363710293803,22.3197401320615,22.8031092347426,23.2864783374238,
23.7698474401049,24.253216542786,24.7365856454672,25.2199547481483,25.7033238508295,
26.1866929535106,26.6700620561917,27.1534311588729,27.636800261554,28.1201693642352,
28.6035384669163,29.0869075695975,29.5702766722786,30.0536457749597,30.5370148776409,
31.020383980322,31.5037530830032,31.9871221856843,32.4704912883655,32.9538603910466,
33.4372294937277,33.9205985964089,34.40396769909,34.8873368017712,35.3707059044523,
35.8540750071334,36.3374441098146,36.8208132124957,37.3041823151769),
 .UNSPECIFIED.);
#1455=B_SPLINE_SURFACE_WITH_KNOTS('',3,3,((#45606,#45607,#45608,#45609,
#45610,#45611,#45612,#45613,#45614,#45615,#45616,#45617,#45618,#45619,#45620,
#45621,#45622,#45623,#45624,#45625,#45626,#45627,#45628,#45629,#45630,#45631,
#45632,#45633,#45634,#45635,#45636,#45637,#45638,#45639,#45640,#45641,#45642,
#45643,#45644,#45645,#45646,#45647,#45648,#45649,#45650,#45651,#45652,#45653,
#45654,#45655,#45656,#45657,#45658,#45659,#45660,#45661,#45662,#45663,#45664,
#45665,#45666,#45667,#45668),(#45669,#45670,#45671,#45672,#45673,#45674,
#45675,#45676,#45677,#45678,#45679,#45680,#45681,#45682,#45683,#45684,#45685,
#45686,#45687,#45688,#45689,#45690,#45691,#45692,#45693,#45694,#45695,#45696,
#45697,#45698,#45699,#45700,#45701,#45702,#45703,#45704,#45705,#45706,#45707,
#45708,#45709,#45710,#45711,#45712,#45713,#45714,#45715,#45716,#45717,#45718,
#45719,#45720,#45721,#45722,#45723,#45724,#45725,#45726,#45727,#45728,#45729,
#45730,#45731),(#45732,#45733,#45734,#45735,#45736,#45737,#45738,#45739,
#45740,#45741,#45742,#45743,#45744,#45745,#45746,#45747,#45748,#45749,#45750,
#45751,#45752,#45753,#45754,#45755,#45756,#45757,#45758,#45759,#45760,#45761,
#45762,#45763,#45764,#45765,#45766,#45767,#45768,#45769,#45770,#45771,#45772,
#45773,#45774,#45775,#45776,#45777,#45778,#45779,#45780,#45781,#45782,#45783,
#45784,#45785,#45786,#45787,#45788,#45789,#45790,#45791,#45792,#45793,#45794),
(#45795,#45796,#45797,#45798,#45799,#45800,#45801,#45802,#45803,#45804,
#45805,#45806,#45807,#45808,#45809,#45810,#45811,#45812,#45813,#45814,#45815,
#45816,#45817,#45818,#45819,#45820,#45821,#45822,#45823,#45824,#45825,#45826,
#45827,#45828,#45829,#45830,#45831,#45832,#45833,#45834,#45835,#45836,#45837,
#45838,#45839,#45840,#45841,#45842,#45843,#45844,#45845,#45846,#45847,#45848,
#45849,#45850,#45851,#45852,#45853,#45854,#45855,#45856,#45857)),
 .UNSPECIFIED.,.F.,.F.,.F.,(4,4),(4,1,1,1,1,1,1,1,1,1,1,1,1,1,1,1,1,1,1,
1,1,1,1,1,1,1,1,1,1,1,1,1,1,1,1,1,1,1,1,1,1,1,1,1,1,1,1,1,1,1,1,1,1,1,1,
1,1,1,1,1,4),(0.,0.231084445243146),(11.614903290721,12.0982723934021,12.5816414960833,
13.0650105987644,13.5483797014456,14.0317488041267,14.5151179068079,14.998487009489,
15.4818561121702,15.9652252148513,16.4485943175325,16.9319634202136,17.4153325228947,
17.8987016255759,18.382070728257,18.8654398309382,19.3488089336193,19.8321780363005,
20.3155471389816,20.7989162416628,21.2822853443439,21.765654447025,22.2490235497062,
22.7323926523873,23.2157617550685,23.6991308577496,24.1824999604308,24.6658690631119,
25.1492381657931,25.6326072684742,26.1159763711553,26.5993454738365,27.0827145765176,
27.5660836791988,28.0494527818799,28.5328218845611,29.0161909872422,29.4995600899234,
29.9829291926045,30.4662982952857,30.9496673979668,31.4330365006479,31.9164056033291,
32.3997747060102,32.8831438086914,33.3665129113725,33.8498820140537,34.3332511167348,
34.816620219416,35.2999893220971,35.7833584247782,36.2667275274594,36.7500966301405,
37.2334657328217,37.7168348355028,38.200203938184,38.6835730408651,39.1669421435463,
39.6503112462274,40.1336803489085,40.6170494515897),.UNSPECIFIED.);
#1456=B_SPLINE_SURFACE_WITH_KNOTS('',3,3,((#47547,#47548,#47549,#47550,
#47551,#47552,#47553,#47554,#47555,#47556,#47557,#47558,#47559,#47560,#47561,
#47562,#47563,#47564,#47565,#47566,#47567,#47568,#47569,#47570,#47571,#47572,
#47573,#47574,#47575,#47576,#47577,#47578,#47579,#47580,#47581,#47582,#47583,
#47584,#47585,#47586,#47587,#47588,#47589,#47590,#47591,#47592,#47593,#47594,
#47595,#47596,#47597,#47598,#47599,#47600,#47601,#47602,#47603,#47604,#47605,
#47606,#47607,#47608,#47609,#47610,#47611,#47612,#47613,#47614,#47615,#47616,
#47617,#47618,#47619,#47620,#47621,#47622,#47623,#47624,#47625,#47626,#47627,
#47628,#47629,#47630,#47631,#47632,#47633,#47634,#47635,#47636,#47637,#47638,
#47639,#47640,#47641,#47642,#47643,#47644,#47645,#47646,#47647),(#47648,
#47649,#47650,#47651,#47652,#47653,#47654,#47655,#47656,#47657,#47658,#47659,
#47660,#47661,#47662,#47663,#47664,#47665,#47666,#47667,#47668,#47669,#47670,
#47671,#47672,#47673,#47674,#47675,#47676,#47677,#47678,#47679,#47680,#47681,
#47682,#47683,#47684,#47685,#47686,#47687,#47688,#47689,#47690,#47691,#47692,
#47693,#47694,#47695,#47696,#47697,#47698,#47699,#47700,#47701,#47702,#47703,
#47704,#47705,#47706,#47707,#47708,#47709,#47710,#47711,#47712,#47713,#47714,
#47715,#47716,#47717,#47718,#47719,#47720,#47721,#47722,#47723,#47724,#47725,
#47726,#47727,#47728,#47729,#47730,#47731,#47732,#47733,#47734,#47735,#47736,
#47737,#47738,#47739,#47740,#47741,#47742,#47743,#47744,#47745,#47746,#47747,
#47748),(#47749,#47750,#47751,#47752,#47753,#47754,#47755,#47756,#47757,
#47758,#47759,#47760,#47761,#47762,#47763,#47764,#47765,#47766,#47767,#47768,
#47769,#47770,#47771,#47772,#47773,#47774,#47775,#47776,#47777,#47778,#47779,
#47780,#47781,#47782,#47783,#47784,#47785,#47786,#47787,#47788,#47789,#47790,
#47791,#47792,#47793,#47794,#47795,#47796,#47797,#47798,#47799,#47800,#47801,
#47802,#47803,#47804,#47805,#47806,#47807,#47808,#47809,#47810,#47811,#47812,
#47813,#47814,#47815,#47816,#47817,#47818,#47819,#47820,#47821,#47822,#47823,
#47824,#47825,#47826,#47827,#47828,#47829,#47830,#47831,#47832,#47833,#47834,
#47835,#47836,#47837,#47838,#47839,#47840,#47841,#47842,#47843,#47844,#47845,
#47846,#47847,#47848,#47849),(#47850,#47851,#47852,#47853,#47854,#47855,
#47856,#47857,#47858,#47859,#47860,#47861,#47862,#47863,#47864,#47865,#47866,
#47867,#47868,#47869,#47870,#47871,#47872,#47873,#47874,#47875,#47876,#47877,
#47878,#47879,#47880,#47881,#47882,#47883,#47884,#47885,#47886,#47887,#47888,
#47889,#47890,#47891,#47892,#47893,#47894,#47895,#47896,#47897,#47898,#47899,
#47900,#47901,#47902,#47903,#47904,#47905,#47906,#47907,#47908,#47909,#47910,
#47911,#47912,#47913,#47914,#47915,#47916,#47917,#47918,#47919,#47920,#47921,
#47922,#47923,#47924,#47925,#47926,#47927,#47928,#47929,#47930,#47931,#47932,
#47933,#47934,#47935,#47936,#47937,#47938,#47939,#47940,#47941,#47942,#47943,
#47944,#47945,#47946,#47947,#47948,#47949,#47950)),.UNSPECIFIED.,.F.,.F.,
 .F.,(4,4),(4,1,1,1,1,1,1,1,1,1,1,1,1,1,1,1,1,1,1,1,1,1,1,1,1,1,1,1,1,1,
1,1,1,1,1,1,1,1,1,1,1,1,1,1,1,1,1,1,1,1,1,1,1,1,1,1,1,1,1,1,1,1,1,1,1,1,
1,1,1,1,1,1,1,1,1,1,1,1,1,1,1,1,1,1,1,1,1,1,1,1,1,1,1,1,1,1,1,1,4),(0.,
0.0820126057383864),(8.31473274985782,8.81155109817156,9.3083694464853,
10.3020061431128,11.2956428397403,12.2892795363678,13.2829162329952,14.2765529296227,
15.2701896262502,16.2638263228777,17.2574630195052,18.2510997161327,19.2447364127602,
20.2383731093876,21.2320098060151,22.2256465026426,23.2192831992701,24.2129198958976,
25.2065565925251,26.2001932891526,27.19382998578,28.1874666824075,29.181103379035,
30.1747400756625,31.16837677229,32.1620134689175,33.155650165545,34.1492868621724,
35.1429235587999,36.1365602554274,37.1301969520549,38.1238336486824,39.1174703453099,
40.1111070419373,41.1047437385648,42.0983804351923,43.0920171318198,44.0856538284473,
45.0792905250748,46.0729272217023,47.0665639183297,48.0602006149572,49.0538373115847,
50.0474740082122,51.0411107048397,52.0347474014672,53.0283840980947,54.0220207947221,
55.0156574913496,56.0092941879771,57.0029308846046,57.9965675812321,58.9902042778596,
59.9838409744871,60.9774776711145,61.971114367742,62.9647510643695,63.958387760997,
64.9520244576245,65.945661154252,66.9392978508795,67.9329345475069,68.9265712441344,
69.9202079407619,70.9138446373894,71.9074813340169,72.9011180306444,73.8947547272718,
74.8883914238993,75.8820281205268,76.8756648171543,77.8693015137818,78.8629382104093,
79.8565749070368,80.8502116036642,81.8438483002917,82.8374849969192,83.8311216935467,
84.8247583901742,85.8183950868017,86.8120317834291,87.8056684800567,88.7993051766841,
89.7929418733116,90.7865785699391,91.7802152665666,92.7738519631941,93.7674886598216,
94.761125356449,95.7547620530765,96.748398749704,97.7420354463315,98.735672142959,
99.7293088395865,100.722945536214,101.716582232841,102.710218929469,103.207037277783,
103.703855626096),.UNSPECIFIED.);
#1457=B_SPLINE_SURFACE_WITH_KNOTS('',3,3,((#48186,#48187,#48188,#48189,
#48190,#48191,#48192,#48193,#48194,#48195,#48196,#48197,#48198,#48199,#48200,
#48201,#48202,#48203,#48204,#48205,#48206,#48207,#48208,#48209,#48210,#48211,
#48212,#48213,#48214,#48215,#48216,#48217,#48218,#48219,#48220,#48221,#48222,
#48223,#48224,#48225,#48226,#48227,#48228,#48229,#48230,#48231,#48232,#48233,
#48234,#48235,#48236,#48237,#48238,#48239,#48240,#48241,#48242,#48243,#48244,
#48245,#48246,#48247,#48248,#48249,#48250,#48251,#48252,#48253,#48254,#48255,
#48256,#48257,#48258,#48259,#48260,#48261,#48262,#48263,#48264,#48265,#48266,
#48267,#48268,#48269,#48270,#48271,#48272,#48273,#48274,#48275,#48276,#48277,
#48278,#48279,#48280,#48281,#48282,#48283,#48284,#48285,#48286),(#48287,
#48288,#48289,#48290,#48291,#48292,#48293,#48294,#48295,#48296,#48297,#48298,
#48299,#48300,#48301,#48302,#48303,#48304,#48305,#48306,#48307,#48308,#48309,
#48310,#48311,#48312,#48313,#48314,#48315,#48316,#48317,#48318,#48319,#48320,
#48321,#48322,#48323,#48324,#48325,#48326,#48327,#48328,#48329,#48330,#48331,
#48332,#48333,#48334,#48335,#48336,#48337,#48338,#48339,#48340,#48341,#48342,
#48343,#48344,#48345,#48346,#48347,#48348,#48349,#48350,#48351,#48352,#48353,
#48354,#48355,#48356,#48357,#48358,#48359,#48360,#48361,#48362,#48363,#48364,
#48365,#48366,#48367,#48368,#48369,#48370,#48371,#48372,#48373,#48374,#48375,
#48376,#48377,#48378,#48379,#48380,#48381,#48382,#48383,#48384,#48385,#48386,
#48387),(#48388,#48389,#48390,#48391,#48392,#48393,#48394,#48395,#48396,
#48397,#48398,#48399,#48400,#48401,#48402,#48403,#48404,#48405,#48406,#48407,
#48408,#48409,#48410,#48411,#48412,#48413,#48414,#48415,#48416,#48417,#48418,
#48419,#48420,#48421,#48422,#48423,#48424,#48425,#48426,#48427,#48428,#48429,
#48430,#48431,#48432,#48433,#48434,#48435,#48436,#48437,#48438,#48439,#48440,
#48441,#48442,#48443,#48444,#48445,#48446,#48447,#48448,#48449,#48450,#48451,
#48452,#48453,#48454,#48455,#48456,#48457,#48458,#48459,#48460,#48461,#48462,
#48463,#48464,#48465,#48466,#48467,#48468,#48469,#48470,#48471,#48472,#48473,
#48474,#48475,#48476,#48477,#48478,#48479,#48480,#48481,#48482,#48483,#48484,
#48485,#48486,#48487,#48488),(#48489,#48490,#48491,#48492,#48493,#48494,
#48495,#48496,#48497,#48498,#48499,#48500,#48501,#48502,#48503,#48504,#48505,
#48506,#48507,#48508,#48509,#48510,#48511,#48512,#48513,#48514,#48515,#48516,
#48517,#48518,#48519,#48520,#48521,#48522,#48523,#48524,#48525,#48526,#48527,
#48528,#48529,#48530,#48531,#48532,#48533,#48534,#48535,#48536,#48537,#48538,
#48539,#48540,#48541,#48542,#48543,#48544,#48545,#48546,#48547,#48548,#48549,
#48550,#48551,#48552,#48553,#48554,#48555,#48556,#48557,#48558,#48559,#48560,
#48561,#48562,#48563,#48564,#48565,#48566,#48567,#48568,#48569,#48570,#48571,
#48572,#48573,#48574,#48575,#48576,#48577,#48578,#48579,#48580,#48581,#48582,
#48583,#48584,#48585,#48586,#48587,#48588,#48589)),.UNSPECIFIED.,.F.,.F.,
 .F.,(4,4),(4,1,1,1,1,1,1,1,1,1,1,1,1,1,1,1,1,1,1,1,1,1,1,1,1,1,1,1,1,1,
1,1,1,1,1,1,1,1,1,1,1,1,1,1,1,1,1,1,1,1,1,1,1,1,1,1,1,1,1,1,1,1,1,1,1,1,
1,1,1,1,1,1,1,1,1,1,1,1,1,1,1,1,1,1,1,1,1,1,1,1,1,1,1,1,1,1,1,1,4),(0.,
0.0820126057383864),(11.6152142277545,12.1120325760682,12.608850924382,
13.6024876210095,14.5961243176369,15.5897610142644,16.5833977108919,17.5770344075194,
18.5706711041469,19.5643078007744,20.5579444974019,21.5515811940293,22.5452178906568,
23.5388545872843,24.5324912839118,25.5261279805393,26.5197646771668,27.5134013737943,
28.5070380704217,29.5006747670492,30.4943114636767,31.4879481603042,32.4815848569317,
33.4752215535592,34.4688582501867,35.4624949468141,36.4561316434416,37.4497683400691,
38.4434050366966,39.4370417333241,40.4306784299516,41.4243151265791,42.4179518232065,
43.411588519834,44.4052252164615,45.398861913089,46.3924986097165,47.386135306344,
48.3797720029714,49.3734086995989,50.3670453962264,51.3606820928539,52.3543187894814,
53.3479554861089,54.3415921827364,55.3352288793638,56.3288655759913,57.3225022726188,
58.3161389692463,59.3097756658738,60.3034123625013,61.2970490591288,62.2906857557562,
63.2843224523837,64.2779591490112,65.2715958456387,66.2652325422662,67.2588692388937,
68.2525059355212,69.2461426321486,70.2397793287761,71.2334160254036,72.2270527220311,
73.2206894186586,74.2143261152861,75.2079628119136,76.201599508541,77.1952362051685,
78.188872901796,79.1825095984235,80.176146295051,81.1697829916785,82.163419688306,
83.1570563849334,84.1506930815609,85.1443297781884,86.1379664748159,87.1316031714434,
88.1252398680709,89.1188765646984,90.1125132613258,91.1061499579533,92.0997866545808,
93.0934233512083,94.0870600478358,95.0806967444633,96.0743334410907,97.0679701377182,
98.0616068343457,99.0552435309732,100.048880227601,101.042516924228,102.036153620856,
103.029790317483,104.023427014111,105.017063710738,106.010700407366,106.507518755679,
107.004337103993),.UNSPECIFIED.);
#1458=B_SPLINE_SURFACE_WITH_KNOTS('',3,3,((#49135,#49136,#49137,#49138,
#49139,#49140,#49141,#49142,#49143,#49144,#49145,#49146,#49147,#49148,#49149,
#49150,#49151,#49152,#49153,#49154,#49155,#49156,#49157,#49158,#49159,#49160,
#49161,#49162,#49163,#49164,#49165),(#49166,#49167,#49168,#49169,#49170,
#49171,#49172,#49173,#49174,#49175,#49176,#49177,#49178,#49179,#49180,#49181,
#49182,#49183,#49184,#49185,#49186,#49187,#49188,#49189,#49190,#49191,#49192,
#49193,#49194,#49195,#49196),(#49197,#49198,#49199,#49200,#49201,#49202,
#49203,#49204,#49205,#49206,#49207,#49208,#49209,#49210,#49211,#49212,#49213,
#49214,#49215,#49216,#49217,#49218,#49219,#49220,#49221,#49222,#49223,#49224,
#49225,#49226,#49227),(#49228,#49229,#49230,#49231,#49232,#49233,#49234,
#49235,#49236,#49237,#49238,#49239,#49240,#49241,#49242,#49243,#49244,#49245,
#49246,#49247,#49248,#49249,#49250,#49251,#49252,#49253,#49254,#49255,#49256,
#49257,#49258)),.UNSPECIFIED.,.F.,.T.,.F.,(4,4),(4,2,2,2,2,2,2,1,1,1,2,
2,2,2,2,2,4),(0.,1.),(0.,0.094448813972548,0.188897627945096,0.283341149511147,
0.377784671077197,0.472228192643248,0.566671714209298,0.661120528181846,
0.755569342154394,0.850018156126942,0.94446697009949,1.03891049166554,1.13335401323159,
1.22779753479764,1.32224105636369,1.41668987033624,1.51113868430879),
 .UNSPECIFIED.);
#1459=B_SPLINE_SURFACE_WITH_KNOTS('',3,3,((#49404,#49405,#49406,#49407,
#49408,#49409,#49410,#49411,#49412,#49413,#49414,#49415,#49416,#49417,#49418,
#49419,#49420,#49421,#49422,#49423,#49424,#49425,#49426,#49427,#49428,#49429,
#49430,#49431,#49432,#49433,#49434),(#49435,#49436,#49437,#49438,#49439,
#49440,#49441,#49442,#49443,#49444,#49445,#49446,#49447,#49448,#49449,#49450,
#49451,#49452,#49453,#49454,#49455,#49456,#49457,#49458,#49459,#49460,#49461,
#49462,#49463,#49464,#49465),(#49466,#49467,#49468,#49469,#49470,#49471,
#49472,#49473,#49474,#49475,#49476,#49477,#49478,#49479,#49480,#49481,#49482,
#49483,#49484,#49485,#49486,#49487,#49488,#49489,#49490,#49491,#49492,#49493,
#49494,#49495,#49496),(#49497,#49498,#49499,#49500,#49501,#49502,#49503,
#49504,#49505,#49506,#49507,#49508,#49509,#49510,#49511,#49512,#49513,#49514,
#49515,#49516,#49517,#49518,#49519,#49520,#49521,#49522,#49523,#49524,#49525,
#49526,#49527)),.UNSPECIFIED.,.F.,.T.,.F.,(4,4),(4,2,2,1,2,2,2,1,1,1,1,
2,2,2,2,2,2,4),(0.,1.),(0.,0.094448813972548,0.283341149511147,0.330562910294172,
0.377784671077197,0.472228192643248,0.566671714209298,0.661120528181846,
0.755569342154394,0.779181545647531,0.850018156126942,0.94446697009949,
1.03891049166554,1.13335401323159,1.22779753479764,1.32224105636369,1.41668987033624,
1.51113868430879),.UNSPECIFIED.);
#1460=B_SPLINE_SURFACE_WITH_KNOTS('',3,3,((#49636,#49637,#49638,#49639,
#49640,#49641,#49642,#49643,#49644,#49645,#49646,#49647,#49648,#49649,#49650,
#49651,#49652,#49653,#49654,#49655,#49656,#49657,#49658,#49659,#49660,#49661,
#49662,#49663,#49664,#49665),(#49666,#49667,#49668,#49669,#49670,#49671,
#49672,#49673,#49674,#49675,#49676,#49677,#49678,#49679,#49680,#49681,#49682,
#49683,#49684,#49685,#49686,#49687,#49688,#49689,#49690,#49691,#49692,#49693,
#49694,#49695),(#49696,#49697,#49698,#49699,#49700,#49701,#49702,#49703,
#49704,#49705,#49706,#49707,#49708,#49709,#49710,#49711,#49712,#49713,#49714,
#49715,#49716,#49717,#49718,#49719,#49720,#49721,#49722,#49723,#49724,#49725),
(#49726,#49727,#49728,#49729,#49730,#49731,#49732,#49733,#49734,#49735,
#49736,#49737,#49738,#49739,#49740,#49741,#49742,#49743,#49744,#49745,#49746,
#49747,#49748,#49749,#49750,#49751,#49752,#49753,#49754,#49755),(#49756,
#49757,#49758,#49759,#49760,#49761,#49762,#49763,#49764,#49765,#49766,#49767,
#49768,#49769,#49770,#49771,#49772,#49773,#49774,#49775,#49776,#49777,#49778,
#49779,#49780,#49781,#49782,#49783,#49784,#49785),(#49786,#49787,#49788,
#49789,#49790,#49791,#49792,#49793,#49794,#49795,#49796,#49797,#49798,#49799,
#49800,#49801,#49802,#49803,#49804,#49805,#49806,#49807,#49808,#49809,#49810,
#49811,#49812,#49813,#49814,#49815),(#49816,#49817,#49818,#49819,#49820,
#49821,#49822,#49823,#49824,#49825,#49826,#49827,#49828,#49829,#49830,#49831,
#49832,#49833,#49834,#49835,#49836,#49837,#49838,#49839,#49840,#49841,#49842,
#49843,#49844,#49845),(#49846,#49847,#49848,#49849,#49850,#49851,#49852,
#49853,#49854,#49855,#49856,#49857,#49858,#49859,#49860,#49861,#49862,#49863,
#49864,#49865,#49866,#49867,#49868,#49869,#49870,#49871,#49872,#49873,#49874,
#49875),(#49876,#49877,#49878,#49879,#49880,#49881,#49882,#49883,#49884,
#49885,#49886,#49887,#49888,#49889,#49890,#49891,#49892,#49893,#49894,#49895,
#49896,#49897,#49898,#49899,#49900,#49901,#49902,#49903,#49904,#49905),
(#49906,#49907,#49908,#49909,#49910,#49911,#49912,#49913,#49914,#49915,
#49916,#49917,#49918,#49919,#49920,#49921,#49922,#49923,#49924,#49925,#49926,
#49927,#49928,#49929,#49930,#49931,#49932,#49933,#49934,#49935),(#49936,
#49937,#49938,#49939,#49940,#49941,#49942,#49943,#49944,#49945,#49946,#49947,
#49948,#49949,#49950,#49951,#49952,#49953,#49954,#49955,#49956,#49957,#49958,
#49959,#49960,#49961,#49962,#49963,#49964,#49965)),.UNSPECIFIED.,.T.,.F.,
 .F.,(4,1,1,1,1,1,1,1,4),(4,1,1,1,1,1,1,1,1,1,1,1,1,1,1,1,1,1,1,1,1,1,1,
1,1,1,1,4),(-3.14159265358979,-2.69279370307697,-2.24399475256414,-1.34639685153848,
-0.448798950512828,0.448798950512828,1.34639685153848,2.24399475256414,
3.14159265358979),(0.,0.0714285714285714,0.142857142857143,0.19047619047619,
0.238095238095238,0.285714285714286,0.30952380952381,0.333333333333333,
0.357142857142857,0.380952380952381,0.404761904761905,0.428571428571429,
0.464285714285714,0.5,0.535714285714286,0.571428571428571,0.607142857142857,
0.642857142857143,0.678571428571428,0.714285714285714,0.767857142857143,
0.785714285714286,0.821428571428571,0.857142857142857,0.892857142857143,
0.928571428571429,0.964285714285714,1.),.UNSPECIFIED.);
#1461=B_SPLINE_SURFACE_WITH_KNOTS('',3,3,((#50966,#50967,#50968,#50969,
#50970,#50971,#50972,#50973,#50974,#50975,#50976,#50977,#50978,#50979,#50980,
#50981,#50982,#50983,#50984,#50985,#50986,#50987,#50988,#50989,#50990,#50991,
#50992,#50993,#50994,#50995,#50996,#50997,#50998,#50999,#51000,#51001,#51002,
#51003,#51004,#51005,#51006,#51007,#51008,#51009,#51010,#51011,#51012,#51013,
#51014,#51015,#51016,#51017,#51018,#51019,#51020,#51021,#51022,#51023,#51024,
#51025,#51026,#51027,#51028,#51029,#51030,#51031,#51032,#51033,#51034,#51035,
#51036,#51037,#51038,#51039,#51040,#51041,#51042,#51043,#51044,#51045,#51046,
#51047,#51048,#51049,#51050,#51051,#51052,#51053,#51054,#51055,#51056,#51057,
#51058,#51059,#51060,#51061,#51062,#51063,#51064,#51065,#51066,#51067,#51068,
#51069,#51070,#51071,#51072,#51073,#51074,#51075,#51076,#51077,#51078,#51079,
#51080,#51081,#51082,#51083,#51084,#51085,#51086,#51087,#51088,#51089,#51090,
#51091,#51092,#51093,#51094,#51095,#51096,#51097,#51098,#51099,#51100,#51101,
#51102,#51103,#51104,#51105,#51106,#51107,#51108,#51109,#51110,#51111,#51112,
#51113,#51114,#51115,#51116,#51117,#51118,#51119,#51120,#51121,#51122,#51123,
#51124,#51125,#51126,#51127,#51128,#51129,#51130,#51131,#51132,#51133,#51134,
#51135,#51136,#51137,#51138,#51139,#51140,#51141,#51142,#51143,#51144,#51145,
#51146,#51147,#51148,#51149,#51150,#51151,#51152,#51153,#51154,#51155,#51156,
#51157,#51158,#51159,#51160,#51161,#51162,#51163,#51164,#51165,#51166,#51167,
#51168,#51169,#51170,#51171,#51172,#51173,#51174,#51175,#51176,#51177,#51178,
#51179,#51180,#51181,#51182,#51183,#51184,#51185,#51186,#51187,#51188,#51189,
#51190,#51191,#51192,#51193,#51194,#51195,#51196,#51197,#51198,#51199,#51200,
#51201,#51202,#51203,#51204,#51205,#51206,#51207,#51208,#51209,#51210,#51211,
#51212,#51213,#51214,#51215,#51216,#51217,#51218,#51219,#51220,#51221,#51222,
#51223,#51224,#51225,#51226,#51227,#51228,#51229,#51230,#51231,#51232,#51233,
#51234,#51235,#51236,#51237,#51238,#51239,#51240,#51241,#51242,#51243,#51244,
#51245,#51246,#51247,#51248,#51249,#51250,#51251,#51252,#51253,#51254,#51255,
#51256,#51257,#51258,#51259,#51260,#51261,#51262,#51263,#51264,#51265,#51266,
#51267,#51268,#51269,#51270,#51271,#51272,#51273,#51274,#51275,#51276,#51277,
#51278,#51279,#51280,#51281,#51282,#51283,#51284,#51285,#51286,#51287,#51288,
#51289,#51290,#51291,#51292,#51293,#51294,#51295,#51296,#51297,#51298,#51299,
#51300,#51301,#51302,#51303,#51304,#51305,#51306,#51307,#51308,#51309,#51310,
#51311,#51312,#51313,#51314,#51315,#51316,#51317,#51318,#51319,#51320,#51321,
#51322,#51323,#51324,#51325,#51326,#51327,#51328,#51329,#51330,#51331,#51332,
#51333,#51334,#51335,#51336,#51337,#51338,#51339,#51340,#51341,#51342,#51343,
#51344,#51345,#51346,#51347,#51348,#51349,#51350,#51351,#51352,#51353,#51354,
#51355,#51356,#51357,#51358,#51359,#51360,#51361,#51362,#51363,#51364,#51365,
#51366,#51367,#51368,#51369,#51370,#51371,#51372,#51373,#51374,#51375,#51376,
#51377,#51378,#51379,#51380,#51381,#51382,#51383,#51384,#51385,#51386,#51387,
#51388,#51389,#51390,#51391,#51392,#51393,#51394,#51395,#51396,#51397,#51398,
#51399,#51400,#51401,#51402,#51403,#51404,#51405,#51406,#51407,#51408,#51409,
#51410,#51411,#51412,#51413,#51414,#51415,#51416,#51417,#51418,#51419,#51420,
#51421,#51422,#51423,#51424,#51425,#51426,#51427,#51428,#51429,#51430,#51431,
#51432,#51433,#51434,#51435,#51436,#51437,#51438,#51439,#51440,#51441,#51442,
#51443,#51444,#51445,#51446,#51447,#51448,#51449,#51450,#51451,#51452,#51453,
#51454,#51455,#51456,#51457,#51458,#51459,#51460,#51461,#51462,#51463,#51464,
#51465,#51466,#51467),(#51468,#51469,#51470,#51471,#51472,#51473,#51474,
#51475,#51476,#51477,#51478,#51479,#51480,#51481,#51482,#51483,#51484,#51485,
#51486,#51487,#51488,#51489,#51490,#51491,#51492,#51493,#51494,#51495,#51496,
#51497,#51498,#51499,#51500,#51501,#51502,#51503,#51504,#51505,#51506,#51507,
#51508,#51509,#51510,#51511,#51512,#51513,#51514,#51515,#51516,#51517,#51518,
#51519,#51520,#51521,#51522,#51523,#51524,#51525,#51526,#51527,#51528,#51529,
#51530,#51531,#51532,#51533,#51534,#51535,#51536,#51537,#51538,#51539,#51540,
#51541,#51542,#51543,#51544,#51545,#51546,#51547,#51548,#51549,#51550,#51551,
#51552,#51553,#51554,#51555,#51556,#51557,#51558,#51559,#51560,#51561,#51562,
#51563,#51564,#51565,#51566,#51567,#51568,#51569,#51570,#51571,#51572,#51573,
#51574,#51575,#51576,#51577,#51578,#51579,#51580,#51581,#51582,#51583,#51584,
#51585,#51586,#51587,#51588,#51589,#51590,#51591,#51592,#51593,#51594,#51595,
#51596,#51597,#51598,#51599,#51600,#51601,#51602,#51603,#51604,#51605,#51606,
#51607,#51608,#51609,#51610,#51611,#51612,#51613,#51614,#51615,#51616,#51617,
#51618,#51619,#51620,#51621,#51622,#51623,#51624,#51625,#51626,#51627,#51628,
#51629,#51630,#51631,#51632,#51633,#51634,#51635,#51636,#51637,#51638,#51639,
#51640,#51641,#51642,#51643,#51644,#51645,#51646,#51647,#51648,#51649,#51650,
#51651,#51652,#51653,#51654,#51655,#51656,#51657,#51658,#51659,#51660,#51661,
#51662,#51663,#51664,#51665,#51666,#51667,#51668,#51669,#51670,#51671,#51672,
#51673,#51674,#51675,#51676,#51677,#51678,#51679,#51680,#51681,#51682,#51683,
#51684,#51685,#51686,#51687,#51688,#51689,#51690,#51691,#51692,#51693,#51694,
#51695,#51696,#51697,#51698,#51699,#51700,#51701,#51702,#51703,#51704,#51705,
#51706,#51707,#51708,#51709,#51710,#51711,#51712,#51713,#51714,#51715,#51716,
#51717,#51718,#51719,#51720,#51721,#51722,#51723,#51724,#51725,#51726,#51727,
#51728,#51729,#51730,#51731,#51732,#51733,#51734,#51735,#51736,#51737,#51738,
#51739,#51740,#51741,#51742,#51743,#51744,#51745,#51746,#51747,#51748,#51749,
#51750,#51751,#51752,#51753,#51754,#51755,#51756,#51757,#51758,#51759,#51760,
#51761,#51762,#51763,#51764,#51765,#51766,#51767,#51768,#51769,#51770,#51771,
#51772,#51773,#51774,#51775,#51776,#51777,#51778,#51779,#51780,#51781,#51782,
#51783,#51784,#51785,#51786,#51787,#51788,#51789,#51790,#51791,#51792,#51793,
#51794,#51795,#51796,#51797,#51798,#51799,#51800,#51801,#51802,#51803,#51804,
#51805,#51806,#51807,#51808,#51809,#51810,#51811,#51812,#51813,#51814,#51815,
#51816,#51817,#51818,#51819,#51820,#51821,#51822,#51823,#51824,#51825,#51826,
#51827,#51828,#51829,#51830,#51831,#51832,#51833,#51834,#51835,#51836,#51837,
#51838,#51839,#51840,#51841,#51842,#51843,#51844,#51845,#51846,#51847,#51848,
#51849,#51850,#51851,#51852,#51853,#51854,#51855,#51856,#51857,#51858,#51859,
#51860,#51861,#51862,#51863,#51864,#51865,#51866,#51867,#51868,#51869,#51870,
#51871,#51872,#51873,#51874,#51875,#51876,#51877,#51878,#51879,#51880,#51881,
#51882,#51883,#51884,#51885,#51886,#51887,#51888,#51889,#51890,#51891,#51892,
#51893,#51894,#51895,#51896,#51897,#51898,#51899,#51900,#51901,#51902,#51903,
#51904,#51905,#51906,#51907,#51908,#51909,#51910,#51911,#51912,#51913,#51914,
#51915,#51916,#51917,#51918,#51919,#51920,#51921,#51922,#51923,#51924,#51925,
#51926,#51927,#51928,#51929,#51930,#51931,#51932,#51933,#51934,#51935,#51936,
#51937,#51938,#51939,#51940,#51941,#51942,#51943,#51944,#51945,#51946,#51947,
#51948,#51949,#51950,#51951,#51952,#51953,#51954,#51955,#51956,#51957,#51958,
#51959,#51960,#51961,#51962,#51963,#51964,#51965,#51966,#51967,#51968,#51969),
(#51970,#51971,#51972,#51973,#51974,#51975,#51976,#51977,#51978,#51979,
#51980,#51981,#51982,#51983,#51984,#51985,#51986,#51987,#51988,#51989,#51990,
#51991,#51992,#51993,#51994,#51995,#51996,#51997,#51998,#51999,#52000,#52001,
#52002,#52003,#52004,#52005,#52006,#52007,#52008,#52009,#52010,#52011,#52012,
#52013,#52014,#52015,#52016,#52017,#52018,#52019,#52020,#52021,#52022,#52023,
#52024,#52025,#52026,#52027,#52028,#52029,#52030,#52031,#52032,#52033,#52034,
#52035,#52036,#52037,#52038,#52039,#52040,#52041,#52042,#52043,#52044,#52045,
#52046,#52047,#52048,#52049,#52050,#52051,#52052,#52053,#52054,#52055,#52056,
#52057,#52058,#52059,#52060,#52061,#52062,#52063,#52064,#52065,#52066,#52067,
#52068,#52069,#52070,#52071,#52072,#52073,#52074,#52075,#52076,#52077,#52078,
#52079,#52080,#52081,#52082,#52083,#52084,#52085,#52086,#52087,#52088,#52089,
#52090,#52091,#52092,#52093,#52094,#52095,#52096,#52097,#52098,#52099,#52100,
#52101,#52102,#52103,#52104,#52105,#52106,#52107,#52108,#52109,#52110,#52111,
#52112,#52113,#52114,#52115,#52116,#52117,#52118,#52119,#52120,#52121,#52122,
#52123,#52124,#52125,#52126,#52127,#52128,#52129,#52130,#52131,#52132,#52133,
#52134,#52135,#52136,#52137,#52138,#52139,#52140,#52141,#52142,#52143,#52144,
#52145,#52146,#52147,#52148,#52149,#52150,#52151,#52152,#52153,#52154,#52155,
#52156,#52157,#52158,#52159,#52160,#52161,#52162,#52163,#52164,#52165,#52166,
#52167,#52168,#52169,#52170,#52171,#52172,#52173,#52174,#52175,#52176,#52177,
#52178,#52179,#52180,#52181,#52182,#52183,#52184,#52185,#52186,#52187,#52188,
#52189,#52190,#52191,#52192,#52193,#52194,#52195,#52196,#52197,#52198,#52199,
#52200,#52201,#52202,#52203,#52204,#52205,#52206,#52207,#52208,#52209,#52210,
#52211,#52212,#52213,#52214,#52215,#52216,#52217,#52218,#52219,#52220,#52221,
#52222,#52223,#52224,#52225,#52226,#52227,#52228,#52229,#52230,#52231,#52232,
#52233,#52234,#52235,#52236,#52237,#52238,#52239,#52240,#52241,#52242,#52243,
#52244,#52245,#52246,#52247,#52248,#52249,#52250,#52251,#52252,#52253,#52254,
#52255,#52256,#52257,#52258,#52259,#52260,#52261,#52262,#52263,#52264,#52265,
#52266,#52267,#52268,#52269,#52270,#52271,#52272,#52273,#52274,#52275,#52276,
#52277,#52278,#52279,#52280,#52281,#52282,#52283,#52284,#52285,#52286,#52287,
#52288,#52289,#52290,#52291,#52292,#52293,#52294,#52295,#52296,#52297,#52298,
#52299,#52300,#52301,#52302,#52303,#52304,#52305,#52306,#52307,#52308,#52309,
#52310,#52311,#52312,#52313,#52314,#52315,#52316,#52317,#52318,#52319,#52320,
#52321,#52322,#52323,#52324,#52325,#52326,#52327,#52328,#52329,#52330,#52331,
#52332,#52333,#52334,#52335,#52336,#52337,#52338,#52339,#52340,#52341,#52342,
#52343,#52344,#52345,#52346,#52347,#52348,#52349,#52350,#52351,#52352,#52353,
#52354,#52355,#52356,#52357,#52358,#52359,#52360,#52361,#52362,#52363,#52364,
#52365,#52366,#52367,#52368,#52369,#52370,#52371,#52372,#52373,#52374,#52375,
#52376,#52377,#52378,#52379,#52380,#52381,#52382,#52383,#52384,#52385,#52386,
#52387,#52388,#52389,#52390,#52391,#52392,#52393,#52394,#52395,#52396,#52397,
#52398,#52399,#52400,#52401,#52402,#52403,#52404,#52405,#52406,#52407,#52408,
#52409,#52410,#52411,#52412,#52413,#52414,#52415,#52416,#52417,#52418,#52419,
#52420,#52421,#52422,#52423,#52424,#52425,#52426,#52427,#52428,#52429,#52430,
#52431,#52432,#52433,#52434,#52435,#52436,#52437,#52438,#52439,#52440,#52441,
#52442,#52443,#52444,#52445,#52446,#52447,#52448,#52449,#52450,#52451,#52452,
#52453,#52454,#52455,#52456,#52457,#52458,#52459,#52460,#52461,#52462,#52463,
#52464,#52465,#52466,#52467,#52468,#52469,#52470,#52471),(#52472,#52473,
#52474,#52475,#52476,#52477,#52478,#52479,#52480,#52481,#52482,#52483,#52484,
#52485,#52486,#52487,#52488,#52489,#52490,#52491,#52492,#52493,#52494,#52495,
#52496,#52497,#52498,#52499,#52500,#52501,#52502,#52503,#52504,#52505,#52506,
#52507,#52508,#52509,#52510,#52511,#52512,#52513,#52514,#52515,#52516,#52517,
#52518,#52519,#52520,#52521,#52522,#52523,#52524,#52525,#52526,#52527,#52528,
#52529,#52530,#52531,#52532,#52533,#52534,#52535,#52536,#52537,#52538,#52539,
#52540,#52541,#52542,#52543,#52544,#52545,#52546,#52547,#52548,#52549,#52550,
#52551,#52552,#52553,#52554,#52555,#52556,#52557,#52558,#52559,#52560,#52561,
#52562,#52563,#52564,#52565,#52566,#52567,#52568,#52569,#52570,#52571,#52572,
#52573,#52574,#52575,#52576,#52577,#52578,#52579,#52580,#52581,#52582,#52583,
#52584,#52585,#52586,#52587,#52588,#52589,#52590,#52591,#52592,#52593,#52594,
#52595,#52596,#52597,#52598,#52599,#52600,#52601,#52602,#52603,#52604,#52605,
#52606,#52607,#52608,#52609,#52610,#52611,#52612,#52613,#52614,#52615,#52616,
#52617,#52618,#52619,#52620,#52621,#52622,#52623,#52624,#52625,#52626,#52627,
#52628,#52629,#52630,#52631,#52632,#52633,#52634,#52635,#52636,#52637,#52638,
#52639,#52640,#52641,#52642,#52643,#52644,#52645,#52646,#52647,#52648,#52649,
#52650,#52651,#52652,#52653,#52654,#52655,#52656,#52657,#52658,#52659,#52660,
#52661,#52662,#52663,#52664,#52665,#52666,#52667,#52668,#52669,#52670,#52671,
#52672,#52673,#52674,#52675,#52676,#52677,#52678,#52679,#52680,#52681,#52682,
#52683,#52684,#52685,#52686,#52687,#52688,#52689,#52690,#52691,#52692,#52693,
#52694,#52695,#52696,#52697,#52698,#52699,#52700,#52701,#52702,#52703,#52704,
#52705,#52706,#52707,#52708,#52709,#52710,#52711,#52712,#52713,#52714,#52715,
#52716,#52717,#52718,#52719,#52720,#52721,#52722,#52723,#52724,#52725,#52726,
#52727,#52728,#52729,#52730,#52731,#52732,#52733,#52734,#52735,#52736,#52737,
#52738,#52739,#52740,#52741,#52742,#52743,#52744,#52745,#52746,#52747,#52748,
#52749,#52750,#52751,#52752,#52753,#52754,#52755,#52756,#52757,#52758,#52759,
#52760,#52761,#52762,#52763,#52764,#52765,#52766,#52767,#52768,#52769,#52770,
#52771,#52772,#52773,#52774,#52775,#52776,#52777,#52778,#52779,#52780,#52781,
#52782,#52783,#52784,#52785,#52786,#52787,#52788,#52789,#52790,#52791,#52792,
#52793,#52794,#52795,#52796,#52797,#52798,#52799,#52800,#52801,#52802,#52803,
#52804,#52805,#52806,#52807,#52808,#52809,#52810,#52811,#52812,#52813,#52814,
#52815,#52816,#52817,#52818,#52819,#52820,#52821,#52822,#52823,#52824,#52825,
#52826,#52827,#52828,#52829,#52830,#52831,#52832,#52833,#52834,#52835,#52836,
#52837,#52838,#52839,#52840,#52841,#52842,#52843,#52844,#52845,#52846,#52847,
#52848,#52849,#52850,#52851,#52852,#52853,#52854,#52855,#52856,#52857,#52858,
#52859,#52860,#52861,#52862,#52863,#52864,#52865,#52866,#52867,#52868,#52869,
#52870,#52871,#52872,#52873,#52874,#52875,#52876,#52877,#52878,#52879,#52880,
#52881,#52882,#52883,#52884,#52885,#52886,#52887,#52888,#52889,#52890,#52891,
#52892,#52893,#52894,#52895,#52896,#52897,#52898,#52899,#52900,#52901,#52902,
#52903,#52904,#52905,#52906,#52907,#52908,#52909,#52910,#52911,#52912,#52913,
#52914,#52915,#52916,#52917,#52918,#52919,#52920,#52921,#52922,#52923,#52924,
#52925,#52926,#52927,#52928,#52929,#52930,#52931,#52932,#52933,#52934,#52935,
#52936,#52937,#52938,#52939,#52940,#52941,#52942,#52943,#52944,#52945,#52946,
#52947,#52948,#52949,#52950,#52951,#52952,#52953,#52954,#52955,#52956,#52957,
#52958,#52959,#52960,#52961,#52962,#52963,#52964,#52965,#52966,#52967,#52968,
#52969,#52970,#52971,#52972,#52973),(#52974,#52975,#52976,#52977,#52978,
#52979,#52980,#52981,#52982,#52983,#52984,#52985,#52986,#52987,#52988,#52989,
#52990,#52991,#52992,#52993,#52994,#52995,#52996,#52997,#52998,#52999,#53000,
#53001,#53002,#53003,#53004,#53005,#53006,#53007,#53008,#53009,#53010,#53011,
#53012,#53013,#53014,#53015,#53016,#53017,#53018,#53019,#53020,#53021,#53022,
#53023,#53024,#53025,#53026,#53027,#53028,#53029,#53030,#53031,#53032,#53033,
#53034,#53035,#53036,#53037,#53038,#53039,#53040,#53041,#53042,#53043,#53044,
#53045,#53046,#53047,#53048,#53049,#53050,#53051,#53052,#53053,#53054,#53055,
#53056,#53057,#53058,#53059,#53060,#53061,#53062,#53063,#53064,#53065,#53066,
#53067,#53068,#53069,#53070,#53071,#53072,#53073,#53074,#53075,#53076,#53077,
#53078,#53079,#53080,#53081,#53082,#53083,#53084,#53085,#53086,#53087,#53088,
#53089,#53090,#53091,#53092,#53093,#53094,#53095,#53096,#53097,#53098,#53099,
#53100,#53101,#53102,#53103,#53104,#53105,#53106,#53107,#53108,#53109,#53110,
#53111,#53112,#53113,#53114,#53115,#53116,#53117,#53118,#53119,#53120,#53121,
#53122,#53123,#53124,#53125,#53126,#53127,#53128,#53129,#53130,#53131,#53132,
#53133,#53134,#53135,#53136,#53137,#53138,#53139,#53140,#53141,#53142,#53143,
#53144,#53145,#53146,#53147,#53148,#53149,#53150,#53151,#53152,#53153,#53154,
#53155,#53156,#53157,#53158,#53159,#53160,#53161,#53162,#53163,#53164,#53165,
#53166,#53167,#53168,#53169,#53170,#53171,#53172,#53173,#53174,#53175,#53176,
#53177,#53178,#53179,#53180,#53181,#53182,#53183,#53184,#53185,#53186,#53187,
#53188,#53189,#53190,#53191,#53192,#53193,#53194,#53195,#53196,#53197,#53198,
#53199,#53200,#53201,#53202,#53203,#53204,#53205,#53206,#53207,#53208,#53209,
#53210,#53211,#53212,#53213,#53214,#53215,#53216,#53217,#53218,#53219,#53220,
#53221,#53222,#53223,#53224,#53225,#53226,#53227,#53228,#53229,#53230,#53231,
#53232,#53233,#53234,#53235,#53236,#53237,#53238,#53239,#53240,#53241,#53242,
#53243,#53244,#53245,#53246,#53247,#53248,#53249,#53250,#53251,#53252,#53253,
#53254,#53255,#53256,#53257,#53258,#53259,#53260,#53261,#53262,#53263,#53264,
#53265,#53266,#53267,#53268,#53269,#53270,#53271,#53272,#53273,#53274,#53275,
#53276,#53277,#53278,#53279,#53280,#53281,#53282,#53283,#53284,#53285,#53286,
#53287,#53288,#53289,#53290,#53291,#53292,#53293,#53294,#53295,#53296,#53297,
#53298,#53299,#53300,#53301,#53302,#53303,#53304,#53305,#53306,#53307,#53308,
#53309,#53310,#53311,#53312,#53313,#53314,#53315,#53316,#53317,#53318,#53319,
#53320,#53321,#53322,#53323,#53324,#53325,#53326,#53327,#53328,#53329,#53330,
#53331,#53332,#53333,#53334,#53335,#53336,#53337,#53338,#53339,#53340,#53341,
#53342,#53343,#53344,#53345,#53346,#53347,#53348,#53349,#53350,#53351,#53352,
#53353,#53354,#53355,#53356,#53357,#53358,#53359,#53360,#53361,#53362,#53363,
#53364,#53365,#53366,#53367,#53368,#53369,#53370,#53371,#53372,#53373,#53374,
#53375,#53376,#53377,#53378,#53379,#53380,#53381,#53382,#53383,#53384,#53385,
#53386,#53387,#53388,#53389,#53390,#53391,#53392,#53393,#53394,#53395,#53396,
#53397,#53398,#53399,#53400,#53401,#53402,#53403,#53404,#53405,#53406,#53407,
#53408,#53409,#53410,#53411,#53412,#53413,#53414,#53415,#53416,#53417,#53418,
#53419,#53420,#53421,#53422,#53423,#53424,#53425,#53426,#53427,#53428,#53429,
#53430,#53431,#53432,#53433,#53434,#53435,#53436,#53437,#53438,#53439,#53440,
#53441,#53442,#53443,#53444,#53445,#53446,#53447,#53448,#53449,#53450,#53451,
#53452,#53453,#53454,#53455,#53456,#53457,#53458,#53459,#53460,#53461,#53462,
#53463,#53464,#53465,#53466,#53467,#53468,#53469,#53470,#53471,#53472,#53473,
#53474,#53475),(#53476,#53477,#53478,#53479,#53480,#53481,#53482,#53483,
#53484,#53485,#53486,#53487,#53488,#53489,#53490,#53491,#53492,#53493,#53494,
#53495,#53496,#53497,#53498,#53499,#53500,#53501,#53502,#53503,#53504,#53505,
#53506,#53507,#53508,#53509,#53510,#53511,#53512,#53513,#53514,#53515,#53516,
#53517,#53518,#53519,#53520,#53521,#53522,#53523,#53524,#53525,#53526,#53527,
#53528,#53529,#53530,#53531,#53532,#53533,#53534,#53535,#53536,#53537,#53538,
#53539,#53540,#53541,#53542,#53543,#53544,#53545,#53546,#53547,#53548,#53549,
#53550,#53551,#53552,#53553,#53554,#53555,#53556,#53557,#53558,#53559,#53560,
#53561,#53562,#53563,#53564,#53565,#53566,#53567,#53568,#53569,#53570,#53571,
#53572,#53573,#53574,#53575,#53576,#53577,#53578,#53579,#53580,#53581,#53582,
#53583,#53584,#53585,#53586,#53587,#53588,#53589,#53590,#53591,#53592,#53593,
#53594,#53595,#53596,#53597,#53598,#53599,#53600,#53601,#53602,#53603,#53604,
#53605,#53606,#53607,#53608,#53609,#53610,#53611,#53612,#53613,#53614,#53615,
#53616,#53617,#53618,#53619,#53620,#53621,#53622,#53623,#53624,#53625,#53626,
#53627,#53628,#53629,#53630,#53631,#53632,#53633,#53634,#53635,#53636,#53637,
#53638,#53639,#53640,#53641,#53642,#53643,#53644,#53645,#53646,#53647,#53648,
#53649,#53650,#53651,#53652,#53653,#53654,#53655,#53656,#53657,#53658,#53659,
#53660,#53661,#53662,#53663,#53664,#53665,#53666,#53667,#53668,#53669,#53670,
#53671,#53672,#53673,#53674,#53675,#53676,#53677,#53678,#53679,#53680,#53681,
#53682,#53683,#53684,#53685,#53686,#53687,#53688,#53689,#53690,#53691,#53692,
#53693,#53694,#53695,#53696,#53697,#53698,#53699,#53700,#53701,#53702,#53703,
#53704,#53705,#53706,#53707,#53708,#53709,#53710,#53711,#53712,#53713,#53714,
#53715,#53716,#53717,#53718,#53719,#53720,#53721,#53722,#53723,#53724,#53725,
#53726,#53727,#53728,#53729,#53730,#53731,#53732,#53733,#53734,#53735,#53736,
#53737,#53738,#53739,#53740,#53741,#53742,#53743,#53744,#53745,#53746,#53747,
#53748,#53749,#53750,#53751,#53752,#53753,#53754,#53755,#53756,#53757,#53758,
#53759,#53760,#53761,#53762,#53763,#53764,#53765,#53766,#53767,#53768,#53769,
#53770,#53771,#53772,#53773,#53774,#53775,#53776,#53777,#53778,#53779,#53780,
#53781,#53782,#53783,#53784,#53785,#53786,#53787,#53788,#53789,#53790,#53791,
#53792,#53793,#53794,#53795,#53796,#53797,#53798,#53799,#53800,#53801,#53802,
#53803,#53804,#53805,#53806,#53807,#53808,#53809,#53810,#53811,#53812,#53813,
#53814,#53815,#53816,#53817,#53818,#53819,#53820,#53821,#53822,#53823,#53824,
#53825,#53826,#53827,#53828,#53829,#53830,#53831,#53832,#53833,#53834,#53835,
#53836,#53837,#53838,#53839,#53840,#53841,#53842,#53843,#53844,#53845,#53846,
#53847,#53848,#53849,#53850,#53851,#53852,#53853,#53854,#53855,#53856,#53857,
#53858,#53859,#53860,#53861,#53862,#53863,#53864,#53865,#53866,#53867,#53868,
#53869,#53870,#53871,#53872,#53873,#53874,#53875,#53876,#53877,#53878,#53879,
#53880,#53881,#53882,#53883,#53884,#53885,#53886,#53887,#53888,#53889,#53890,
#53891,#53892,#53893,#53894,#53895,#53896,#53897,#53898,#53899,#53900,#53901,
#53902,#53903,#53904,#53905,#53906,#53907,#53908,#53909,#53910,#53911,#53912,
#53913,#53914,#53915,#53916,#53917,#53918,#53919,#53920,#53921,#53922,#53923,
#53924,#53925,#53926,#53927,#53928,#53929,#53930,#53931,#53932,#53933,#53934,
#53935,#53936,#53937,#53938,#53939,#53940,#53941,#53942,#53943,#53944,#53945,
#53946,#53947,#53948,#53949,#53950,#53951,#53952,#53953,#53954,#53955,#53956,
#53957,#53958,#53959,#53960,#53961,#53962,#53963,#53964,#53965,#53966,#53967,
#53968,#53969,#53970,#53971,#53972,#53973,#53974,#53975,#53976,#53977),
(#53978,#53979,#53980,#53981,#53982,#53983,#53984,#53985,#53986,#53987,
#53988,#53989,#53990,#53991,#53992,#53993,#53994,#53995,#53996,#53997,#53998,
#53999,#54000,#54001,#54002,#54003,#54004,#54005,#54006,#54007,#54008,#54009,
#54010,#54011,#54012,#54013,#54014,#54015,#54016,#54017,#54018,#54019,#54020,
#54021,#54022,#54023,#54024,#54025,#54026,#54027,#54028,#54029,#54030,#54031,
#54032,#54033,#54034,#54035,#54036,#54037,#54038,#54039,#54040,#54041,#54042,
#54043,#54044,#54045,#54046,#54047,#54048,#54049,#54050,#54051,#54052,#54053,
#54054,#54055,#54056,#54057,#54058,#54059,#54060,#54061,#54062,#54063,#54064,
#54065,#54066,#54067,#54068,#54069,#54070,#54071,#54072,#54073,#54074,#54075,
#54076,#54077,#54078,#54079,#54080,#54081,#54082,#54083,#54084,#54085,#54086,
#54087,#54088,#54089,#54090,#54091,#54092,#54093,#54094,#54095,#54096,#54097,
#54098,#54099,#54100,#54101,#54102,#54103,#54104,#54105,#54106,#54107,#54108,
#54109,#54110,#54111,#54112,#54113,#54114,#54115,#54116,#54117,#54118,#54119,
#54120,#54121,#54122,#54123,#54124,#54125,#54126,#54127,#54128,#54129,#54130,
#54131,#54132,#54133,#54134,#54135,#54136,#54137,#54138,#54139,#54140,#54141,
#54142,#54143,#54144,#54145,#54146,#54147,#54148,#54149,#54150,#54151,#54152,
#54153,#54154,#54155,#54156,#54157,#54158,#54159,#54160,#54161,#54162,#54163,
#54164,#54165,#54166,#54167,#54168,#54169,#54170,#54171,#54172,#54173,#54174,
#54175,#54176,#54177,#54178,#54179,#54180,#54181,#54182,#54183,#54184,#54185,
#54186,#54187,#54188,#54189,#54190,#54191,#54192,#54193,#54194,#54195,#54196,
#54197,#54198,#54199,#54200,#54201,#54202,#54203,#54204,#54205,#54206,#54207,
#54208,#54209,#54210,#54211,#54212,#54213,#54214,#54215,#54216,#54217,#54218,
#54219,#54220,#54221,#54222,#54223,#54224,#54225,#54226,#54227,#54228,#54229,
#54230,#54231,#54232,#54233,#54234,#54235,#54236,#54237,#54238,#54239,#54240,
#54241,#54242,#54243,#54244,#54245,#54246,#54247,#54248,#54249,#54250,#54251,
#54252,#54253,#54254,#54255,#54256,#54257,#54258,#54259,#54260,#54261,#54262,
#54263,#54264,#54265,#54266,#54267,#54268,#54269,#54270,#54271,#54272,#54273,
#54274,#54275,#54276,#54277,#54278,#54279,#54280,#54281,#54282,#54283,#54284,
#54285,#54286,#54287,#54288,#54289,#54290,#54291,#54292,#54293,#54294,#54295,
#54296,#54297,#54298,#54299,#54300,#54301,#54302,#54303,#54304,#54305,#54306,
#54307,#54308,#54309,#54310,#54311,#54312,#54313,#54314,#54315,#54316,#54317,
#54318,#54319,#54320,#54321,#54322,#54323,#54324,#54325,#54326,#54327,#54328,
#54329,#54330,#54331,#54332,#54333,#54334,#54335,#54336,#54337,#54338,#54339,
#54340,#54341,#54342,#54343,#54344,#54345,#54346,#54347,#54348,#54349,#54350,
#54351,#54352,#54353,#54354,#54355,#54356,#54357,#54358,#54359,#54360,#54361,
#54362,#54363,#54364,#54365,#54366,#54367,#54368,#54369,#54370,#54371,#54372,
#54373,#54374,#54375,#54376,#54377,#54378,#54379,#54380,#54381,#54382,#54383,
#54384,#54385,#54386,#54387,#54388,#54389,#54390,#54391,#54392,#54393,#54394,
#54395,#54396,#54397,#54398,#54399,#54400,#54401,#54402,#54403,#54404,#54405,
#54406,#54407,#54408,#54409,#54410,#54411,#54412,#54413,#54414,#54415,#54416,
#54417,#54418,#54419,#54420,#54421,#54422,#54423,#54424,#54425,#54426,#54427,
#54428,#54429,#54430,#54431,#54432,#54433,#54434,#54435,#54436,#54437,#54438,
#54439,#54440,#54441,#54442,#54443,#54444,#54445,#54446,#54447,#54448,#54449,
#54450,#54451,#54452,#54453,#54454,#54455,#54456,#54457,#54458,#54459,#54460,
#54461,#54462,#54463,#54464,#54465,#54466,#54467,#54468,#54469,#54470,#54471,
#54472,#54473,#54474,#54475,#54476,#54477,#54478,#54479),(#54480,#54481,
#54482,#54483,#54484,#54485,#54486,#54487,#54488,#54489,#54490,#54491,#54492,
#54493,#54494,#54495,#54496,#54497,#54498,#54499,#54500,#54501,#54502,#54503,
#54504,#54505,#54506,#54507,#54508,#54509,#54510,#54511,#54512,#54513,#54514,
#54515,#54516,#54517,#54518,#54519,#54520,#54521,#54522,#54523,#54524,#54525,
#54526,#54527,#54528,#54529,#54530,#54531,#54532,#54533,#54534,#54535,#54536,
#54537,#54538,#54539,#54540,#54541,#54542,#54543,#54544,#54545,#54546,#54547,
#54548,#54549,#54550,#54551,#54552,#54553,#54554,#54555,#54556,#54557,#54558,
#54559,#54560,#54561,#54562,#54563,#54564,#54565,#54566,#54567,#54568,#54569,
#54570,#54571,#54572,#54573,#54574,#54575,#54576,#54577,#54578,#54579,#54580,
#54581,#54582,#54583,#54584,#54585,#54586,#54587,#54588,#54589,#54590,#54591,
#54592,#54593,#54594,#54595,#54596,#54597,#54598,#54599,#54600,#54601,#54602,
#54603,#54604,#54605,#54606,#54607,#54608,#54609,#54610,#54611,#54612,#54613,
#54614,#54615,#54616,#54617,#54618,#54619,#54620,#54621,#54622,#54623,#54624,
#54625,#54626,#54627,#54628,#54629,#54630,#54631,#54632,#54633,#54634,#54635,
#54636,#54637,#54638,#54639,#54640,#54641,#54642,#54643,#54644,#54645,#54646,
#54647,#54648,#54649,#54650,#54651,#54652,#54653,#54654,#54655,#54656,#54657,
#54658,#54659,#54660,#54661,#54662,#54663,#54664,#54665,#54666,#54667,#54668,
#54669,#54670,#54671,#54672,#54673,#54674,#54675,#54676,#54677,#54678,#54679,
#54680,#54681,#54682,#54683,#54684,#54685,#54686,#54687,#54688,#54689,#54690,
#54691,#54692,#54693,#54694,#54695,#54696,#54697,#54698,#54699,#54700,#54701,
#54702,#54703,#54704,#54705,#54706,#54707,#54708,#54709,#54710,#54711,#54712,
#54713,#54714,#54715,#54716,#54717,#54718,#54719,#54720,#54721,#54722,#54723,
#54724,#54725,#54726,#54727,#54728,#54729,#54730,#54731,#54732,#54733,#54734,
#54735,#54736,#54737,#54738,#54739,#54740,#54741,#54742,#54743,#54744,#54745,
#54746,#54747,#54748,#54749,#54750,#54751,#54752,#54753,#54754,#54755,#54756,
#54757,#54758,#54759,#54760,#54761,#54762,#54763,#54764,#54765,#54766,#54767,
#54768,#54769,#54770,#54771,#54772,#54773,#54774,#54775,#54776,#54777,#54778,
#54779,#54780,#54781,#54782,#54783,#54784,#54785,#54786,#54787,#54788,#54789,
#54790,#54791,#54792,#54793,#54794,#54795,#54796,#54797,#54798,#54799,#54800,
#54801,#54802,#54803,#54804,#54805,#54806,#54807,#54808,#54809,#54810,#54811,
#54812,#54813,#54814,#54815,#54816,#54817,#54818,#54819,#54820,#54821,#54822,
#54823,#54824,#54825,#54826,#54827,#54828,#54829,#54830,#54831,#54832,#54833,
#54834,#54835,#54836,#54837,#54838,#54839,#54840,#54841,#54842,#54843,#54844,
#54845,#54846,#54847,#54848,#54849,#54850,#54851,#54852,#54853,#54854,#54855,
#54856,#54857,#54858,#54859,#54860,#54861,#54862,#54863,#54864,#54865,#54866,
#54867,#54868,#54869,#54870,#54871,#54872,#54873,#54874,#54875,#54876,#54877,
#54878,#54879,#54880,#54881,#54882,#54883,#54884,#54885,#54886,#54887,#54888,
#54889,#54890,#54891,#54892,#54893,#54894,#54895,#54896,#54897,#54898,#54899,
#54900,#54901,#54902,#54903,#54904,#54905,#54906,#54907,#54908,#54909,#54910,
#54911,#54912,#54913,#54914,#54915,#54916,#54917,#54918,#54919,#54920,#54921,
#54922,#54923,#54924,#54925,#54926,#54927,#54928,#54929,#54930,#54931,#54932,
#54933,#54934,#54935,#54936,#54937,#54938,#54939,#54940,#54941,#54942,#54943,
#54944,#54945,#54946,#54947,#54948,#54949,#54950,#54951,#54952,#54953,#54954,
#54955,#54956,#54957,#54958,#54959,#54960,#54961,#54962,#54963,#54964,#54965,
#54966,#54967,#54968,#54969,#54970,#54971,#54972,#54973,#54974,#54975,#54976,
#54977,#54978,#54979,#54980,#54981),(#54982,#54983,#54984,#54985,#54986,
#54987,#54988,#54989,#54990,#54991,#54992,#54993,#54994,#54995,#54996,#54997,
#54998,#54999,#55000,#55001,#55002,#55003,#55004,#55005,#55006,#55007,#55008,
#55009,#55010,#55011,#55012,#55013,#55014,#55015,#55016,#55017,#55018,#55019,
#55020,#55021,#55022,#55023,#55024,#55025,#55026,#55027,#55028,#55029,#55030,
#55031,#55032,#55033,#55034,#55035,#55036,#55037,#55038,#55039,#55040,#55041,
#55042,#55043,#55044,#55045,#55046,#55047,#55048,#55049,#55050,#55051,#55052,
#55053,#55054,#55055,#55056,#55057,#55058,#55059,#55060,#55061,#55062,#55063,
#55064,#55065,#55066,#55067,#55068,#55069,#55070,#55071,#55072,#55073,#55074,
#55075,#55076,#55077,#55078,#55079,#55080,#55081,#55082,#55083,#55084,#55085,
#55086,#55087,#55088,#55089,#55090,#55091,#55092,#55093,#55094,#55095,#55096,
#55097,#55098,#55099,#55100,#55101,#55102,#55103,#55104,#55105,#55106,#55107,
#55108,#55109,#55110,#55111,#55112,#55113,#55114,#55115,#55116,#55117,#55118,
#55119,#55120,#55121,#55122,#55123,#55124,#55125,#55126,#55127,#55128,#55129,
#55130,#55131,#55132,#55133,#55134,#55135,#55136,#55137,#55138,#55139,#55140,
#55141,#55142,#55143,#55144,#55145,#55146,#55147,#55148,#55149,#55150,#55151,
#55152,#55153,#55154,#55155,#55156,#55157,#55158,#55159,#55160,#55161,#55162,
#55163,#55164,#55165,#55166,#55167,#55168,#55169,#55170,#55171,#55172,#55173,
#55174,#55175,#55176,#55177,#55178,#55179,#55180,#55181,#55182,#55183,#55184,
#55185,#55186,#55187,#55188,#55189,#55190,#55191,#55192,#55193,#55194,#55195,
#55196,#55197,#55198,#55199,#55200,#55201,#55202,#55203,#55204,#55205,#55206,
#55207,#55208,#55209,#55210,#55211,#55212,#55213,#55214,#55215,#55216,#55217,
#55218,#55219,#55220,#55221,#55222,#55223,#55224,#55225,#55226,#55227,#55228,
#55229,#55230,#55231,#55232,#55233,#55234,#55235,#55236,#55237,#55238,#55239,
#55240,#55241,#55242,#55243,#55244,#55245,#55246,#55247,#55248,#55249,#55250,
#55251,#55252,#55253,#55254,#55255,#55256,#55257,#55258,#55259,#55260,#55261,
#55262,#55263,#55264,#55265,#55266,#55267,#55268,#55269,#55270,#55271,#55272,
#55273,#55274,#55275,#55276,#55277,#55278,#55279,#55280,#55281,#55282,#55283,
#55284,#55285,#55286,#55287,#55288,#55289,#55290,#55291,#55292,#55293,#55294,
#55295,#55296,#55297,#55298,#55299,#55300,#55301,#55302,#55303,#55304,#55305,
#55306,#55307,#55308,#55309,#55310,#55311,#55312,#55313,#55314,#55315,#55316,
#55317,#55318,#55319,#55320,#55321,#55322,#55323,#55324,#55325,#55326,#55327,
#55328,#55329,#55330,#55331,#55332,#55333,#55334,#55335,#55336,#55337,#55338,
#55339,#55340,#55341,#55342,#55343,#55344,#55345,#55346,#55347,#55348,#55349,
#55350,#55351,#55352,#55353,#55354,#55355,#55356,#55357,#55358,#55359,#55360,
#55361,#55362,#55363,#55364,#55365,#55366,#55367,#55368,#55369,#55370,#55371,
#55372,#55373,#55374,#55375,#55376,#55377,#55378,#55379,#55380,#55381,#55382,
#55383,#55384,#55385,#55386,#55387,#55388,#55389,#55390,#55391,#55392,#55393,
#55394,#55395,#55396,#55397,#55398,#55399,#55400,#55401,#55402,#55403,#55404,
#55405,#55406,#55407,#55408,#55409,#55410,#55411,#55412,#55413,#55414,#55415,
#55416,#55417,#55418,#55419,#55420,#55421,#55422,#55423,#55424,#55425,#55426,
#55427,#55428,#55429,#55430,#55431,#55432,#55433,#55434,#55435,#55436,#55437,
#55438,#55439,#55440,#55441,#55442,#55443,#55444,#55445,#55446,#55447,#55448,
#55449,#55450,#55451,#55452,#55453,#55454,#55455,#55456,#55457,#55458,#55459,
#55460,#55461,#55462,#55463,#55464,#55465,#55466,#55467,#55468,#55469,#55470,
#55471,#55472,#55473,#55474,#55475,#55476,#55477,#55478,#55479,#55480,#55481,
#55482,#55483),(#55484,#55485,#55486,#55487,#55488,#55489,#55490,#55491,
#55492,#55493,#55494,#55495,#55496,#55497,#55498,#55499,#55500,#55501,#55502,
#55503,#55504,#55505,#55506,#55507,#55508,#55509,#55510,#55511,#55512,#55513,
#55514,#55515,#55516,#55517,#55518,#55519,#55520,#55521,#55522,#55523,#55524,
#55525,#55526,#55527,#55528,#55529,#55530,#55531,#55532,#55533,#55534,#55535,
#55536,#55537,#55538,#55539,#55540,#55541,#55542,#55543,#55544,#55545,#55546,
#55547,#55548,#55549,#55550,#55551,#55552,#55553,#55554,#55555,#55556,#55557,
#55558,#55559,#55560,#55561,#55562,#55563,#55564,#55565,#55566,#55567,#55568,
#55569,#55570,#55571,#55572,#55573,#55574,#55575,#55576,#55577,#55578,#55579,
#55580,#55581,#55582,#55583,#55584,#55585,#55586,#55587,#55588,#55589,#55590,
#55591,#55592,#55593,#55594,#55595,#55596,#55597,#55598,#55599,#55600,#55601,
#55602,#55603,#55604,#55605,#55606,#55607,#55608,#55609,#55610,#55611,#55612,
#55613,#55614,#55615,#55616,#55617,#55618,#55619,#55620,#55621,#55622,#55623,
#55624,#55625,#55626,#55627,#55628,#55629,#55630,#55631,#55632,#55633,#55634,
#55635,#55636,#55637,#55638,#55639,#55640,#55641,#55642,#55643,#55644,#55645,
#55646,#55647,#55648,#55649,#55650,#55651,#55652,#55653,#55654,#55655,#55656,
#55657,#55658,#55659,#55660,#55661,#55662,#55663,#55664,#55665,#55666,#55667,
#55668,#55669,#55670,#55671,#55672,#55673,#55674,#55675,#55676,#55677,#55678,
#55679,#55680,#55681,#55682,#55683,#55684,#55685,#55686,#55687,#55688,#55689,
#55690,#55691,#55692,#55693,#55694,#55695,#55696,#55697,#55698,#55699,#55700,
#55701,#55702,#55703,#55704,#55705,#55706,#55707,#55708,#55709,#55710,#55711,
#55712,#55713,#55714,#55715,#55716,#55717,#55718,#55719,#55720,#55721,#55722,
#55723,#55724,#55725,#55726,#55727,#55728,#55729,#55730,#55731,#55732,#55733,
#55734,#55735,#55736,#55737,#55738,#55739,#55740,#55741,#55742,#55743,#55744,
#55745,#55746,#55747,#55748,#55749,#55750,#55751,#55752,#55753,#55754,#55755,
#55756,#55757,#55758,#55759,#55760,#55761,#55762,#55763,#55764,#55765,#55766,
#55767,#55768,#55769,#55770,#55771,#55772,#55773,#55774,#55775,#55776,#55777,
#55778,#55779,#55780,#55781,#55782,#55783,#55784,#55785,#55786,#55787,#55788,
#55789,#55790,#55791,#55792,#55793,#55794,#55795,#55796,#55797,#55798,#55799,
#55800,#55801,#55802,#55803,#55804,#55805,#55806,#55807,#55808,#55809,#55810,
#55811,#55812,#55813,#55814,#55815,#55816,#55817,#55818,#55819,#55820,#55821,
#55822,#55823,#55824,#55825,#55826,#55827,#55828,#55829,#55830,#55831,#55832,
#55833,#55834,#55835,#55836,#55837,#55838,#55839,#55840,#55841,#55842,#55843,
#55844,#55845,#55846,#55847,#55848,#55849,#55850,#55851,#55852,#55853,#55854,
#55855,#55856,#55857,#55858,#55859,#55860,#55861,#55862,#55863,#55864,#55865,
#55866,#55867,#55868,#55869,#55870,#55871,#55872,#55873,#55874,#55875,#55876,
#55877,#55878,#55879,#55880,#55881,#55882,#55883,#55884,#55885,#55886,#55887,
#55888,#55889,#55890,#55891,#55892,#55893,#55894,#55895,#55896,#55897,#55898,
#55899,#55900,#55901,#55902,#55903,#55904,#55905,#55906,#55907,#55908,#55909,
#55910,#55911,#55912,#55913,#55914,#55915,#55916,#55917,#55918,#55919,#55920,
#55921,#55922,#55923,#55924,#55925,#55926,#55927,#55928,#55929,#55930,#55931,
#55932,#55933,#55934,#55935,#55936,#55937,#55938,#55939,#55940,#55941,#55942,
#55943,#55944,#55945,#55946,#55947,#55948,#55949,#55950,#55951,#55952,#55953,
#55954,#55955,#55956,#55957,#55958,#55959,#55960,#55961,#55962,#55963,#55964,
#55965,#55966,#55967,#55968,#55969,#55970,#55971,#55972,#55973,#55974,#55975,
#55976,#55977,#55978,#55979,#55980,#55981,#55982,#55983,#55984,#55985),
(#55986,#55987,#55988,#55989,#55990,#55991,#55992,#55993,#55994,#55995,
#55996,#55997,#55998,#55999,#56000,#56001,#56002,#56003,#56004,#56005,#56006,
#56007,#56008,#56009,#56010,#56011,#56012,#56013,#56014,#56015,#56016,#56017,
#56018,#56019,#56020,#56021,#56022,#56023,#56024,#56025,#56026,#56027,#56028,
#56029,#56030,#56031,#56032,#56033,#56034,#56035,#56036,#56037,#56038,#56039,
#56040,#56041,#56042,#56043,#56044,#56045,#56046,#56047,#56048,#56049,#56050,
#56051,#56052,#56053,#56054,#56055,#56056,#56057,#56058,#56059,#56060,#56061,
#56062,#56063,#56064,#56065,#56066,#56067,#56068,#56069,#56070,#56071,#56072,
#56073,#56074,#56075,#56076,#56077,#56078,#56079,#56080,#56081,#56082,#56083,
#56084,#56085,#56086,#56087,#56088,#56089,#56090,#56091,#56092,#56093,#56094,
#56095,#56096,#56097,#56098,#56099,#56100,#56101,#56102,#56103,#56104,#56105,
#56106,#56107,#56108,#56109,#56110,#56111,#56112,#56113,#56114,#56115,#56116,
#56117,#56118,#56119,#56120,#56121,#56122,#56123,#56124,#56125,#56126,#56127,
#56128,#56129,#56130,#56131,#56132,#56133,#56134,#56135,#56136,#56137,#56138,
#56139,#56140,#56141,#56142,#56143,#56144,#56145,#56146,#56147,#56148,#56149,
#56150,#56151,#56152,#56153,#56154,#56155,#56156,#56157,#56158,#56159,#56160,
#56161,#56162,#56163,#56164,#56165,#56166,#56167,#56168,#56169,#56170,#56171,
#56172,#56173,#56174,#56175,#56176,#56177,#56178,#56179,#56180,#56181,#56182,
#56183,#56184,#56185,#56186,#56187,#56188,#56189,#56190,#56191,#56192,#56193,
#56194,#56195,#56196,#56197,#56198,#56199,#56200,#56201,#56202,#56203,#56204,
#56205,#56206,#56207,#56208,#56209,#56210,#56211,#56212,#56213,#56214,#56215,
#56216,#56217,#56218,#56219,#56220,#56221,#56222,#56223,#56224,#56225,#56226,
#56227,#56228,#56229,#56230,#56231,#56232,#56233,#56234,#56235,#56236,#56237,
#56238,#56239,#56240,#56241,#56242,#56243,#56244,#56245,#56246,#56247,#56248,
#56249,#56250,#56251,#56252,#56253,#56254,#56255,#56256,#56257,#56258,#56259,
#56260,#56261,#56262,#56263,#56264,#56265,#56266,#56267,#56268,#56269,#56270,
#56271,#56272,#56273,#56274,#56275,#56276,#56277,#56278,#56279,#56280,#56281,
#56282,#56283,#56284,#56285,#56286,#56287,#56288,#56289,#56290,#56291,#56292,
#56293,#56294,#56295,#56296,#56297,#56298,#56299,#56300,#56301,#56302,#56303,
#56304,#56305,#56306,#56307,#56308,#56309,#56310,#56311,#56312,#56313,#56314,
#56315,#56316,#56317,#56318,#56319,#56320,#56321,#56322,#56323,#56324,#56325,
#56326,#56327,#56328,#56329,#56330,#56331,#56332,#56333,#56334,#56335,#56336,
#56337,#56338,#56339,#56340,#56341,#56342,#56343,#56344,#56345,#56346,#56347,
#56348,#56349,#56350,#56351,#56352,#56353,#56354,#56355,#56356,#56357,#56358,
#56359,#56360,#56361,#56362,#56363,#56364,#56365,#56366,#56367,#56368,#56369,
#56370,#56371,#56372,#56373,#56374,#56375,#56376,#56377,#56378,#56379,#56380,
#56381,#56382,#56383,#56384,#56385,#56386,#56387,#56388,#56389,#56390,#56391,
#56392,#56393,#56394,#56395,#56396,#56397,#56398,#56399,#56400,#56401,#56402,
#56403,#56404,#56405,#56406,#56407,#56408,#56409,#56410,#56411,#56412,#56413,
#56414,#56415,#56416,#56417,#56418,#56419,#56420,#56421,#56422,#56423,#56424,
#56425,#56426,#56427,#56428,#56429,#56430,#56431,#56432,#56433,#56434,#56435,
#56436,#56437,#56438,#56439,#56440,#56441,#56442,#56443,#56444,#56445,#56446,
#56447,#56448,#56449,#56450,#56451,#56452,#56453,#56454,#56455,#56456,#56457,
#56458,#56459,#56460,#56461,#56462,#56463,#56464,#56465,#56466,#56467,#56468,
#56469,#56470,#56471,#56472,#56473,#56474,#56475,#56476,#56477,#56478,#56479,
#56480,#56481,#56482,#56483,#56484,#56485,#56486,#56487)),.UNSPECIFIED.,
 .T.,.F.,.F.,(4,1,1,1,1,1,1,1,4),(4,1,1,1,1,1,1,1,1,1,1,1,1,1,1,1,1,1,1,
1,1,1,1,1,1,1,1,1,1,1,1,1,1,1,1,1,1,1,1,1,1,1,1,1,1,1,1,1,1,1,1,1,1,1,1,
1,1,1,1,1,1,1,1,1,1,1,1,1,1,1,1,1,1,1,1,1,1,1,1,1,1,1,1,1,1,1,1,1,1,1,1,
1,1,1,1,1,1,1,1,1,1,1,1,1,1,1,1,1,1,1,1,1,1,1,1,1,1,1,1,1,1,1,1,1,1,1,1,
1,1,1,1,1,1,1,1,1,1,1,1,1,1,1,1,1,1,1,1,1,1,1,1,1,1,1,1,1,1,1,1,1,1,1,1,
1,1,1,1,1,1,1,1,1,1,1,1,1,1,1,1,1,1,1,1,1,1,1,1,1,1,1,1,1,1,1,1,1,1,1,1,
1,1,1,1,1,1,1,1,1,1,1,1,1,1,1,1,1,1,1,1,1,1,1,1,1,1,1,1,1,1,1,1,1,1,1,1,
1,1,1,1,1,1,1,1,1,1,1,1,1,1,1,1,1,1,1,1,1,1,1,1,1,1,1,1,1,1,1,1,1,1,1,1,
1,1,1,1,1,1,1,1,1,1,1,1,1,1,1,1,1,1,1,1,1,1,1,1,1,1,1,1,1,1,1,1,1,1,1,1,
1,1,1,1,1,1,1,1,1,1,1,1,1,1,1,1,1,1,1,1,1,1,1,1,1,1,1,1,1,1,1,1,1,1,1,1,
1,1,1,1,1,1,1,1,1,1,1,1,1,1,1,1,1,1,1,1,1,1,1,1,1,1,1,1,1,1,1,1,1,1,1,1,
1,1,1,1,1,1,1,1,1,1,1,1,1,1,1,1,1,1,1,1,1,1,1,1,1,1,1,1,1,1,1,1,1,1,1,1,
1,1,1,1,1,1,1,1,1,1,1,1,1,1,1,1,1,1,1,1,1,1,1,1,1,1,1,1,1,1,1,1,1,1,1,1,
1,1,1,1,1,1,1,1,1,1,1,1,1,1,1,1,1,1,1,1,1,1,1,1,1,1,1,1,1,1,1,1,1,1,1,1,
1,1,1,1,1,1,1,1,1,1,1,1,4),(-3.14159265358979,-2.24399475256414,-1.34639685153848,
-0.448798950512828,0.448798950512828,1.34639685153848,1.5707963267949,2.24399475256414,
3.14159265358979),(0.,0.00167410714285714,0.00223214285714286,0.00334821428571429,
0.00446428571428571,0.00558035714285714,0.00669642857142857,0.00892857142857143,
0.0111607142857143,0.0133928571428571,0.015625,0.0178571428571429,0.0200892857142857,
0.0223214285714286,0.0245535714285714,0.0267857142857143,0.0290178571428571,
0.03125,0.0334821428571429,0.0357142857142857,0.0379464285714286,0.0401785714285714,
0.0424107142857143,0.0446428571428571,0.046875,0.0491071428571428,0.0513392857142857,
0.0535714285714286,0.0558035714285714,0.0580357142857143,0.0602678571428571,
0.0625,0.0647321428571428,0.0669642857142857,0.0680803571428572,0.0691964285714286,
0.0714285714285714,0.0736607142857143,0.0758928571428571,0.078125,0.0803571428571428,
0.0825892857142857,0.0848214285714286,0.0870535714285714,0.0892857142857143,
0.0915178571428571,0.09375,0.0959821428571428,0.0982142857142857,0.100446428571429,
0.102678571428571,0.104910714285714,0.107142857142857,0.109375,0.111607142857143,
0.113839285714286,0.116071428571429,0.118303571428571,0.119419642857143,
0.120535714285714,0.122767857142857,0.125,0.127232142857143,0.129464285714286,
0.131696428571429,0.133928571428571,0.136160714285714,0.138392857142857,
0.140625,0.142857142857143,0.144345238095238,0.145833333333333,0.146205357142857,
0.146577380952381,0.146949404761905,0.147321428571429,0.148809523809524,
0.150297619047619,0.151785714285714,0.15327380952381,0.154761904761905,
0.15625,0.157738095238095,0.160714285714286,0.162202380952381,0.162946428571429,
0.163690476190476,0.165178571428571,0.165550595238095,0.165922619047619,
0.166294642857143,0.166480654761905,0.166666666666667,0.169312169312169,
0.171957671957672,0.172839506172839,0.173721340388007,0.174162257495591,
0.174603174603175,0.177248677248677,0.17989417989418,0.182539682539683,
0.18452380952381,0.186507936507937,0.188492063492063,0.19047619047619,0.191468253968254,
0.192460317460317,0.193452380952381,0.193948412698413,0.194444444444444,
0.196428571428571,0.198412698412698,0.200396825396825,0.202380952380952,
0.202876984126984,0.203373015873016,0.204365079365079,0.206349206349206,
0.206597222222222,0.206845238095238,0.207093253968254,0.20734126984127,
0.207589285714286,0.207837301587302,0.208333333333333,0.21031746031746,
0.212301587301587,0.214285714285714,0.216269841269841,0.218253968253968,
0.220238095238095,0.222222222222222,0.222883597883598,0.223544973544974,
0.224867724867725,0.227513227513228,0.23015873015873,0.232804232804233,
0.235449735449735,0.238095238095238,0.239583333333333,0.241071428571429,
0.244047619047619,0.247023809523809,0.25,0.25297619047619,0.255952380952381,
0.258928571428571,0.260416666666667,0.261904761904762,0.263392857142857,
0.264880952380952,0.267857142857143,0.270833333333333,0.273809523809524,
0.276785714285714,0.279761904761905,0.282738095238095,0.285714285714286,
0.288690476190476,0.291666666666667,0.294642857142857,0.297619047619048,
0.300595238095238,0.303571428571429,0.306547619047619,0.30952380952381,
0.3125,0.31547619047619,0.318452380952381,0.321428571428571,0.324404761904762,
0.327380952380952,0.328869047619048,0.330357142857143,0.333333333333333,
0.336309523809524,0.339285714285714,0.342261904761905,0.345238095238095,
0.348214285714286,0.351190476190476,0.354166666666667,0.357142857142857,
0.360119047619048,0.363095238095238,0.366071428571428,0.367559523809524,
0.369047619047619,0.370535714285714,0.37202380952381,0.373511904761905,
0.375,0.376488095238095,0.37797619047619,0.378720238095238,0.379464285714286,
0.380952380952381,0.383928571428571,0.386904761904762,0.389880952380952,
0.391369047619048,0.392113095238095,0.392857142857143,0.394345238095238,
0.395833333333333,0.398809523809524,0.401785714285714,0.404761904761905,
0.407738095238095,0.40922619047619,0.410714285714286,0.411458333333333,
0.411830357142857,0.412202380952381,0.412946428571429,0.413690476190476,
0.415178571428571,0.416666666666667,0.418154761904762,0.419642857142857,
0.421130952380952,0.422619047619048,0.424107142857143,0.425595238095238,
0.427083333333333,0.427827380952381,0.428571428571429,0.430803571428571,
0.433035714285714,0.435267857142857,0.4375,0.439732142857143,0.441964285714286,
0.444196428571429,0.446428571428571,0.447544642857143,0.448660714285714,
0.450892857142857,0.453125,0.455357142857143,0.457589285714286,0.459821428571429,
0.462053571428571,0.464285714285714,0.466517857142857,0.46875,0.470982142857143,
0.472098214285714,0.473214285714286,0.475446428571429,0.477678571428571,
0.479910714285714,0.482142857142857,0.484375,0.486607142857143,0.488839285714286,
0.491071428571429,0.493303571428571,0.495535714285714,0.497767857142857,
0.5,0.502232142857143,0.504464285714286,0.506696428571429,0.508928571428571,
0.511160714285714,0.513392857142857,0.515625,0.517857142857143,0.520089285714286,
0.522321428571428,0.524553571428571,0.526785714285714,0.529017857142857,
0.53125,0.533482142857143,0.535714285714286,0.537946428571429,0.540178571428571,
0.542410714285714,0.544642857142857,0.545200892857143,0.545758928571429,
0.546875,0.549107142857143,0.551339285714286,0.553571428571429,0.555803571428571,
0.558035714285714,0.560267857142857,0.5625,0.564732142857143,0.566964285714286,
0.569196428571429,0.571428571428571,0.573660714285714,0.575892857142857,
0.578125,0.580357142857143,0.582589285714286,0.584821428571428,0.587053571428571,
0.589285714285714,0.591517857142857,0.59375,0.595982142857143,0.598214285714286,
0.600446428571428,0.602678571428571,0.604910714285714,0.607142857142857,
0.609375,0.611607142857143,0.613839285714286,0.616071428571429,0.618303571428571,
0.620535714285714,0.622767857142857,0.625,0.627232142857143,0.629464285714286,
0.631696428571429,0.633928571428571,0.636160714285714,0.638392857142857,
0.640625,0.642857142857143,0.644345238095238,0.645833333333333,0.648809523809524,
0.651785714285714,0.654761904761905,0.657738095238095,0.660714285714286,
0.663690476190476,0.665178571428571,0.666666666666667,0.667989417989418,
0.669312169312169,0.671957671957672,0.674603174603175,0.675925925925926,
0.677248677248677,0.67989417989418,0.682539682539682,0.684523809523809,
0.686507936507936,0.688492063492063,0.69047619047619,0.692460317460317,
0.694444444444444,0.696428571428571,0.697420634920635,0.698412698412698,
0.701058201058201,0.703703703703704,0.705026455026455,0.706349206349206,
0.707671957671958,0.71031746031746,0.712301587301587,0.714285714285714,
0.716517857142857,0.71875,0.720982142857143,0.72265625,0.723214285714286,
0.724702380952381,0.726190476190476,0.727678571428571,0.729166666666667,
0.730654761904762,0.732142857142857,0.733258928571428,0.734375,0.736607142857143,
0.738839285714286,0.741071428571428,0.743303571428571,0.745535714285714,
0.747767857142857,0.75,0.752232142857143,0.754464285714286,0.756696428571428,
0.758928571428571,0.761160714285714,0.763392857142857,0.765625,0.767857142857143,
0.770089285714286,0.772321428571428,0.774553571428571,0.776785714285714,
0.779017857142857,0.78125,0.783482142857143,0.785714285714286,0.787946428571428,
0.790178571428571,0.792410714285714,0.794642857142857,0.796875,0.799107142857143,
0.801339285714286,0.803571428571428,0.805803571428571,0.808035714285714,
0.810267857142857,0.8125,0.814732142857143,0.816964285714286,0.819196428571429,
0.821428571428571,0.823660714285714,0.825892857142857,0.828125,0.830357142857143,
0.832589285714286,0.834821428571428,0.837053571428571,0.839285714285714,
0.841517857142857,0.84375,0.845982142857143,0.848214285714286,0.850446428571428,
0.852678571428571,0.854910714285714,0.857142857142857,0.859375,0.861607142857143,
0.863839285714286,0.866071428571429,0.868303571428571,0.870535714285714,
0.872767857142857,0.875,0.877232142857143,0.879464285714286,0.881696428571429,
0.883928571428571,0.886160714285714,0.888392857142857,0.890625,0.892857142857143,
0.895089285714286,0.897321428571428,0.899553571428571,0.901785714285714,
0.904017857142857,0.90625,0.908482142857143,0.910714285714286,0.912946428571429,
0.915178571428571,0.917410714285714,0.919642857142857,0.921875,0.922991071428571,
0.924107142857143,0.926339285714286,0.928571428571429,0.930803571428571,
0.933035714285714,0.935267857142857,0.9375,0.939732142857143,0.941964285714286,
0.944196428571429,0.946428571428571,0.948660714285714,0.950892857142857,
0.953125,0.955357142857143,0.957589285714286,0.959821428571429,0.962053571428571,
0.964285714285714,0.966517857142857,0.96875,0.970982142857143,0.973214285714286,
0.975446428571429,0.977678571428572,0.979910714285714,0.982142857142857,
0.984375,0.986607142857143,0.988839285714286,0.991071428571429,0.993303571428571,
0.994419642857143,0.995535714285714,0.996651785714286,0.997767857142857,
0.998883928571429,1.),.UNSPECIFIED.);
#1462=B_SPLINE_SURFACE_WITH_KNOTS('',3,3,((#58051,#58052,#58053,#58054,
#58055,#58056,#58057,#58058,#58059,#58060,#58061,#58062,#58063,#58064,#58065,
#58066,#58067,#58068,#58069,#58070,#58071,#58072,#58073,#58074,#58075,#58076,
#58077,#58078,#58079,#58080,#58081,#58082,#58083,#58084,#58085,#58086,#58087,
#58088,#58089,#58090,#58091,#58092,#58093,#58094,#58095,#58096,#58097,#58098,
#58099,#58100,#58101,#58102,#58103,#58104,#58105,#58106,#58107,#58108,#58109,
#58110,#58111,#58112,#58113,#58114,#58115,#58116,#58117,#58118,#58119,#58120,
#58121,#58122,#58123,#58124,#58125,#58126),(#58127,#58128,#58129,#58130,
#58131,#58132,#58133,#58134,#58135,#58136,#58137,#58138,#58139,#58140,#58141,
#58142,#58143,#58144,#58145,#58146,#58147,#58148,#58149,#58150,#58151,#58152,
#58153,#58154,#58155,#58156,#58157,#58158,#58159,#58160,#58161,#58162,#58163,
#58164,#58165,#58166,#58167,#58168,#58169,#58170,#58171,#58172,#58173,#58174,
#58175,#58176,#58177,#58178,#58179,#58180,#58181,#58182,#58183,#58184,#58185,
#58186,#58187,#58188,#58189,#58190,#58191,#58192,#58193,#58194,#58195,#58196,
#58197,#58198,#58199,#58200,#58201,#58202),(#58203,#58204,#58205,#58206,
#58207,#58208,#58209,#58210,#58211,#58212,#58213,#58214,#58215,#58216,#58217,
#58218,#58219,#58220,#58221,#58222,#58223,#58224,#58225,#58226,#58227,#58228,
#58229,#58230,#58231,#58232,#58233,#58234,#58235,#58236,#58237,#58238,#58239,
#58240,#58241,#58242,#58243,#58244,#58245,#58246,#58247,#58248,#58249,#58250,
#58251,#58252,#58253,#58254,#58255,#58256,#58257,#58258,#58259,#58260,#58261,
#58262,#58263,#58264,#58265,#58266,#58267,#58268,#58269,#58270,#58271,#58272,
#58273,#58274,#58275,#58276,#58277,#58278),(#58279,#58280,#58281,#58282,
#58283,#58284,#58285,#58286,#58287,#58288,#58289,#58290,#58291,#58292,#58293,
#58294,#58295,#58296,#58297,#58298,#58299,#58300,#58301,#58302,#58303,#58304,
#58305,#58306,#58307,#58308,#58309,#58310,#58311,#58312,#58313,#58314,#58315,
#58316,#58317,#58318,#58319,#58320,#58321,#58322,#58323,#58324,#58325,#58326,
#58327,#58328,#58329,#58330,#58331,#58332,#58333,#58334,#58335,#58336,#58337,
#58338,#58339,#58340,#58341,#58342,#58343,#58344,#58345,#58346,#58347,#58348,
#58349,#58350,#58351,#58352,#58353,#58354)),.UNSPECIFIED.,.F.,.F.,.F.,(4,
4),(4,1,1,1,1,1,1,1,1,1,1,1,1,1,1,1,1,1,1,1,1,1,1,1,1,1,1,1,1,1,1,1,1,1,
1,1,1,1,1,1,1,1,1,1,1,1,1,1,1,1,1,1,1,1,1,1,1,1,1,1,1,1,1,1,1,1,1,1,1,1,
1,1,1,4),(0.,0.0986691610045069),(11.6147305479242,12.1093719750971,12.60401340227,
13.5932962566158,14.5825791109615,15.5718619653073,16.561144819653,17.5504276739988,
18.5397105283446,19.5289933826903,20.5182762370361,21.5075590913819,22.4968419457276,
23.4861248000734,24.4754076544192,25.4646905087649,26.4539733631107,27.4432562174565,
28.4325390718022,29.421821926148,30.4111047804938,31.4003876348395,32.3896704891853,
33.3789533435311,34.3682361978768,35.3575190522226,36.3468019065684,37.3360847609141,
38.3253676152599,39.3146504696057,40.3039333239514,41.2932161782972,42.2824990326429,
43.2717818869887,44.2610647413345,45.2503475956803,46.239630450026,47.2289133043718,
48.2181961587175,49.2074790130633,50.1967618674091,51.1860447217548,52.1753275761006,
53.1646104304464,54.1538932847921,55.1431761391379,56.1324589934837,57.1217418478294,
58.1110247021752,59.100307556521,60.0895904108667,61.0788732652125,62.0681561195583,
63.057438973904,64.0467218282498,65.0360046825956,66.0252875369413,67.0145703912871,
68.0038532456329,68.9931360999786,69.9824189543244,70.9717018086701,71.9609846630159,
72.9502675173617,73.9395503717074,74.9288332260532,75.918116080399,76.9073989347447,
77.8966817890905,78.8859646434363,79.875247497782,80.8645303521278,81.3591717793007,
81.8538132064736),.UNSPECIFIED.);
#1463=B_SPLINE_SURFACE_WITH_KNOTS('',3,3,((#58460,#58461,#58462,#58463,
#58464,#58465,#58466,#58467,#58468,#58469,#58470,#58471,#58472,#58473,#58474,
#58475,#58476,#58477,#58478,#58479,#58480,#58481,#58482,#58483,#58484,#58485,
#58486,#58487,#58488,#58489,#58490,#58491,#58492,#58493,#58494,#58495,#58496,
#58497,#58498,#58499,#58500,#58501,#58502,#58503,#58504,#58505,#58506,#58507,
#58508,#58509,#58510,#58511,#58512,#58513,#58514,#58515,#58516,#58517,#58518,
#58519,#58520,#58521,#58522,#58523,#58524,#58525,#58526,#58527,#58528,#58529,
#58530,#58531,#58532,#58533,#58534,#58535),(#58536,#58537,#58538,#58539,
#58540,#58541,#58542,#58543,#58544,#58545,#58546,#58547,#58548,#58549,#58550,
#58551,#58552,#58553,#58554,#58555,#58556,#58557,#58558,#58559,#58560,#58561,
#58562,#58563,#58564,#58565,#58566,#58567,#58568,#58569,#58570,#58571,#58572,
#58573,#58574,#58575,#58576,#58577,#58578,#58579,#58580,#58581,#58582,#58583,
#58584,#58585,#58586,#58587,#58588,#58589,#58590,#58591,#58592,#58593,#58594,
#58595,#58596,#58597,#58598,#58599,#58600,#58601,#58602,#58603,#58604,#58605,
#58606,#58607,#58608,#58609,#58610,#58611),(#58612,#58613,#58614,#58615,
#58616,#58617,#58618,#58619,#58620,#58621,#58622,#58623,#58624,#58625,#58626,
#58627,#58628,#58629,#58630,#58631,#58632,#58633,#58634,#58635,#58636,#58637,
#58638,#58639,#58640,#58641,#58642,#58643,#58644,#58645,#58646,#58647,#58648,
#58649,#58650,#58651,#58652,#58653,#58654,#58655,#58656,#58657,#58658,#58659,
#58660,#58661,#58662,#58663,#58664,#58665,#58666,#58667,#58668,#58669,#58670,
#58671,#58672,#58673,#58674,#58675,#58676,#58677,#58678,#58679,#58680,#58681,
#58682,#58683,#58684,#58685,#58686,#58687),(#58688,#58689,#58690,#58691,
#58692,#58693,#58694,#58695,#58696,#58697,#58698,#58699,#58700,#58701,#58702,
#58703,#58704,#58705,#58706,#58707,#58708,#58709,#58710,#58711,#58712,#58713,
#58714,#58715,#58716,#58717,#58718,#58719,#58720,#58721,#58722,#58723,#58724,
#58725,#58726,#58727,#58728,#58729,#58730,#58731,#58732,#58733,#58734,#58735,
#58736,#58737,#58738,#58739,#58740,#58741,#58742,#58743,#58744,#58745,#58746,
#58747,#58748,#58749,#58750,#58751,#58752,#58753,#58754,#58755,#58756,#58757,
#58758,#58759,#58760,#58761,#58762,#58763)),.UNSPECIFIED.,.F.,.F.,.F.,(4,
4),(4,1,1,1,1,1,1,1,1,1,1,1,1,1,1,1,1,1,1,1,1,1,1,1,1,1,1,1,1,1,1,1,1,1,
1,1,1,1,1,1,1,1,1,1,1,1,1,1,1,1,1,1,1,1,1,1,1,1,1,1,1,1,1,1,1,1,1,1,1,1,
1,1,1,4),(0.,0.0986691610045069),(8.30989595155337,8.80453737872625,9.29917880589914,
10.2884616602449,11.2777445145907,12.2670273689364,13.2563102232822,14.245593077628,
15.2348759319737,16.2241587863195,17.2134416406653,18.202724495011,19.1920073493568,
20.1812902037026,21.1705730580483,22.1598559123941,23.1491387667399,24.1384216210856,
25.1277044754314,26.1169873297771,27.1062701841229,28.0955530384687,29.0848358928144,
30.0741187471602,31.063401601506,32.0526844558517,33.0419673101975,34.0312501645433,
35.020533018889,36.0098158732348,36.9990987275806,37.9883815819263,38.9776644362721,
39.9669472906179,40.9562301449636,41.9455129993094,42.9347958536552,43.9240787080009,
44.9133615623467,45.9026444166925,46.8919272710382,47.881210125384,48.8704929797298,
49.8597758340755,50.8490586884213,51.8383415427671,52.8276243971128,53.8169072514586,
54.8061901058043,55.7954729601501,56.7847558144959,57.7740386688416,58.7633215231874,
59.7526043775332,60.7418872318789,61.7311700862247,62.7204529405705,63.7097357949162,
64.699018649262,65.6883015036078,66.6775843579535,67.6668672122993,68.6561500666451,
69.6454329209908,70.6347157753366,71.6239986296824,72.6132814840281,73.6025643383739,
74.5918471927197,75.5811300470654,76.5704129014112,77.5596957557569,78.0543371829298,
78.5489786101027),.UNSPECIFIED.);
#1464=B_SPLINE_SURFACE_WITH_KNOTS('',2,1,((#64841,#64842),(#64843,#64844),
(#64845,#64846)),.UNSPECIFIED.,.F.,.F.,.F.,(3,3),(2,2),(0.,1.),(0.,0.04),
 .UNSPECIFIED.);
#1465=B_SPLINE_SURFACE_WITH_KNOTS('',2,1,((#64859,#64860),(#64861,#64862),
(#64863,#64864)),.UNSPECIFIED.,.F.,.F.,.F.,(3,3),(2,2),(0.,1.),(0.,0.04),
 .UNSPECIFIED.);
#1466=B_SPLINE_SURFACE_WITH_KNOTS('',2,1,((#64874,#64875),(#64876,#64877),
(#64878,#64879)),.UNSPECIFIED.,.F.,.F.,.F.,(3,3),(2,2),(0.,1.),(0.,0.04),
 .UNSPECIFIED.);
#1467=B_SPLINE_SURFACE_WITH_KNOTS('',2,1,((#64889,#64890),(#64891,#64892),
(#64893,#64894)),.UNSPECIFIED.,.F.,.F.,.F.,(3,3),(2,2),(0.,1.),(0.,0.04),
 .UNSPECIFIED.);
#1468=B_SPLINE_SURFACE_WITH_KNOTS('',2,1,((#64904,#64905),(#64906,#64907),
(#64908,#64909)),.UNSPECIFIED.,.F.,.F.,.F.,(3,3),(2,2),(0.,1.),(0.,0.04),
 .UNSPECIFIED.);
#1469=B_SPLINE_SURFACE_WITH_KNOTS('',2,1,((#64919,#64920),(#64921,#64922),
(#64923,#64924)),.UNSPECIFIED.,.F.,.F.,.F.,(3,3),(2,2),(0.,1.),(0.,0.04),
 .UNSPECIFIED.);
#1470=B_SPLINE_SURFACE_WITH_KNOTS('',2,1,((#64934,#64935),(#64936,#64937),
(#64938,#64939)),.UNSPECIFIED.,.F.,.F.,.F.,(3,3),(2,2),(0.,1.),(0.,0.04),
 .UNSPECIFIED.);
#1471=B_SPLINE_SURFACE_WITH_KNOTS('',2,1,((#64949,#64950),(#64951,#64952),
(#64953,#64954)),.UNSPECIFIED.,.F.,.F.,.F.,(3,3),(2,2),(0.,1.),(0.,0.04),
 .UNSPECIFIED.);
#1472=B_SPLINE_SURFACE_WITH_KNOTS('',2,1,((#64964,#64965),(#64966,#64967),
(#64968,#64969)),.UNSPECIFIED.,.F.,.F.,.F.,(3,3),(2,2),(0.,1.),(0.,0.04),
 .UNSPECIFIED.);
#1473=B_SPLINE_SURFACE_WITH_KNOTS('',2,1,((#64976,#64977),(#64978,#64979),
(#64980,#64981)),.UNSPECIFIED.,.F.,.F.,.F.,(3,3),(2,2),(0.,1.),(0.,0.04),
 .UNSPECIFIED.);
#1474=B_SPLINE_SURFACE_WITH_KNOTS('',2,1,((#64994,#64995),(#64996,#64997),
(#64998,#64999)),.UNSPECIFIED.,.F.,.F.,.F.,(3,3),(2,2),(0.,1.),(0.,0.04),
 .UNSPECIFIED.);
#1475=B_SPLINE_SURFACE_WITH_KNOTS('',2,1,((#65009,#65010),(#65011,#65012),
(#65013,#65014)),.UNSPECIFIED.,.F.,.F.,.F.,(3,3),(2,2),(0.,1.),(0.,0.04),
 .UNSPECIFIED.);
#1476=B_SPLINE_SURFACE_WITH_KNOTS('',2,1,((#65024,#65025),(#65026,#65027),
(#65028,#65029)),.UNSPECIFIED.,.F.,.F.,.F.,(3,3),(2,2),(0.,1.),(0.,0.04),
 .UNSPECIFIED.);
#1477=B_SPLINE_SURFACE_WITH_KNOTS('',2,1,((#65039,#65040),(#65041,#65042),
(#65043,#65044)),.UNSPECIFIED.,.F.,.F.,.F.,(3,3),(2,2),(0.,1.),(0.,0.04),
 .UNSPECIFIED.);
#1478=B_SPLINE_SURFACE_WITH_KNOTS('',2,1,((#65054,#65055),(#65056,#65057),
(#65058,#65059)),.UNSPECIFIED.,.F.,.F.,.F.,(3,3),(2,2),(0.,1.),(0.,0.04),
 .UNSPECIFIED.);
#1479=B_SPLINE_SURFACE_WITH_KNOTS('',2,1,((#65069,#65070),(#65071,#65072),
(#65073,#65074)),.UNSPECIFIED.,.F.,.F.,.F.,(3,3),(2,2),(0.,1.),(0.,0.04),
 .UNSPECIFIED.);
#1480=B_SPLINE_SURFACE_WITH_KNOTS('',2,1,((#65084,#65085),(#65086,#65087),
(#65088,#65089)),.UNSPECIFIED.,.F.,.F.,.F.,(3,3),(2,2),(0.,1.),(0.,0.04),
 .UNSPECIFIED.);
#1481=B_SPLINE_SURFACE_WITH_KNOTS('',2,1,((#65096,#65097),(#65098,#65099),
(#65100,#65101)),.UNSPECIFIED.,.F.,.F.,.F.,(3,3),(2,2),(0.,1.),(0.,0.04),
 .UNSPECIFIED.);
#1482=B_SPLINE_SURFACE_WITH_KNOTS('',2,1,((#65114,#65115),(#65116,#65117),
(#65118,#65119)),.UNSPECIFIED.,.F.,.F.,.F.,(3,3),(2,2),(0.,1.),(0.,0.04),
 .UNSPECIFIED.);
#1483=B_SPLINE_SURFACE_WITH_KNOTS('',2,1,((#65129,#65130),(#65131,#65132),
(#65133,#65134)),.UNSPECIFIED.,.F.,.F.,.F.,(3,3),(2,2),(0.,1.),(0.,0.04),
 .UNSPECIFIED.);
#1484=B_SPLINE_SURFACE_WITH_KNOTS('',2,1,((#65144,#65145),(#65146,#65147),
(#65148,#65149)),.UNSPECIFIED.,.F.,.F.,.F.,(3,3),(2,2),(0.,1.),(0.,0.04),
 .UNSPECIFIED.);
#1485=B_SPLINE_SURFACE_WITH_KNOTS('',2,1,((#65159,#65160),(#65161,#65162),
(#65163,#65164)),.UNSPECIFIED.,.F.,.F.,.F.,(3,3),(2,2),(0.,1.),(0.,0.04),
 .UNSPECIFIED.);
#1486=B_SPLINE_SURFACE_WITH_KNOTS('',2,1,((#65174,#65175),(#65176,#65177),
(#65178,#65179)),.UNSPECIFIED.,.F.,.F.,.F.,(3,3),(2,2),(0.,1.),(0.,0.04),
 .UNSPECIFIED.);
#1487=B_SPLINE_SURFACE_WITH_KNOTS('',2,1,((#65189,#65190),(#65191,#65192),
(#65193,#65194)),.UNSPECIFIED.,.F.,.F.,.F.,(3,3),(2,2),(0.,1.),(0.,0.04),
 .UNSPECIFIED.);
#1488=B_SPLINE_SURFACE_WITH_KNOTS('',2,1,((#65204,#65205),(#65206,#65207),
(#65208,#65209)),.UNSPECIFIED.,.F.,.F.,.F.,(3,3),(2,2),(0.,1.),(0.,0.04),
 .UNSPECIFIED.);
#1489=B_SPLINE_SURFACE_WITH_KNOTS('',2,1,((#65219,#65220),(#65221,#65222),
(#65223,#65224)),.UNSPECIFIED.,.F.,.F.,.F.,(3,3),(2,2),(0.,1.),(0.,0.04),
 .UNSPECIFIED.);
#1490=B_SPLINE_SURFACE_WITH_KNOTS('',2,1,((#65234,#65235),(#65236,#65237),
(#65238,#65239)),.UNSPECIFIED.,.F.,.F.,.F.,(3,3),(2,2),(0.,1.),(0.,0.04),
 .UNSPECIFIED.);
#1491=B_SPLINE_SURFACE_WITH_KNOTS('',2,1,((#65249,#65250),(#65251,#65252),
(#65253,#65254)),.UNSPECIFIED.,.F.,.F.,.F.,(3,3),(2,2),(0.,1.),(0.,0.04),
 .UNSPECIFIED.);
#1492=B_SPLINE_SURFACE_WITH_KNOTS('',2,1,((#65264,#65265),(#65266,#65267),
(#65268,#65269)),.UNSPECIFIED.,.F.,.F.,.F.,(3,3),(2,2),(0.,1.),(0.,0.04),
 .UNSPECIFIED.);
#1493=B_SPLINE_SURFACE_WITH_KNOTS('',2,1,((#65279,#65280),(#65281,#65282),
(#65283,#65284)),.UNSPECIFIED.,.F.,.F.,.F.,(3,3),(2,2),(0.,1.),(0.,0.04),
 .UNSPECIFIED.);
#1494=B_SPLINE_SURFACE_WITH_KNOTS('',2,1,((#65294,#65295),(#65296,#65297),
(#65298,#65299)),.UNSPECIFIED.,.F.,.F.,.F.,(3,3),(2,2),(0.,1.),(0.,0.04),
 .UNSPECIFIED.);
#1495=B_SPLINE_SURFACE_WITH_KNOTS('',2,1,((#65309,#65310),(#65311,#65312),
(#65313,#65314)),.UNSPECIFIED.,.F.,.F.,.F.,(3,3),(2,2),(0.,1.),(0.,0.04),
 .UNSPECIFIED.);
#1496=B_SPLINE_SURFACE_WITH_KNOTS('',2,1,((#65324,#65325),(#65326,#65327),
(#65328,#65329)),.UNSPECIFIED.,.F.,.F.,.F.,(3,3),(2,2),(0.,1.),(0.,0.04),
 .UNSPECIFIED.);
#1497=B_SPLINE_SURFACE_WITH_KNOTS('',2,1,((#65362,#65363),(#65364,#65365),
(#65366,#65367)),.UNSPECIFIED.,.F.,.F.,.F.,(3,3),(2,2),(0.,1.),(0.,0.04),
 .UNSPECIFIED.);
#1498=B_SPLINE_SURFACE_WITH_KNOTS('',2,1,((#65380,#65381),(#65382,#65383),
(#65384,#65385)),.UNSPECIFIED.,.F.,.F.,.F.,(3,3),(2,2),(0.,1.),(0.,0.04),
 .UNSPECIFIED.);
#1499=B_SPLINE_SURFACE_WITH_KNOTS('',2,1,((#65395,#65396),(#65397,#65398),
(#65399,#65400)),.UNSPECIFIED.,.F.,.F.,.F.,(3,3),(2,2),(0.,1.),(0.,0.04),
 .UNSPECIFIED.);
#1500=B_SPLINE_SURFACE_WITH_KNOTS('',2,1,((#65410,#65411),(#65412,#65413),
(#65414,#65415)),.UNSPECIFIED.,.F.,.F.,.F.,(3,3),(2,2),(0.,1.),(0.,0.04),
 .UNSPECIFIED.);
#1501=B_SPLINE_SURFACE_WITH_KNOTS('',2,1,((#65425,#65426),(#65427,#65428),
(#65429,#65430)),.UNSPECIFIED.,.F.,.F.,.F.,(3,3),(2,2),(0.,1.),(0.,0.04),
 .UNSPECIFIED.);
#1502=B_SPLINE_SURFACE_WITH_KNOTS('',2,1,((#65440,#65441),(#65442,#65443),
(#65444,#65445)),.UNSPECIFIED.,.F.,.F.,.F.,(3,3),(2,2),(0.,1.),(0.,0.04),
 .UNSPECIFIED.);
#1503=B_SPLINE_SURFACE_WITH_KNOTS('',2,1,((#65455,#65456),(#65457,#65458),
(#65459,#65460)),.UNSPECIFIED.,.F.,.F.,.F.,(3,3),(2,2),(0.,1.),(0.,0.04),
 .UNSPECIFIED.);
#1504=B_SPLINE_SURFACE_WITH_KNOTS('',2,1,((#65470,#65471),(#65472,#65473),
(#65474,#65475)),.UNSPECIFIED.,.F.,.F.,.F.,(3,3),(2,2),(0.,1.),(0.,0.04),
 .UNSPECIFIED.);
#1505=B_SPLINE_SURFACE_WITH_KNOTS('',2,1,((#65485,#65486),(#65487,#65488),
(#65489,#65490)),.UNSPECIFIED.,.F.,.F.,.F.,(3,3),(2,2),(0.,1.),(0.,0.04),
 .UNSPECIFIED.);
#1506=B_SPLINE_SURFACE_WITH_KNOTS('',2,1,((#65497,#65498),(#65499,#65500),
(#65501,#65502)),.UNSPECIFIED.,.F.,.F.,.F.,(3,3),(2,2),(0.,1.),(0.,0.04),
 .UNSPECIFIED.);
#1507=B_SPLINE_SURFACE_WITH_KNOTS('',2,1,((#65515,#65516),(#65517,#65518),
(#65519,#65520)),.UNSPECIFIED.,.F.,.F.,.F.,(3,3),(2,2),(0.,1.),(0.,0.04),
 .UNSPECIFIED.);
#1508=B_SPLINE_SURFACE_WITH_KNOTS('',2,1,((#65530,#65531),(#65532,#65533),
(#65534,#65535)),.UNSPECIFIED.,.F.,.F.,.F.,(3,3),(2,2),(0.,1.),(0.,0.04),
 .UNSPECIFIED.);
#1509=B_SPLINE_SURFACE_WITH_KNOTS('',2,1,((#65545,#65546),(#65547,#65548),
(#65549,#65550)),.UNSPECIFIED.,.F.,.F.,.F.,(3,3),(2,2),(0.,1.),(0.,0.04),
 .UNSPECIFIED.);
#1510=B_SPLINE_SURFACE_WITH_KNOTS('',2,1,((#65560,#65561),(#65562,#65563),
(#65564,#65565)),.UNSPECIFIED.,.F.,.F.,.F.,(3,3),(2,2),(0.,1.),(0.,0.04),
 .UNSPECIFIED.);
#1511=B_SPLINE_SURFACE_WITH_KNOTS('',2,1,((#65575,#65576),(#65577,#65578),
(#65579,#65580)),.UNSPECIFIED.,.F.,.F.,.F.,(3,3),(2,2),(0.,1.),(0.,0.04),
 .UNSPECIFIED.);
#1512=B_SPLINE_SURFACE_WITH_KNOTS('',2,1,((#65590,#65591),(#65592,#65593),
(#65594,#65595)),.UNSPECIFIED.,.F.,.F.,.F.,(3,3),(2,2),(0.,1.),(0.,0.04),
 .UNSPECIFIED.);
#1513=B_SPLINE_SURFACE_WITH_KNOTS('',2,1,((#65605,#65606),(#65607,#65608),
(#65609,#65610)),.UNSPECIFIED.,.F.,.F.,.F.,(3,3),(2,2),(0.,1.),(0.,0.04),
 .UNSPECIFIED.);
#1514=B_SPLINE_SURFACE_WITH_KNOTS('',2,1,((#65617,#65618),(#65619,#65620),
(#65621,#65622)),.UNSPECIFIED.,.F.,.F.,.F.,(3,3),(2,2),(0.,1.),(0.,0.04),
 .UNSPECIFIED.);
#1515=B_SPLINE_SURFACE_WITH_KNOTS('',2,1,((#65635,#65636),(#65637,#65638),
(#65639,#65640)),.UNSPECIFIED.,.F.,.F.,.F.,(3,3),(2,2),(0.,1.),(0.,0.04),
 .UNSPECIFIED.);
#1516=B_SPLINE_SURFACE_WITH_KNOTS('',2,1,((#65650,#65651),(#65652,#65653),
(#65654,#65655)),.UNSPECIFIED.,.F.,.F.,.F.,(3,3),(2,2),(0.,1.),(0.,0.04),
 .UNSPECIFIED.);
#1517=B_SPLINE_SURFACE_WITH_KNOTS('',2,1,((#65665,#65666),(#65667,#65668),
(#65669,#65670)),.UNSPECIFIED.,.F.,.F.,.F.,(3,3),(2,2),(0.,1.),(0.,0.04),
 .UNSPECIFIED.);
#1518=B_SPLINE_SURFACE_WITH_KNOTS('',2,1,((#65680,#65681),(#65682,#65683),
(#65684,#65685)),.UNSPECIFIED.,.F.,.F.,.F.,(3,3),(2,2),(0.,1.),(0.,0.04),
 .UNSPECIFIED.);
#1519=B_SPLINE_SURFACE_WITH_KNOTS('',2,1,((#65695,#65696),(#65697,#65698),
(#65699,#65700)),.UNSPECIFIED.,.F.,.F.,.F.,(3,3),(2,2),(0.,1.),(0.,0.04),
 .UNSPECIFIED.);
#1520=B_SPLINE_SURFACE_WITH_KNOTS('',2,1,((#65710,#65711),(#65712,#65713),
(#65714,#65715)),.UNSPECIFIED.,.F.,.F.,.F.,(3,3),(2,2),(0.,1.),(0.,0.04),
 .UNSPECIFIED.);
#1521=B_SPLINE_SURFACE_WITH_KNOTS('',2,1,((#65725,#65726),(#65727,#65728),
(#65729,#65730)),.UNSPECIFIED.,.F.,.F.,.F.,(3,3),(2,2),(0.,1.),(0.,0.04),
 .UNSPECIFIED.);
#1522=B_SPLINE_SURFACE_WITH_KNOTS('',2,1,((#65740,#65741),(#65742,#65743),
(#65744,#65745)),.UNSPECIFIED.,.F.,.F.,.F.,(3,3),(2,2),(0.,1.),(0.,0.04),
 .UNSPECIFIED.);
#1523=B_SPLINE_SURFACE_WITH_KNOTS('',2,1,((#65755,#65756),(#65757,#65758),
(#65759,#65760)),.UNSPECIFIED.,.F.,.F.,.F.,(3,3),(2,2),(0.,1.),(0.,0.04),
 .UNSPECIFIED.);
#1524=B_SPLINE_SURFACE_WITH_KNOTS('',2,1,((#65770,#65771),(#65772,#65773),
(#65774,#65775)),.UNSPECIFIED.,.F.,.F.,.F.,(3,3),(2,2),(0.,1.),(0.,0.04),
 .UNSPECIFIED.);
#1525=B_SPLINE_SURFACE_WITH_KNOTS('',2,1,((#65785,#65786),(#65787,#65788),
(#65789,#65790)),.UNSPECIFIED.,.F.,.F.,.F.,(3,3),(2,2),(0.,1.),(0.,0.04),
 .UNSPECIFIED.);
#1526=B_SPLINE_SURFACE_WITH_KNOTS('',2,1,((#65800,#65801),(#65802,#65803),
(#65804,#65805)),.UNSPECIFIED.,.F.,.F.,.F.,(3,3),(2,2),(0.,1.),(0.,0.04),
 .UNSPECIFIED.);
#1527=B_SPLINE_SURFACE_WITH_KNOTS('',2,1,((#65815,#65816),(#65817,#65818),
(#65819,#65820)),.UNSPECIFIED.,.F.,.F.,.F.,(3,3),(2,2),(0.,1.),(0.,0.04),
 .UNSPECIFIED.);
#1528=B_SPLINE_SURFACE_WITH_KNOTS('',2,1,((#65830,#65831),(#65832,#65833),
(#65834,#65835)),.UNSPECIFIED.,.F.,.F.,.F.,(3,3),(2,2),(0.,1.),(0.,0.04),
 .UNSPECIFIED.);
#1529=B_SPLINE_SURFACE_WITH_KNOTS('',2,1,((#65845,#65846),(#65847,#65848),
(#65849,#65850)),.UNSPECIFIED.,.F.,.F.,.F.,(3,3),(2,2),(0.,1.),(0.,0.04),
 .UNSPECIFIED.);
#1530=B_SPLINE_SURFACE_WITH_KNOTS('',3,3,((#66016,#66017,#66018,#66019,
#66020,#66021,#66022,#66023,#66024,#66025,#66026,#66027,#66028,#66029,#66030,
#66031,#66032,#66033,#66034,#66035,#66036,#66037,#66038,#66039,#66040,#66041,
#66042,#66043,#66044,#66045,#66046,#66047,#66048,#66049,#66050,#66051,#66052,
#66053,#66054,#66055,#66056,#66057,#66058,#66059,#66060,#66061,#66062,#66063,
#66064,#66065,#66066,#66067,#66068,#66069,#66070,#66071,#66072,#66073,#66074,
#66075,#66076,#66077,#66078,#66079,#66080,#66081,#66082,#66083,#66084,#66085,
#66086,#66087,#66088,#66089,#66090,#66091,#66092,#66093,#66094,#66095,#66096,
#66097,#66098,#66099,#66100,#66101,#66102,#66103,#66104,#66105,#66106,#66107,
#66108,#66109,#66110,#66111,#66112,#66113,#66114,#66115,#66116,#66117,#66118,
#66119,#66120,#66121,#66122,#66123,#66124,#66125,#66126,#66127,#66128,#66129,
#66130,#66131,#66132,#66133,#66134,#66135,#66136,#66137,#66138,#66139,#66140,
#66141,#66142,#66143,#66144,#66145,#66146,#66147,#66148,#66149,#66150,#66151,
#66152,#66153,#66154,#66155,#66156,#66157,#66158,#66159,#66160,#66161,#66162,
#66163,#66164,#66165,#66166,#66167,#66168,#66169,#66170,#66171,#66172,#66173,
#66174,#66175,#66176,#66177,#66178,#66179,#66180,#66181,#66182,#66183,#66184,
#66185,#66186,#66187,#66188,#66189,#66190,#66191,#66192,#66193,#66194,#66195,
#66196,#66197,#66198,#66199,#66200,#66201,#66202,#66203,#66204,#66205,#66206,
#66207,#66208,#66209,#66210,#66211,#66212,#66213,#66214,#66215,#66216,#66217,
#66218,#66219,#66220,#66221,#66222,#66223,#66224,#66225,#66226,#66227,#66228,
#66229,#66230,#66231,#66232,#66233,#66234,#66235,#66236,#66237,#66238,#66239,
#66240,#66241,#66242,#66243,#66244,#66245,#66246,#66247,#66248,#66249,#66250,
#66251,#66252,#66253,#66254,#66255,#66256,#66257,#66258,#66259,#66260,#66261,
#66262,#66263,#66264,#66265,#66266,#66267,#66268,#66269,#66270,#66271,#66272,
#66273,#66274,#66275,#66276,#66277,#66278,#66279,#66280,#66281,#66282,#66283,
#66284,#66285,#66286,#66287,#66288,#66289,#66290,#66291,#66292,#66293,#66294,
#66295,#66296,#66297,#66298,#66299,#66300,#66301,#66302,#66303,#66304,#66305,
#66306,#66307,#66308,#66309,#66310,#66311,#66312,#66313,#66314,#66315,#66316,
#66317,#66318,#66319,#66320,#66321,#66322,#66323,#66324,#66325,#66326,#66327,
#66328,#66329,#66330,#66331,#66332,#66333,#66334,#66335,#66336,#66337,#66338,
#66339,#66340,#66341,#66342,#66343,#66344,#66345,#66346,#66347,#66348,#66349,
#66350,#66351,#66352,#66353,#66354,#66355,#66356,#66357,#66358,#66359,#66360,
#66361,#66362,#66363,#66364,#66365,#66366,#66367,#66368,#66369,#66370,#66371,
#66372,#66373,#66374,#66375,#66376,#66377,#66378,#66379,#66380,#66381,#66382,
#66383,#66384,#66385,#66386,#66387,#66388,#66389,#66390,#66391,#66392,#66393,
#66394,#66395,#66396,#66397,#66398,#66399,#66400,#66401,#66402,#66403,#66404,
#66405,#66406,#66407,#66408,#66409,#66410,#66411,#66412,#66413,#66414,#66415,
#66416,#66417,#66418,#66419,#66420,#66421,#66422,#66423,#66424,#66425,#66426,
#66427,#66428,#66429,#66430,#66431,#66432,#66433,#66434,#66435,#66436,#66437,
#66438,#66439,#66440,#66441,#66442,#66443,#66444,#66445,#66446,#66447,#66448,
#66449,#66450,#66451,#66452,#66453,#66454,#66455,#66456,#66457,#66458,#66459,
#66460,#66461,#66462,#66463,#66464,#66465,#66466,#66467,#66468,#66469,#66470,
#66471,#66472,#66473,#66474,#66475,#66476,#66477,#66478,#66479,#66480,#66481,
#66482,#66483,#66484,#66485,#66486,#66487,#66488,#66489,#66490,#66491,#66492,
#66493,#66494,#66495,#66496,#66497,#66498,#66499,#66500,#66501,#66502,#66503,
#66504,#66505,#66506,#66507,#66508,#66509,#66510,#66511,#66512,#66513,#66514,
#66515,#66516,#66517,#66518,#66519,#66520,#66521,#66522,#66523,#66524,#66525,
#66526,#66527,#66528,#66529,#66530,#66531,#66532,#66533,#66534,#66535,#66536,
#66537,#66538,#66539,#66540,#66541,#66542,#66543,#66544,#66545,#66546,#66547,
#66548,#66549,#66550,#66551,#66552,#66553),(#66554,#66555,#66556,#66557,
#66558,#66559,#66560,#66561,#66562,#66563,#66564,#66565,#66566,#66567,#66568,
#66569,#66570,#66571,#66572,#66573,#66574,#66575,#66576,#66577,#66578,#66579,
#66580,#66581,#66582,#66583,#66584,#66585,#66586,#66587,#66588,#66589,#66590,
#66591,#66592,#66593,#66594,#66595,#66596,#66597,#66598,#66599,#66600,#66601,
#66602,#66603,#66604,#66605,#66606,#66607,#66608,#66609,#66610,#66611,#66612,
#66613,#66614,#66615,#66616,#66617,#66618,#66619,#66620,#66621,#66622,#66623,
#66624,#66625,#66626,#66627,#66628,#66629,#66630,#66631,#66632,#66633,#66634,
#66635,#66636,#66637,#66638,#66639,#66640,#66641,#66642,#66643,#66644,#66645,
#66646,#66647,#66648,#66649,#66650,#66651,#66652,#66653,#66654,#66655,#66656,
#66657,#66658,#66659,#66660,#66661,#66662,#66663,#66664,#66665,#66666,#66667,
#66668,#66669,#66670,#66671,#66672,#66673,#66674,#66675,#66676,#66677,#66678,
#66679,#66680,#66681,#66682,#66683,#66684,#66685,#66686,#66687,#66688,#66689,
#66690,#66691,#66692,#66693,#66694,#66695,#66696,#66697,#66698,#66699,#66700,
#66701,#66702,#66703,#66704,#66705,#66706,#66707,#66708,#66709,#66710,#66711,
#66712,#66713,#66714,#66715,#66716,#66717,#66718,#66719,#66720,#66721,#66722,
#66723,#66724,#66725,#66726,#66727,#66728,#66729,#66730,#66731,#66732,#66733,
#66734,#66735,#66736,#66737,#66738,#66739,#66740,#66741,#66742,#66743,#66744,
#66745,#66746,#66747,#66748,#66749,#66750,#66751,#66752,#66753,#66754,#66755,
#66756,#66757,#66758,#66759,#66760,#66761,#66762,#66763,#66764,#66765,#66766,
#66767,#66768,#66769,#66770,#66771,#66772,#66773,#66774,#66775,#66776,#66777,
#66778,#66779,#66780,#66781,#66782,#66783,#66784,#66785,#66786,#66787,#66788,
#66789,#66790,#66791,#66792,#66793,#66794,#66795,#66796,#66797,#66798,#66799,
#66800,#66801,#66802,#66803,#66804,#66805,#66806,#66807,#66808,#66809,#66810,
#66811,#66812,#66813,#66814,#66815,#66816,#66817,#66818,#66819,#66820,#66821,
#66822,#66823,#66824,#66825,#66826,#66827,#66828,#66829,#66830,#66831,#66832,
#66833,#66834,#66835,#66836,#66837,#66838,#66839,#66840,#66841,#66842,#66843,
#66844,#66845,#66846,#66847,#66848,#66849,#66850,#66851,#66852,#66853,#66854,
#66855,#66856,#66857,#66858,#66859,#66860,#66861,#66862,#66863,#66864,#66865,
#66866,#66867,#66868,#66869,#66870,#66871,#66872,#66873,#66874,#66875,#66876,
#66877,#66878,#66879,#66880,#66881,#66882,#66883,#66884,#66885,#66886,#66887,
#66888,#66889,#66890,#66891,#66892,#66893,#66894,#66895,#66896,#66897,#66898,
#66899,#66900,#66901,#66902,#66903,#66904,#66905,#66906,#66907,#66908,#66909,
#66910,#66911,#66912,#66913,#66914,#66915,#66916,#66917,#66918,#66919,#66920,
#66921,#66922,#66923,#66924,#66925,#66926,#66927,#66928,#66929,#66930,#66931,
#66932,#66933,#66934,#66935,#66936,#66937,#66938,#66939,#66940,#66941,#66942,
#66943,#66944,#66945,#66946,#66947,#66948,#66949,#66950,#66951,#66952,#66953,
#66954,#66955,#66956,#66957,#66958,#66959,#66960,#66961,#66962,#66963,#66964,
#66965,#66966,#66967,#66968,#66969,#66970,#66971,#66972,#66973,#66974,#66975,
#66976,#66977,#66978,#66979,#66980,#66981,#66982,#66983,#66984,#66985,#66986,
#66987,#66988,#66989,#66990,#66991,#66992,#66993,#66994,#66995,#66996,#66997,
#66998,#66999,#67000,#67001,#67002,#67003,#67004,#67005,#67006,#67007,#67008,
#67009,#67010,#67011,#67012,#67013,#67014,#67015,#67016,#67017,#67018,#67019,
#67020,#67021,#67022,#67023,#67024,#67025,#67026,#67027,#67028,#67029,#67030,
#67031,#67032,#67033,#67034,#67035,#67036,#67037,#67038,#67039,#67040,#67041,
#67042,#67043,#67044,#67045,#67046,#67047,#67048,#67049,#67050,#67051,#67052,
#67053,#67054,#67055,#67056,#67057,#67058,#67059,#67060,#67061,#67062,#67063,
#67064,#67065,#67066,#67067,#67068,#67069,#67070,#67071,#67072,#67073,#67074,
#67075,#67076,#67077,#67078,#67079,#67080,#67081,#67082,#67083,#67084,#67085,
#67086,#67087,#67088,#67089,#67090,#67091),(#67092,#67093,#67094,#67095,
#67096,#67097,#67098,#67099,#67100,#67101,#67102,#67103,#67104,#67105,#67106,
#67107,#67108,#67109,#67110,#67111,#67112,#67113,#67114,#67115,#67116,#67117,
#67118,#67119,#67120,#67121,#67122,#67123,#67124,#67125,#67126,#67127,#67128,
#67129,#67130,#67131,#67132,#67133,#67134,#67135,#67136,#67137,#67138,#67139,
#67140,#67141,#67142,#67143,#67144,#67145,#67146,#67147,#67148,#67149,#67150,
#67151,#67152,#67153,#67154,#67155,#67156,#67157,#67158,#67159,#67160,#67161,
#67162,#67163,#67164,#67165,#67166,#67167,#67168,#67169,#67170,#67171,#67172,
#67173,#67174,#67175,#67176,#67177,#67178,#67179,#67180,#67181,#67182,#67183,
#67184,#67185,#67186,#67187,#67188,#67189,#67190,#67191,#67192,#67193,#67194,
#67195,#67196,#67197,#67198,#67199,#67200,#67201,#67202,#67203,#67204,#67205,
#67206,#67207,#67208,#67209,#67210,#67211,#67212,#67213,#67214,#67215,#67216,
#67217,#67218,#67219,#67220,#67221,#67222,#67223,#67224,#67225,#67226,#67227,
#67228,#67229,#67230,#67231,#67232,#67233,#67234,#67235,#67236,#67237,#67238,
#67239,#67240,#67241,#67242,#67243,#67244,#67245,#67246,#67247,#67248,#67249,
#67250,#67251,#67252,#67253,#67254,#67255,#67256,#67257,#67258,#67259,#67260,
#67261,#67262,#67263,#67264,#67265,#67266,#67267,#67268,#67269,#67270,#67271,
#67272,#67273,#67274,#67275,#67276,#67277,#67278,#67279,#67280,#67281,#67282,
#67283,#67284,#67285,#67286,#67287,#67288,#67289,#67290,#67291,#67292,#67293,
#67294,#67295,#67296,#67297,#67298,#67299,#67300,#67301,#67302,#67303,#67304,
#67305,#67306,#67307,#67308,#67309,#67310,#67311,#67312,#67313,#67314,#67315,
#67316,#67317,#67318,#67319,#67320,#67321,#67322,#67323,#67324,#67325,#67326,
#67327,#67328,#67329,#67330,#67331,#67332,#67333,#67334,#67335,#67336,#67337,
#67338,#67339,#67340,#67341,#67342,#67343,#67344,#67345,#67346,#67347,#67348,
#67349,#67350,#67351,#67352,#67353,#67354,#67355,#67356,#67357,#67358,#67359,
#67360,#67361,#67362,#67363,#67364,#67365,#67366,#67367,#67368,#67369,#67370,
#67371,#67372,#67373,#67374,#67375,#67376,#67377,#67378,#67379,#67380,#67381,
#67382,#67383,#67384,#67385,#67386,#67387,#67388,#67389,#67390,#67391,#67392,
#67393,#67394,#67395,#67396,#67397,#67398,#67399,#67400,#67401,#67402,#67403,
#67404,#67405,#67406,#67407,#67408,#67409,#67410,#67411,#67412,#67413,#67414,
#67415,#67416,#67417,#67418,#67419,#67420,#67421,#67422,#67423,#67424,#67425,
#67426,#67427,#67428,#67429,#67430,#67431,#67432,#67433,#67434,#67435,#67436,
#67437,#67438,#67439,#67440,#67441,#67442,#67443,#67444,#67445,#67446,#67447,
#67448,#67449,#67450,#67451,#67452,#67453,#67454,#67455,#67456,#67457,#67458,
#67459,#67460,#67461,#67462,#67463,#67464,#67465,#67466,#67467,#67468,#67469,
#67470,#67471,#67472,#67473,#67474,#67475,#67476,#67477,#67478,#67479,#67480,
#67481,#67482,#67483,#67484,#67485,#67486,#67487,#67488,#67489,#67490,#67491,
#67492,#67493,#67494,#67495,#67496,#67497,#67498,#67499,#67500,#67501,#67502,
#67503,#67504,#67505,#67506,#67507,#67508,#67509,#67510,#67511,#67512,#67513,
#67514,#67515,#67516,#67517,#67518,#67519,#67520,#67521,#67522,#67523,#67524,
#67525,#67526,#67527,#67528,#67529,#67530,#67531,#67532,#67533,#67534,#67535,
#67536,#67537,#67538,#67539,#67540,#67541,#67542,#67543,#67544,#67545,#67546,
#67547,#67548,#67549,#67550,#67551,#67552,#67553,#67554,#67555,#67556,#67557,
#67558,#67559,#67560,#67561,#67562,#67563,#67564,#67565,#67566,#67567,#67568,
#67569,#67570,#67571,#67572,#67573,#67574,#67575,#67576,#67577,#67578,#67579,
#67580,#67581,#67582,#67583,#67584,#67585,#67586,#67587,#67588,#67589,#67590,
#67591,#67592,#67593,#67594,#67595,#67596,#67597,#67598,#67599,#67600,#67601,
#67602,#67603,#67604,#67605,#67606,#67607,#67608,#67609,#67610,#67611,#67612,
#67613,#67614,#67615,#67616,#67617,#67618,#67619,#67620,#67621,#67622,#67623,
#67624,#67625,#67626,#67627,#67628,#67629),(#67630,#67631,#67632,#67633,
#67634,#67635,#67636,#67637,#67638,#67639,#67640,#67641,#67642,#67643,#67644,
#67645,#67646,#67647,#67648,#67649,#67650,#67651,#67652,#67653,#67654,#67655,
#67656,#67657,#67658,#67659,#67660,#67661,#67662,#67663,#67664,#67665,#67666,
#67667,#67668,#67669,#67670,#67671,#67672,#67673,#67674,#67675,#67676,#67677,
#67678,#67679,#67680,#67681,#67682,#67683,#67684,#67685,#67686,#67687,#67688,
#67689,#67690,#67691,#67692,#67693,#67694,#67695,#67696,#67697,#67698,#67699,
#67700,#67701,#67702,#67703,#67704,#67705,#67706,#67707,#67708,#67709,#67710,
#67711,#67712,#67713,#67714,#67715,#67716,#67717,#67718,#67719,#67720,#67721,
#67722,#67723,#67724,#67725,#67726,#67727,#67728,#67729,#67730,#67731,#67732,
#67733,#67734,#67735,#67736,#67737,#67738,#67739,#67740,#67741,#67742,#67743,
#67744,#67745,#67746,#67747,#67748,#67749,#67750,#67751,#67752,#67753,#67754,
#67755,#67756,#67757,#67758,#67759,#67760,#67761,#67762,#67763,#67764,#67765,
#67766,#67767,#67768,#67769,#67770,#67771,#67772,#67773,#67774,#67775,#67776,
#67777,#67778,#67779,#67780,#67781,#67782,#67783,#67784,#67785,#67786,#67787,
#67788,#67789,#67790,#67791,#67792,#67793,#67794,#67795,#67796,#67797,#67798,
#67799,#67800,#67801,#67802,#67803,#67804,#67805,#67806,#67807,#67808,#67809,
#67810,#67811,#67812,#67813,#67814,#67815,#67816,#67817,#67818,#67819,#67820,
#67821,#67822,#67823,#67824,#67825,#67826,#67827,#67828,#67829,#67830,#67831,
#67832,#67833,#67834,#67835,#67836,#67837,#67838,#67839,#67840,#67841,#67842,
#67843,#67844,#67845,#67846,#67847,#67848,#67849,#67850,#67851,#67852,#67853,
#67854,#67855,#67856,#67857,#67858,#67859,#67860,#67861,#67862,#67863,#67864,
#67865,#67866,#67867,#67868,#67869,#67870,#67871,#67872,#67873,#67874,#67875,
#67876,#67877,#67878,#67879,#67880,#67881,#67882,#67883,#67884,#67885,#67886,
#67887,#67888,#67889,#67890,#67891,#67892,#67893,#67894,#67895,#67896,#67897,
#67898,#67899,#67900,#67901,#67902,#67903,#67904,#67905,#67906,#67907,#67908,
#67909,#67910,#67911,#67912,#67913,#67914,#67915,#67916,#67917,#67918,#67919,
#67920,#67921,#67922,#67923,#67924,#67925,#67926,#67927,#67928,#67929,#67930,
#67931,#67932,#67933,#67934,#67935,#67936,#67937,#67938,#67939,#67940,#67941,
#67942,#67943,#67944,#67945,#67946,#67947,#67948,#67949,#67950,#67951,#67952,
#67953,#67954,#67955,#67956,#67957,#67958,#67959,#67960,#67961,#67962,#67963,
#67964,#67965,#67966,#67967,#67968,#67969,#67970,#67971,#67972,#67973,#67974,
#67975,#67976,#67977,#67978,#67979,#67980,#67981,#67982,#67983,#67984,#67985,
#67986,#67987,#67988,#67989,#67990,#67991,#67992,#67993,#67994,#67995,#67996,
#67997,#67998,#67999,#68000,#68001,#68002,#68003,#68004,#68005,#68006,#68007,
#68008,#68009,#68010,#68011,#68012,#68013,#68014,#68015,#68016,#68017,#68018,
#68019,#68020,#68021,#68022,#68023,#68024,#68025,#68026,#68027,#68028,#68029,
#68030,#68031,#68032,#68033,#68034,#68035,#68036,#68037,#68038,#68039,#68040,
#68041,#68042,#68043,#68044,#68045,#68046,#68047,#68048,#68049,#68050,#68051,
#68052,#68053,#68054,#68055,#68056,#68057,#68058,#68059,#68060,#68061,#68062,
#68063,#68064,#68065,#68066,#68067,#68068,#68069,#68070,#68071,#68072,#68073,
#68074,#68075,#68076,#68077,#68078,#68079,#68080,#68081,#68082,#68083,#68084,
#68085,#68086,#68087,#68088,#68089,#68090,#68091,#68092,#68093,#68094,#68095,
#68096,#68097,#68098,#68099,#68100,#68101,#68102,#68103,#68104,#68105,#68106,
#68107,#68108,#68109,#68110,#68111,#68112,#68113,#68114,#68115,#68116,#68117,
#68118,#68119,#68120,#68121,#68122,#68123,#68124,#68125,#68126,#68127,#68128,
#68129,#68130,#68131,#68132,#68133,#68134,#68135,#68136,#68137,#68138,#68139,
#68140,#68141,#68142,#68143,#68144,#68145,#68146,#68147,#68148,#68149,#68150,
#68151,#68152,#68153,#68154,#68155,#68156,#68157,#68158,#68159,#68160,#68161,
#68162,#68163,#68164,#68165,#68166,#68167)),.UNSPECIFIED.,.F.,.F.,.F.,(4,
4),(4,1,1,1,1,1,1,1,1,1,1,1,1,1,1,1,1,1,1,1,1,1,1,1,1,1,1,1,1,1,1,1,1,1,
1,1,1,1,1,1,1,1,1,1,1,1,1,1,1,1,1,1,1,1,1,1,1,1,1,1,1,1,1,1,1,1,1,1,1,1,
1,1,1,1,1,1,1,1,1,1,1,1,1,1,1,1,1,1,1,1,1,1,1,1,1,1,1,1,1,1,1,1,1,1,1,1,
1,1,1,1,1,1,1,1,1,1,1,1,1,1,1,1,1,1,1,1,1,1,1,1,1,1,1,1,1,1,1,1,1,1,1,1,
1,1,1,1,1,1,1,1,1,1,1,1,1,1,1,1,1,1,1,1,1,1,1,1,1,1,1,1,1,1,1,1,1,1,1,1,
1,1,1,1,1,1,1,1,1,1,1,1,1,1,1,1,1,1,1,1,1,1,1,1,1,1,1,1,1,1,1,1,1,1,1,1,
1,1,1,1,1,1,1,1,1,1,1,1,1,1,1,1,1,1,1,1,1,1,1,1,1,1,1,1,1,1,1,1,1,1,1,1,
1,1,1,1,1,1,1,1,1,1,1,1,1,1,1,1,1,1,1,1,1,1,1,1,1,1,1,1,1,1,1,1,1,1,1,1,
1,1,1,1,1,1,1,1,1,1,1,1,1,1,1,1,1,1,1,1,1,1,1,1,1,1,1,1,1,1,1,1,1,1,1,1,
1,1,1,1,1,1,1,1,1,1,1,1,1,1,1,1,1,1,1,1,1,1,1,1,1,1,1,1,1,1,1,1,1,1,1,1,
1,1,1,1,1,1,1,1,1,1,1,1,1,1,1,1,1,1,1,1,1,1,1,1,1,1,1,1,1,1,1,1,1,1,1,1,
1,1,1,1,1,1,1,1,1,1,1,1,1,1,1,1,1,1,1,1,1,1,1,1,1,1,1,1,1,1,1,1,1,1,1,1,
1,1,1,1,1,1,1,1,1,1,1,1,1,1,1,1,1,1,1,1,1,1,1,1,1,1,1,1,1,1,1,1,1,1,1,1,
1,1,1,1,1,1,1,1,1,1,1,1,1,1,1,1,1,1,1,1,1,1,1,1,1,1,1,1,1,1,1,1,1,1,1,1,
1,1,1,1,1,1,1,1,1,1,1,1,1,1,1,1,1,1,1,1,1,1,1,1,1,1,1,1,1,1,1,1,1,4),(0.,
0.132097741590587),(8.30112925462677,8.80022146583195,9.29931367703713,
9.79840588824231,10.2974980994475,11.2956825218578,12.2938669442682,13.2920513666786,
13.7911435778838,14.2902357890889,14.7893280002941,15.2884202114993,16.2866046339097,
16.7856968451148,17.28478905632,18.2829734787304,19.2811579011407,20.2793423235511,
20.7784345347563,21.2775267459615,21.7766189571666,22.2757111683718,23.2738955907822,
23.7729878019874,24.2720800131925,25.2702644356029,26.2684488580133,27.2666332804236,
27.7657254916288,28.264817702834,28.7639099140392,29.2630021252443,30.2611865476547,
30.7602787588599,31.2593709700651,32.2575553924754,33.2557398148858,34.2539242372961,
34.7530164485013,35.2521086597065,35.7512008709117,36.2502930821169,37.2484775045272,
37.7475697157324,38.2466619269376,39.2448463493479,40.2430307717583,41.2412151941687,
41.7403074053738,42.239399616579,42.7384918277842,43.2375840389894,44.2357684613998,
44.7348606726049,45.2339528838101,46.2321373062205,47.2303217286308,48.2285061510412,
48.7275983622464,49.2266905734515,49.7257827846567,50.2248749958619,51.2230594182723,
51.7221516294775,52.2212438406826,53.219428263093,54.2176126855034,55.2157971079137,
55.7148893191189,56.2139815303241,56.7130737415293,57.2121659527344,58.2103503751448,
58.70944258635,59.2085347975552,60.2067192199655,61.2049036423759,62.2030880647862,
62.7021802759914,63.2012724871966,63.7003646984018,64.199456909607,65.1976413320173,
65.6967335432225,66.1958257544277,67.194010176838,68.1921945992484,69.1903790216588,
69.689471232864,70.1885634440691,70.6876556552743,71.1867478664795,72.1849322888899,
72.684024500095,73.1831167113002,74.1813011337106,75.1794855561209,76.1776699785313,
76.6767621897365,77.1758544009417,77.6749466121468,78.174038823352,79.1722232457624,
79.6713154569676,80.1704076681727,81.1685920905831,82.1667765129935,83.1649609354038,
83.664053146609,84.1631453578142,84.6622375690194,85.1613297802245,86.1595142026349,
86.6586064138401,87.1576986250453,88.1558830474556,89.154067469866,90.1522518922763,
90.6513441034815,91.1504363146867,91.6495285258919,92.1486207370971,93.1468051595074,
93.6458973707126,94.1449895819178,95.1431740043281,96.1413584267385,97.1395428491489,
97.638635060354,98.1377272715592,98.6368194827644,99.1359116939696,100.13409611638,
100.633188327585,101.13228053879,102.130464961201,103.128649383611,104.126833806021,
104.625926017227,105.125018228432,105.624110439637,106.123202650842,107.121387073252,
107.620479284458,108.119571495663,109.117755918073,110.115940340484,111.114124762894,
111.613216974099,112.112309185304,112.611401396509,113.110493607715,114.108678030125,
114.60777024133,115.106862452535,116.105046874946,117.103231297356,118.101415719766,
118.600507930972,119.099600142177,119.598692353382,120.097784564587,121.095968986998,
121.595061198203,122.094153409408,123.092337831818,124.090522254229,125.088706676639,
125.587798887844,126.086891099049,126.585983310255,127.08507552146,128.08325994387,
128.582352155075,129.08144436628,130.079628788691,131.077813211101,132.075997633511,
132.575089844717,133.074182055922,133.573274267127,134.072366478332,135.070550900743,
135.569643111948,136.068735323153,137.066919745563,138.065104167974,139.063288590384,
139.562380801589,140.061473012794,140.560565224,141.059657435205,142.057841857615,
142.55693406882,143.056026280025,144.054210702436,145.052395124846,146.050579547257,
146.549671758462,147.048763969667,147.547856180872,148.046948392077,149.045132814488,
149.544225025693,150.043317236898,151.041501659308,152.039686081719,153.037870504129,
153.536962715334,154.036054926539,154.535147137745,155.03423934895,156.03242377136,
156.531515982565,157.030608193771,158.028792616181,159.026977038591,160.025161461002,
160.524253672207,161.023345883412,161.522438094617,162.021530305822,163.019714728233,
163.518806939438,164.017899150643,165.016083573053,166.014267995464,167.012452417874,
167.511544629079,168.010636840284,168.50972905149,169.008821262695,170.007005685105,
170.50609789631,171.005190107516,172.003374529926,173.001558952336,173.999743374747,
174.498835585952,174.997927797157,175.497020008362,175.996112219567,176.994296641978,
177.493388853183,177.992481064388,178.990665486798,179.988849909209,180.987034331619,
181.486126542824,181.98521875403,182.484310965235,182.98340317644,183.98158759885,
184.480679810055,184.979772021261,185.977956443671,186.976140866081,187.974325288492,
188.473417499697,188.972509710902,189.471601922107,189.970694133312,190.968878555723,
191.467970766928,191.967062978133,192.965247400543,193.963431822954,194.961616245364,
195.959800667775,196.957985090185,197.956169512595,198.954353935006,199.453446146211,
199.952538357416,200.950722779826,201.449814991032,201.948907202237,202.447999413442,
202.947091624647,203.945276047057,204.943460469468,205.941644891878,206.440737103083,
206.939829314289,207.938013736699,208.437105947904,208.936198159109,209.435290370314,
209.93438258152,210.93256700393,211.93075142634,212.928935848751,213.428028059956,
213.927120271161,214.925304693571,215.424396904777,215.923489115982,216.422581327187,
216.921673538392,217.919857960803,218.918042383213,219.916226805623,220.415319016828,
220.914411228034,221.912595650444,222.411687861649,222.910780072854,223.40987228406,
223.908964495265,224.907148917675,225.905333340085,226.903517762496,227.402609973701,
227.901702184906,228.899886607316,229.398978818522,229.898071029727,230.397163240932,
230.896255452137,231.894439874548,232.892624296958,233.890808719368,234.389900930573,
234.888993141779,235.887177564189,236.386269775394,236.885361986599,237.384454197805,
237.88354640901,238.88173083142,239.87991525383,240.878099676241,241.377191887446,
241.876284098651,242.874468521062,243.373560732267,243.872652943472,244.371745154677,
244.870837365882,245.869021788293,246.867206210703,247.865390633113,248.364482844319,
248.863575055524,249.861759477934,250.360851689139,250.859943900344,251.35903611155,
251.858128322755,252.856312745165,253.854497167575,254.852681589986,255.351773801191,
255.850866012396,256.849050434807,257.348142646012,257.847234857217,258.346327068422,
258.845419279627,259.843603702038,260.841788124448,261.839972546858,262.339064758064,
262.838156969269,263.836341391679,264.335433602884,264.834525814089,265.333618025295,
265.8327102365,266.83089465891,267.829079081321,268.827263503731,269.326355714936,
269.825447926141,270.823632348552,271.322724559757,271.821816770962,272.320908982167,
272.820001193372,273.818185615783,274.816370038193,275.814554460603,276.313646671809,
276.812738883014,277.810923305424,278.310015516629,278.809107727834,279.30819993904,
279.807292150245,280.805476572655,281.803660995066,282.801845417476,283.300937628681,
283.800029839886,284.798214262297,285.297306473502,285.796398684707,286.295490895912,
286.794583107117,287.792767529528,288.790951951938,289.789136374348,290.288228585554,
290.787320796759,291.785505219169,292.284597430374,292.78368964158,293.282781852785,
293.78187406399,294.7800584864,295.778242908811,296.776427331221,297.275519542426,
297.774611753631,298.772796176042,299.271888387247,299.770980598452,300.270072809657,
300.769165020862,301.767349443273,302.765533865683,303.763718288094,304.262810499299,
304.761902710504,305.760087132914,306.259179344119,306.758271555325,307.25736376653,
307.756455977735,308.754640400145,309.752824822556,310.751009244966,311.250101456171,
311.749193667376,312.747378089787,313.246470300992,313.745562512197,314.244654723402,
314.743746934607,315.741931357018,316.740115779428,317.738300201839,318.237392413044,
318.736484624249,319.734669046659,320.233761257864,320.73285346907,321.231945680275,
321.73103789148,322.72922231389,323.727406736301,324.725591158711,325.224683369916,
325.723775581121,326.721960003532,327.221052214737,327.720144425942,328.219236637147,
328.718328848352,329.716513270763,330.714697693173,331.712882115584,332.211974326789,
332.711066537994,333.709250960404,334.208343171609,334.707435382815,335.20652759402,
335.705619805225,336.703804227635,337.701988650046,338.700173072456,339.199265283661,
339.698357494866,340.696541917277,341.195634128482,341.694726339687,342.193818550892,
342.692910762098,343.691095184508,344.689279606918,345.687464029329,346.186556240534,
346.685648451739,347.683832874149,348.182925085355,348.68201729656,349.181109507765,
349.68020171897,350.67838614138,351.676570563791,352.674754986201,353.173847197406,
353.672939408612,354.671123831022,355.170216042227,355.669308253432,356.168400464637,
356.667492675843,357.665677098253,358.663861520663,359.662045943074,360.161138154279,
360.660230365484,361.658414787894,362.1575069991,362.656599210305,363.15569142151,
363.654783632715,364.652968055125,365.651152477536,366.649336899946,367.148429111151,
367.647521322357,368.645705744767,369.144797955972,369.643890167177,370.142982378382,
370.642074589588,371.640259011998,372.638443434408,373.636627856819,374.135720068024,
374.634812279229,375.632996701639,376.132088912845,376.63118112405,377.130273335255,
377.62936554646,378.627549968871,379.625734391281,380.623918813691,381.123011024896,
381.622103236102,382.121195447307,382.620287658512),.UNSPECIFIED.);
#1531=B_SPLINE_SURFACE_WITH_KNOTS('',3,3,((#68350,#68351,#68352,#68353,
#68354,#68355,#68356,#68357,#68358,#68359,#68360,#68361,#68362,#68363,#68364,
#68365,#68366,#68367,#68368,#68369,#68370,#68371,#68372,#68373,#68374,#68375,
#68376,#68377,#68378,#68379,#68380,#68381,#68382,#68383,#68384,#68385,#68386,
#68387,#68388,#68389,#68390,#68391,#68392,#68393,#68394,#68395,#68396,#68397,
#68398,#68399,#68400,#68401,#68402,#68403,#68404,#68405,#68406,#68407,#68408,
#68409,#68410,#68411,#68412,#68413,#68414,#68415,#68416,#68417,#68418,#68419,
#68420,#68421,#68422,#68423,#68424,#68425,#68426,#68427,#68428,#68429,#68430,
#68431,#68432,#68433,#68434,#68435,#68436,#68437,#68438,#68439,#68440,#68441,
#68442,#68443,#68444,#68445,#68446,#68447,#68448,#68449,#68450,#68451,#68452,
#68453,#68454,#68455,#68456,#68457,#68458,#68459,#68460,#68461,#68462,#68463,
#68464,#68465,#68466,#68467,#68468,#68469,#68470,#68471,#68472,#68473,#68474,
#68475,#68476,#68477,#68478,#68479,#68480,#68481,#68482,#68483,#68484,#68485,
#68486,#68487,#68488,#68489,#68490,#68491,#68492,#68493,#68494,#68495,#68496,
#68497,#68498,#68499,#68500,#68501,#68502,#68503,#68504,#68505,#68506,#68507,
#68508,#68509,#68510,#68511,#68512,#68513,#68514,#68515,#68516,#68517,#68518,
#68519,#68520,#68521,#68522,#68523,#68524,#68525,#68526,#68527,#68528,#68529,
#68530,#68531,#68532,#68533,#68534,#68535,#68536,#68537,#68538,#68539,#68540,
#68541,#68542,#68543,#68544,#68545,#68546,#68547,#68548,#68549,#68550,#68551,
#68552,#68553,#68554,#68555,#68556,#68557,#68558,#68559,#68560,#68561,#68562,
#68563,#68564,#68565,#68566,#68567,#68568,#68569,#68570,#68571,#68572,#68573,
#68574,#68575,#68576,#68577,#68578,#68579,#68580,#68581,#68582,#68583,#68584,
#68585,#68586,#68587,#68588,#68589,#68590,#68591,#68592,#68593,#68594,#68595,
#68596,#68597,#68598,#68599,#68600,#68601,#68602,#68603,#68604,#68605,#68606,
#68607,#68608,#68609,#68610,#68611,#68612,#68613,#68614,#68615,#68616,#68617,
#68618,#68619,#68620,#68621,#68622,#68623,#68624,#68625,#68626,#68627,#68628,
#68629,#68630,#68631,#68632,#68633,#68634,#68635,#68636,#68637,#68638,#68639,
#68640,#68641,#68642,#68643,#68644,#68645,#68646,#68647,#68648,#68649,#68650,
#68651,#68652,#68653,#68654,#68655,#68656,#68657,#68658,#68659,#68660,#68661,
#68662,#68663,#68664,#68665,#68666,#68667,#68668,#68669,#68670,#68671,#68672,
#68673,#68674,#68675,#68676,#68677,#68678,#68679,#68680,#68681,#68682,#68683,
#68684,#68685,#68686,#68687,#68688,#68689,#68690,#68691,#68692,#68693,#68694,
#68695,#68696,#68697,#68698,#68699,#68700,#68701,#68702,#68703,#68704,#68705,
#68706,#68707,#68708,#68709,#68710,#68711,#68712,#68713,#68714,#68715,#68716,
#68717,#68718,#68719,#68720,#68721,#68722,#68723,#68724,#68725,#68726,#68727,
#68728,#68729,#68730,#68731,#68732,#68733,#68734,#68735,#68736,#68737,#68738,
#68739,#68740,#68741,#68742,#68743,#68744,#68745,#68746,#68747,#68748,#68749,
#68750,#68751,#68752,#68753,#68754,#68755,#68756,#68757,#68758,#68759,#68760,
#68761,#68762,#68763,#68764,#68765,#68766,#68767,#68768,#68769,#68770,#68771,
#68772,#68773,#68774,#68775,#68776,#68777,#68778,#68779,#68780,#68781,#68782,
#68783,#68784,#68785,#68786,#68787,#68788,#68789,#68790,#68791,#68792,#68793,
#68794,#68795,#68796,#68797,#68798,#68799,#68800,#68801,#68802,#68803,#68804,
#68805,#68806,#68807,#68808,#68809,#68810,#68811,#68812,#68813,#68814,#68815,
#68816,#68817,#68818,#68819,#68820,#68821,#68822,#68823,#68824,#68825,#68826,
#68827,#68828,#68829,#68830,#68831,#68832,#68833,#68834,#68835,#68836,#68837,
#68838,#68839,#68840,#68841,#68842,#68843,#68844,#68845,#68846,#68847,#68848,
#68849,#68850,#68851,#68852,#68853,#68854,#68855,#68856,#68857,#68858,#68859,
#68860,#68861,#68862,#68863,#68864,#68865,#68866,#68867,#68868,#68869,#68870,
#68871,#68872,#68873,#68874,#68875,#68876,#68877,#68878,#68879,#68880,#68881,
#68882,#68883,#68884,#68885,#68886,#68887),(#68888,#68889,#68890,#68891,
#68892,#68893,#68894,#68895,#68896,#68897,#68898,#68899,#68900,#68901,#68902,
#68903,#68904,#68905,#68906,#68907,#68908,#68909,#68910,#68911,#68912,#68913,
#68914,#68915,#68916,#68917,#68918,#68919,#68920,#68921,#68922,#68923,#68924,
#68925,#68926,#68927,#68928,#68929,#68930,#68931,#68932,#68933,#68934,#68935,
#68936,#68937,#68938,#68939,#68940,#68941,#68942,#68943,#68944,#68945,#68946,
#68947,#68948,#68949,#68950,#68951,#68952,#68953,#68954,#68955,#68956,#68957,
#68958,#68959,#68960,#68961,#68962,#68963,#68964,#68965,#68966,#68967,#68968,
#68969,#68970,#68971,#68972,#68973,#68974,#68975,#68976,#68977,#68978,#68979,
#68980,#68981,#68982,#68983,#68984,#68985,#68986,#68987,#68988,#68989,#68990,
#68991,#68992,#68993,#68994,#68995,#68996,#68997,#68998,#68999,#69000,#69001,
#69002,#69003,#69004,#69005,#69006,#69007,#69008,#69009,#69010,#69011,#69012,
#69013,#69014,#69015,#69016,#69017,#69018,#69019,#69020,#69021,#69022,#69023,
#69024,#69025,#69026,#69027,#69028,#69029,#69030,#69031,#69032,#69033,#69034,
#69035,#69036,#69037,#69038,#69039,#69040,#69041,#69042,#69043,#69044,#69045,
#69046,#69047,#69048,#69049,#69050,#69051,#69052,#69053,#69054,#69055,#69056,
#69057,#69058,#69059,#69060,#69061,#69062,#69063,#69064,#69065,#69066,#69067,
#69068,#69069,#69070,#69071,#69072,#69073,#69074,#69075,#69076,#69077,#69078,
#69079,#69080,#69081,#69082,#69083,#69084,#69085,#69086,#69087,#69088,#69089,
#69090,#69091,#69092,#69093,#69094,#69095,#69096,#69097,#69098,#69099,#69100,
#69101,#69102,#69103,#69104,#69105,#69106,#69107,#69108,#69109,#69110,#69111,
#69112,#69113,#69114,#69115,#69116,#69117,#69118,#69119,#69120,#69121,#69122,
#69123,#69124,#69125,#69126,#69127,#69128,#69129,#69130,#69131,#69132,#69133,
#69134,#69135,#69136,#69137,#69138,#69139,#69140,#69141,#69142,#69143,#69144,
#69145,#69146,#69147,#69148,#69149,#69150,#69151,#69152,#69153,#69154,#69155,
#69156,#69157,#69158,#69159,#69160,#69161,#69162,#69163,#69164,#69165,#69166,
#69167,#69168,#69169,#69170,#69171,#69172,#69173,#69174,#69175,#69176,#69177,
#69178,#69179,#69180,#69181,#69182,#69183,#69184,#69185,#69186,#69187,#69188,
#69189,#69190,#69191,#69192,#69193,#69194,#69195,#69196,#69197,#69198,#69199,
#69200,#69201,#69202,#69203,#69204,#69205,#69206,#69207,#69208,#69209,#69210,
#69211,#69212,#69213,#69214,#69215,#69216,#69217,#69218,#69219,#69220,#69221,
#69222,#69223,#69224,#69225,#69226,#69227,#69228,#69229,#69230,#69231,#69232,
#69233,#69234,#69235,#69236,#69237,#69238,#69239,#69240,#69241,#69242,#69243,
#69244,#69245,#69246,#69247,#69248,#69249,#69250,#69251,#69252,#69253,#69254,
#69255,#69256,#69257,#69258,#69259,#69260,#69261,#69262,#69263,#69264,#69265,
#69266,#69267,#69268,#69269,#69270,#69271,#69272,#69273,#69274,#69275,#69276,
#69277,#69278,#69279,#69280,#69281,#69282,#69283,#69284,#69285,#69286,#69287,
#69288,#69289,#69290,#69291,#69292,#69293,#69294,#69295,#69296,#69297,#69298,
#69299,#69300,#69301,#69302,#69303,#69304,#69305,#69306,#69307,#69308,#69309,
#69310,#69311,#69312,#69313,#69314,#69315,#69316,#69317,#69318,#69319,#69320,
#69321,#69322,#69323,#69324,#69325,#69326,#69327,#69328,#69329,#69330,#69331,
#69332,#69333,#69334,#69335,#69336,#69337,#69338,#69339,#69340,#69341,#69342,
#69343,#69344,#69345,#69346,#69347,#69348,#69349,#69350,#69351,#69352,#69353,
#69354,#69355,#69356,#69357,#69358,#69359,#69360,#69361,#69362,#69363,#69364,
#69365,#69366,#69367,#69368,#69369,#69370,#69371,#69372,#69373,#69374,#69375,
#69376,#69377,#69378,#69379,#69380,#69381,#69382,#69383,#69384,#69385,#69386,
#69387,#69388,#69389,#69390,#69391,#69392,#69393,#69394,#69395,#69396,#69397,
#69398,#69399,#69400,#69401,#69402,#69403,#69404,#69405,#69406,#69407,#69408,
#69409,#69410,#69411,#69412,#69413,#69414,#69415,#69416,#69417,#69418,#69419,
#69420,#69421,#69422,#69423,#69424,#69425),(#69426,#69427,#69428,#69429,
#69430,#69431,#69432,#69433,#69434,#69435,#69436,#69437,#69438,#69439,#69440,
#69441,#69442,#69443,#69444,#69445,#69446,#69447,#69448,#69449,#69450,#69451,
#69452,#69453,#69454,#69455,#69456,#69457,#69458,#69459,#69460,#69461,#69462,
#69463,#69464,#69465,#69466,#69467,#69468,#69469,#69470,#69471,#69472,#69473,
#69474,#69475,#69476,#69477,#69478,#69479,#69480,#69481,#69482,#69483,#69484,
#69485,#69486,#69487,#69488,#69489,#69490,#69491,#69492,#69493,#69494,#69495,
#69496,#69497,#69498,#69499,#69500,#69501,#69502,#69503,#69504,#69505,#69506,
#69507,#69508,#69509,#69510,#69511,#69512,#69513,#69514,#69515,#69516,#69517,
#69518,#69519,#69520,#69521,#69522,#69523,#69524,#69525,#69526,#69527,#69528,
#69529,#69530,#69531,#69532,#69533,#69534,#69535,#69536,#69537,#69538,#69539,
#69540,#69541,#69542,#69543,#69544,#69545,#69546,#69547,#69548,#69549,#69550,
#69551,#69552,#69553,#69554,#69555,#69556,#69557,#69558,#69559,#69560,#69561,
#69562,#69563,#69564,#69565,#69566,#69567,#69568,#69569,#69570,#69571,#69572,
#69573,#69574,#69575,#69576,#69577,#69578,#69579,#69580,#69581,#69582,#69583,
#69584,#69585,#69586,#69587,#69588,#69589,#69590,#69591,#69592,#69593,#69594,
#69595,#69596,#69597,#69598,#69599,#69600,#69601,#69602,#69603,#69604,#69605,
#69606,#69607,#69608,#69609,#69610,#69611,#69612,#69613,#69614,#69615,#69616,
#69617,#69618,#69619,#69620,#69621,#69622,#69623,#69624,#69625,#69626,#69627,
#69628,#69629,#69630,#69631,#69632,#69633,#69634,#69635,#69636,#69637,#69638,
#69639,#69640,#69641,#69642,#69643,#69644,#69645,#69646,#69647,#69648,#69649,
#69650,#69651,#69652,#69653,#69654,#69655,#69656,#69657,#69658,#69659,#69660,
#69661,#69662,#69663,#69664,#69665,#69666,#69667,#69668,#69669,#69670,#69671,
#69672,#69673,#69674,#69675,#69676,#69677,#69678,#69679,#69680,#69681,#69682,
#69683,#69684,#69685,#69686,#69687,#69688,#69689,#69690,#69691,#69692,#69693,
#69694,#69695,#69696,#69697,#69698,#69699,#69700,#69701,#69702,#69703,#69704,
#69705,#69706,#69707,#69708,#69709,#69710,#69711,#69712,#69713,#69714,#69715,
#69716,#69717,#69718,#69719,#69720,#69721,#69722,#69723,#69724,#69725,#69726,
#69727,#69728,#69729,#69730,#69731,#69732,#69733,#69734,#69735,#69736,#69737,
#69738,#69739,#69740,#69741,#69742,#69743,#69744,#69745,#69746,#69747,#69748,
#69749,#69750,#69751,#69752,#69753,#69754,#69755,#69756,#69757,#69758,#69759,
#69760,#69761,#69762,#69763,#69764,#69765,#69766,#69767,#69768,#69769,#69770,
#69771,#69772,#69773,#69774,#69775,#69776,#69777,#69778,#69779,#69780,#69781,
#69782,#69783,#69784,#69785,#69786,#69787,#69788,#69789,#69790,#69791,#69792,
#69793,#69794,#69795,#69796,#69797,#69798,#69799,#69800,#69801,#69802,#69803,
#69804,#69805,#69806,#69807,#69808,#69809,#69810,#69811,#69812,#69813,#69814,
#69815,#69816,#69817,#69818,#69819,#69820,#69821,#69822,#69823,#69824,#69825,
#69826,#69827,#69828,#69829,#69830,#69831,#69832,#69833,#69834,#69835,#69836,
#69837,#69838,#69839,#69840,#69841,#69842,#69843,#69844,#69845,#69846,#69847,
#69848,#69849,#69850,#69851,#69852,#69853,#69854,#69855,#69856,#69857,#69858,
#69859,#69860,#69861,#69862,#69863,#69864,#69865,#69866,#69867,#69868,#69869,
#69870,#69871,#69872,#69873,#69874,#69875,#69876,#69877,#69878,#69879,#69880,
#69881,#69882,#69883,#69884,#69885,#69886,#69887,#69888,#69889,#69890,#69891,
#69892,#69893,#69894,#69895,#69896,#69897,#69898,#69899,#69900,#69901,#69902,
#69903,#69904,#69905,#69906,#69907,#69908,#69909,#69910,#69911,#69912,#69913,
#69914,#69915,#69916,#69917,#69918,#69919,#69920,#69921,#69922,#69923,#69924,
#69925,#69926,#69927,#69928,#69929,#69930,#69931,#69932,#69933,#69934,#69935,
#69936,#69937,#69938,#69939,#69940,#69941,#69942,#69943,#69944,#69945,#69946,
#69947,#69948,#69949,#69950,#69951,#69952,#69953,#69954,#69955,#69956,#69957,
#69958,#69959,#69960,#69961,#69962,#69963),(#69964,#69965,#69966,#69967,
#69968,#69969,#69970,#69971,#69972,#69973,#69974,#69975,#69976,#69977,#69978,
#69979,#69980,#69981,#69982,#69983,#69984,#69985,#69986,#69987,#69988,#69989,
#69990,#69991,#69992,#69993,#69994,#69995,#69996,#69997,#69998,#69999,#70000,
#70001,#70002,#70003,#70004,#70005,#70006,#70007,#70008,#70009,#70010,#70011,
#70012,#70013,#70014,#70015,#70016,#70017,#70018,#70019,#70020,#70021,#70022,
#70023,#70024,#70025,#70026,#70027,#70028,#70029,#70030,#70031,#70032,#70033,
#70034,#70035,#70036,#70037,#70038,#70039,#70040,#70041,#70042,#70043,#70044,
#70045,#70046,#70047,#70048,#70049,#70050,#70051,#70052,#70053,#70054,#70055,
#70056,#70057,#70058,#70059,#70060,#70061,#70062,#70063,#70064,#70065,#70066,
#70067,#70068,#70069,#70070,#70071,#70072,#70073,#70074,#70075,#70076,#70077,
#70078,#70079,#70080,#70081,#70082,#70083,#70084,#70085,#70086,#70087,#70088,
#70089,#70090,#70091,#70092,#70093,#70094,#70095,#70096,#70097,#70098,#70099,
#70100,#70101,#70102,#70103,#70104,#70105,#70106,#70107,#70108,#70109,#70110,
#70111,#70112,#70113,#70114,#70115,#70116,#70117,#70118,#70119,#70120,#70121,
#70122,#70123,#70124,#70125,#70126,#70127,#70128,#70129,#70130,#70131,#70132,
#70133,#70134,#70135,#70136,#70137,#70138,#70139,#70140,#70141,#70142,#70143,
#70144,#70145,#70146,#70147,#70148,#70149,#70150,#70151,#70152,#70153,#70154,
#70155,#70156,#70157,#70158,#70159,#70160,#70161,#70162,#70163,#70164,#70165,
#70166,#70167,#70168,#70169,#70170,#70171,#70172,#70173,#70174,#70175,#70176,
#70177,#70178,#70179,#70180,#70181,#70182,#70183,#70184,#70185,#70186,#70187,
#70188,#70189,#70190,#70191,#70192,#70193,#70194,#70195,#70196,#70197,#70198,
#70199,#70200,#70201,#70202,#70203,#70204,#70205,#70206,#70207,#70208,#70209,
#70210,#70211,#70212,#70213,#70214,#70215,#70216,#70217,#70218,#70219,#70220,
#70221,#70222,#70223,#70224,#70225,#70226,#70227,#70228,#70229,#70230,#70231,
#70232,#70233,#70234,#70235,#70236,#70237,#70238,#70239,#70240,#70241,#70242,
#70243,#70244,#70245,#70246,#70247,#70248,#70249,#70250,#70251,#70252,#70253,
#70254,#70255,#70256,#70257,#70258,#70259,#70260,#70261,#70262,#70263,#70264,
#70265,#70266,#70267,#70268,#70269,#70270,#70271,#70272,#70273,#70274,#70275,
#70276,#70277,#70278,#70279,#70280,#70281,#70282,#70283,#70284,#70285,#70286,
#70287,#70288,#70289,#70290,#70291,#70292,#70293,#70294,#70295,#70296,#70297,
#70298,#70299,#70300,#70301,#70302,#70303,#70304,#70305,#70306,#70307,#70308,
#70309,#70310,#70311,#70312,#70313,#70314,#70315,#70316,#70317,#70318,#70319,
#70320,#70321,#70322,#70323,#70324,#70325,#70326,#70327,#70328,#70329,#70330,
#70331,#70332,#70333,#70334,#70335,#70336,#70337,#70338,#70339,#70340,#70341,
#70342,#70343,#70344,#70345,#70346,#70347,#70348,#70349,#70350,#70351,#70352,
#70353,#70354,#70355,#70356,#70357,#70358,#70359,#70360,#70361,#70362,#70363,
#70364,#70365,#70366,#70367,#70368,#70369,#70370,#70371,#70372,#70373,#70374,
#70375,#70376,#70377,#70378,#70379,#70380,#70381,#70382,#70383,#70384,#70385,
#70386,#70387,#70388,#70389,#70390,#70391,#70392,#70393,#70394,#70395,#70396,
#70397,#70398,#70399,#70400,#70401,#70402,#70403,#70404,#70405,#70406,#70407,
#70408,#70409,#70410,#70411,#70412,#70413,#70414,#70415,#70416,#70417,#70418,
#70419,#70420,#70421,#70422,#70423,#70424,#70425,#70426,#70427,#70428,#70429,
#70430,#70431,#70432,#70433,#70434,#70435,#70436,#70437,#70438,#70439,#70440,
#70441,#70442,#70443,#70444,#70445,#70446,#70447,#70448,#70449,#70450,#70451,
#70452,#70453,#70454,#70455,#70456,#70457,#70458,#70459,#70460,#70461,#70462,
#70463,#70464,#70465,#70466,#70467,#70468,#70469,#70470,#70471,#70472,#70473,
#70474,#70475,#70476,#70477,#70478,#70479,#70480,#70481,#70482,#70483,#70484,
#70485,#70486,#70487,#70488,#70489,#70490,#70491,#70492,#70493,#70494,#70495,
#70496,#70497,#70498,#70499,#70500,#70501)),.UNSPECIFIED.,.F.,.F.,.F.,(4,
4),(4,1,1,1,1,1,1,1,1,1,1,1,1,1,1,1,1,1,1,1,1,1,1,1,1,1,1,1,1,1,1,1,1,1,
1,1,1,1,1,1,1,1,1,1,1,1,1,1,1,1,1,1,1,1,1,1,1,1,1,1,1,1,1,1,1,1,1,1,1,1,
1,1,1,1,1,1,1,1,1,1,1,1,1,1,1,1,1,1,1,1,1,1,1,1,1,1,1,1,1,1,1,1,1,1,1,1,
1,1,1,1,1,1,1,1,1,1,1,1,1,1,1,1,1,1,1,1,1,1,1,1,1,1,1,1,1,1,1,1,1,1,1,1,
1,1,1,1,1,1,1,1,1,1,1,1,1,1,1,1,1,1,1,1,1,1,1,1,1,1,1,1,1,1,1,1,1,1,1,1,
1,1,1,1,1,1,1,1,1,1,1,1,1,1,1,1,1,1,1,1,1,1,1,1,1,1,1,1,1,1,1,1,1,1,1,1,
1,1,1,1,1,1,1,1,1,1,1,1,1,1,1,1,1,1,1,1,1,1,1,1,1,1,1,1,1,1,1,1,1,1,1,1,
1,1,1,1,1,1,1,1,1,1,1,1,1,1,1,1,1,1,1,1,1,1,1,1,1,1,1,1,1,1,1,1,1,1,1,1,
1,1,1,1,1,1,1,1,1,1,1,1,1,1,1,1,1,1,1,1,1,1,1,1,1,1,1,1,1,1,1,1,1,1,1,1,
1,1,1,1,1,1,1,1,1,1,1,1,1,1,1,1,1,1,1,1,1,1,1,1,1,1,1,1,1,1,1,1,1,1,1,1,
1,1,1,1,1,1,1,1,1,1,1,1,1,1,1,1,1,1,1,1,1,1,1,1,1,1,1,1,1,1,1,1,1,1,1,1,
1,1,1,1,1,1,1,1,1,1,1,1,1,1,1,1,1,1,1,1,1,1,1,1,1,1,1,1,1,1,1,1,1,1,1,1,
1,1,1,1,1,1,1,1,1,1,1,1,1,1,1,1,1,1,1,1,1,1,1,1,1,1,1,1,1,1,1,1,1,1,1,1,
1,1,1,1,1,1,1,1,1,1,1,1,1,1,1,1,1,1,1,1,1,1,1,1,1,1,1,1,1,1,1,1,1,1,1,1,
1,1,1,1,1,1,1,1,1,1,1,1,1,1,1,1,1,1,1,1,1,1,1,1,1,1,1,1,1,1,1,1,1,4),(0.,
0.132097741590587),(11.6150328478189,12.1141250590241,12.6132172702293,
13.1123094814345,13.6114016926397,14.60958611505,15.6077705374604,16.6059549598707,
17.1050471710759,17.6041393822811,18.1032315934863,18.6023238046915,19.6005082271018,
20.099600438307,20.5986926495122,21.5968770719225,22.5950614943329,23.5932459167433,
24.0923381279484,24.5914303391536,25.0905225503588,25.589614761564,26.5877991839743,
27.0868913951795,27.5859836063847,28.5841680287951,29.5823524512054,30.5805368736158,
31.079629084821,31.5787212960261,32.0778135072313,32.5769057184365,33.5750901408469,
34.074182352052,34.5732745632572,35.5714589856676,36.569643408078,37.5678278304883,
38.0669200416935,38.5660122528987,39.0651044641039,39.564196675309,40.5623810977194,
41.0614733089246,41.5605655201297,42.5587499425401,43.5569343649505,44.5551187873608,
45.054210998566,45.5533032097712,46.0523954209764,46.5514876321816,47.5496720545919,
48.0487642657971,48.5478564770023,49.5460408994126,50.544225321823,51.5424097442334,
52.0415019554385,52.5405941666437,53.0396863778489,53.5387785890541,54.5369630114644,
55.0360552226696,55.5351474338748,56.5333318562852,57.5315162786955,58.5297007011059,
59.0287929123111,59.5278851235162,60.0269773347214,60.5260695459266,61.524253968337,
62.0233461795421,62.5224383907473,63.5206228131577,64.518807235568,65.5169916579784,
66.0160838691836,66.5151760803888,67.0142682915939,67.5133605027991,68.5115449252095,
69.0106371364147,69.5097293476198,70.5079137700302,71.5060981924406,72.5042826148509,
73.0033748260561,73.5024670372613,74.0015592484665,74.5006514596716,75.498835882082,
75.9979280932872,76.4970203044924,77.4952047269027,78.4933891493131,79.4915735717234,
79.9906657829286,80.4897579941338,80.988850205339,81.4879424165442,82.4861268389545,
82.9852190501597,83.4843112613649,84.4824956837752,85.4806801061856,86.4788645285959,
86.9779567398011,87.4770489510063,87.9761411622115,88.4752333734167,89.473417795827,
89.9725100070322,90.4716022182374,91.4697866406478,92.4679710630581,93.4661554854685,
93.9652476966737,94.4643399078788,94.963432119084,95.4625243302892,96.4607087526996,
96.9598009639047,97.4588931751099,98.4570775975203,99.4552620199306,100.453446442341,
100.952538653546,101.451630864751,101.950723075957,102.449815287162,103.447999709572,
103.947091920777,104.446184131982,105.444368554393,106.442552976803,107.440737399214,
107.939829610419,108.438921821624,108.938014032829,109.437106244034,110.435290666445,
110.93438287765,111.433475088855,112.431659511265,113.429843933676,114.428028356086,
114.927120567291,115.426212778496,115.925304989702,116.424397200907,117.422581623317,
117.921673834522,118.420766045727,119.418950468138,120.417134890548,121.415319312959,
121.914411524164,122.413503735369,122.912595946574,123.411688157779,124.40987258019,
124.908964791395,125.4080570026,126.40624142501,127.404425847421,128.402610269831,
128.901702481036,129.400794692241,129.899886903447,130.398979114652,131.397163537062,
131.896255748267,132.395347959473,133.393532381883,134.391716804293,135.389901226704,
135.888993437909,136.388085649114,136.887177860319,137.386270071524,138.384454493935,
138.88354670514,139.382638916345,140.380823338755,141.379007761166,142.377192183576,
142.876284394781,143.375376605987,143.874468817192,144.373561028397,145.371745450807,
145.870837662012,146.369929873218,147.368114295628,148.366298718038,149.364483140449,
149.863575351654,150.362667562859,150.861759774064,151.360851985269,152.35903640768,
152.858128618885,153.35722083009,154.3554052525,155.353589674911,156.351774097321,
156.850866308526,157.349958519732,157.849050730937,158.348142942142,159.346327364552,
159.845419575757,160.344511786963,161.342696209373,162.340880631783,163.339065054194,
163.838157265399,164.337249476604,164.836341687809,165.335433899014,166.333618321425,
166.83271053263,167.331802743835,168.329987166246,169.328171588656,170.326356011066,
170.825448222271,171.324540433477,171.823632644682,172.322724855887,173.320909278297,
173.820001489502,174.319093700708,175.317278123118,176.315462545528,177.313646967939,
177.812739179144,178.311831390349,178.810923601554,179.310015812759,180.30820023517,
180.807292446375,181.30638465758,182.304569079991,183.302753502401,184.300937924811,
184.800030136016,185.299122347222,185.798214558427,186.297306769632,187.295491192042,
187.794583403248,188.293675614453,189.291860036863,190.290044459273,191.288228881684,
191.787321092889,192.286413304094,192.785505515299,193.284597726505,194.282782148915,
194.78187436012,195.280966571325,196.279150993736,197.277335416146,198.275519838556,
199.273704260967,200.271888683377,201.270073105787,202.268257528198,202.767349739403,
203.266441950608,204.264626373018,204.763718584224,205.262810795429,205.761903006634,
206.260995217839,207.25917964025,208.25736406266,209.25554848507,209.754640696275,
210.253732907481,211.251917329891,211.751009541096,212.250101752301,212.749193963507,
213.248286174712,214.246470597122,215.244655019532,216.242839441943,216.741931653148,
217.241023864353,218.239208286764,218.738300497969,219.237392709174,219.736484920379,
220.235577131584,221.233761553995,222.231945976405,223.230130398815,223.72922261002,
224.228314821226,225.226499243636,225.725591454841,226.224683666046,226.723775877252,
227.222868088457,228.221052510867,229.219236933277,230.217421355688,230.716513566893,
231.215605778098,232.213790200509,232.712882411714,233.211974622919,233.711066834124,
234.210159045329,235.20834346774,236.20652789015,237.20471231256,237.703804523766,
238.202896734971,239.201081157381,239.700173368586,240.199265579791,240.698357790997,
241.197450002202,242.195634424612,243.193818847023,244.192003269433,244.691095480638,
245.190187691843,246.188372114254,246.687464325459,247.186556536664,247.685648747869,
248.184740959074,249.182925381485,250.181109803895,251.179294226305,251.678386437511,
252.177478648716,253.175663071126,253.674755282331,254.173847493536,254.672939704742,
255.172031915947,256.170216338357,257.168400760768,258.166585183178,258.665677394383,
259.164769605588,260.162954027999,260.662046239204,261.161138450409,261.660230661614,
262.159322872819,263.15750729523,264.15569171764,265.15387614005,265.652968351256,
266.152060562461,267.150244984871,267.649337196076,268.148429407282,268.647521618487,
269.146613829692,270.144798252102,271.142982674513,272.141167096923,272.640259308128,
273.139351519333,274.137535941744,274.636628152949,275.135720364154,275.634812575359,
276.133904786564,277.132089208975,278.130273631385,279.128458053795,279.627550265001,
280.126642476206,281.124826898616,281.623919109821,282.123011321027,282.622103532232,
283.121195743437,284.119380165847,285.117564588258,286.115749010668,286.614841221873,
287.113933433078,288.112117855489,288.611210066694,289.110302277899,289.609394489104,
290.108486700309,291.10667112272,292.10485554513,293.103039967541,293.602132178746,
294.101224389951,295.099408812361,295.598501023566,296.097593234772,296.596685445977,
297.095777657182,298.093962079592,299.092146502003,300.090330924413,300.589423135618,
301.088515346823,302.086699769234,302.585791980439,303.084884191644,303.583976402849,
304.083068614054,305.081253036465,306.079437458875,307.077621881286,307.576714092491,
308.075806303696,309.073990726106,309.573082937311,310.072175148517,310.571267359722,
311.070359570927,312.068543993337,313.066728415748,314.064912838158,314.564005049363,
315.063097260568,316.061281682979,316.560373894184,317.059466105389,317.558558316594,
318.0576505278,319.05583495021,320.05401937262,321.052203795031,321.551296006236,
322.050388217441,323.048572639851,323.547664851057,324.046757062262,324.545849273467,
325.044941484672,326.043125907082,327.041310329493,328.039494751903,328.538586963108,
329.037679174313,330.035863596724,330.534955807929,331.034048019134,331.533140230339,
332.032232441545,333.030416863955,334.028601286365,335.026785708776,335.525877919981,
336.024970131186,337.023154553596,337.522246764802,338.021338976007,338.520431187212,
339.019523398417,340.017707820827,341.015892243238,342.014076665648,342.513168876853,
343.012261088059,344.010445510469,344.509537721674,345.008629932879,345.507722144084,
346.00681435529,347.0049987777,348.00318320011,349.001367622521,349.500459833726,
349.999552044931,350.997736467341,351.496828678547,351.995920889752,352.495013100957,
352.994105312162,353.992289734573,354.990474156983,355.988658579393,356.487750790598,
356.986843001804,357.985027424214,358.484119635419,358.983211846624,359.48230405783,
359.981396269035,360.979580691445,361.977765113855,362.975949536266,363.475041747471,
363.974133958676,364.972318381086,365.471410592292,365.970502803497,366.469595014702,
366.968687225907,367.966871648318,368.965056070728,369.963240493138,370.462332704343,
370.961424915549,371.959609337959,372.458701549164,372.957793760369,373.456885971574,
373.95597818278,374.95416260519,375.9523470276,376.950531450011,377.449623661216,
377.948715872421,378.946900294831,379.445992506037,379.945084717242,380.444176928447,
380.943269139652,381.941453562063,382.939637984473,383.937822406883,384.436914618089,
384.936006829294,385.435099040499,385.934191251704),.UNSPECIFIED.);
#1532=CYLINDRICAL_SURFACE('',#28711,0.875);
#1533=CYLINDRICAL_SURFACE('',#28715,0.875);
#1534=CYLINDRICAL_SURFACE('',#28719,0.875);
#1535=CYLINDRICAL_SURFACE('',#28723,0.875);
#1536=CYLINDRICAL_SURFACE('',#28741,0.875);
#1537=CYLINDRICAL_SURFACE('',#28745,0.875);
#1538=CYLINDRICAL_SURFACE('',#28749,0.875);
#1539=CYLINDRICAL_SURFACE('',#28753,0.875);
#1540=CYLINDRICAL_SURFACE('',#28759,0.8);
#1541=CYLINDRICAL_SURFACE('',#28762,1.8);
#1542=CYLINDRICAL_SURFACE('',#28789,0.8);
#1543=CYLINDRICAL_SURFACE('',#28792,0.8);
#1544=CYLINDRICAL_SURFACE('',#28825,1.8);
#1545=CYLINDRICAL_SURFACE('',#28831,1.8);
#1546=CYLINDRICAL_SURFACE('',#28846,0.4);
#1547=CYLINDRICAL_SURFACE('',#28849,0.4);
#1548=CYLINDRICAL_SURFACE('',#28867,0.4);
#1549=CYLINDRICAL_SURFACE('',#28869,0.4);
#1550=CYLINDRICAL_SURFACE('',#28875,1.8);
#1551=CYLINDRICAL_SURFACE('',#28895,0.8);
#1552=CYLINDRICAL_SURFACE('',#28898,0.8);
#1553=CYLINDRICAL_SURFACE('',#28920,0.8);
#1554=CYLINDRICAL_SURFACE('',#28934,1.8);
#1555=CYLINDRICAL_SURFACE('',#28949,0.4);
#1556=CYLINDRICAL_SURFACE('',#28952,0.4);
#1557=CYLINDRICAL_SURFACE('',#28969,0.4);
#1558=CYLINDRICAL_SURFACE('',#28971,0.4);
#1559=CYLINDRICAL_SURFACE('',#28976,1.8);
#1560=CYLINDRICAL_SURFACE('',#28983,1.8);
#1561=CYLINDRICAL_SURFACE('',#28990,1.8);
#1562=CYLINDRICAL_SURFACE('',#28997,0.504999999999999);
#1563=CYLINDRICAL_SURFACE('',#29007,0.504999999999999);
#1564=CYLINDRICAL_SURFACE('',#29042,0.8);
#1565=CYLINDRICAL_SURFACE('',#29044,0.8);
#1566=CYLINDRICAL_SURFACE('',#29155,2.5);
#1567=CYLINDRICAL_SURFACE('',#29162,0.504999999999999);
#1568=CYLINDRICAL_SURFACE('',#29170,0.504999999999999);
#1569=CYLINDRICAL_SURFACE('',#29276,0.7);
#1570=CYLINDRICAL_SURFACE('',#29284,0.699999999999999);
#1571=CYLINDRICAL_SURFACE('',#29291,0.699999999999999);
#1572=CYLINDRICAL_SURFACE('',#29299,0.7);
#1573=CYLINDRICAL_SURFACE('',#29328,0.875);
#1574=CYLINDRICAL_SURFACE('',#29333,0.875);
#1575=CYLINDRICAL_SURFACE('',#29374,0.2);
#1576=CYLINDRICAL_SURFACE('',#29392,1.);
#1577=CYLINDRICAL_SURFACE('',#29395,1.);
#1578=CYLINDRICAL_SURFACE('',#29445,0.5);
#1579=CYLINDRICAL_SURFACE('',#29447,0.5);
#1580=CYLINDRICAL_SURFACE('',#29456,1.);
#1581=CYLINDRICAL_SURFACE('',#29459,0.41);
#1582=CYLINDRICAL_SURFACE('',#29463,0.405000000000001);
#1583=CYLINDRICAL_SURFACE('',#29467,0.5);
#1584=CYLINDRICAL_SURFACE('',#29468,0.5);
#1585=CYLINDRICAL_SURFACE('',#29470,0.5);
#1586=CYLINDRICAL_SURFACE('',#29488,1.8);
#1587=CYLINDRICAL_SURFACE('',#29492,2.655);
#1588=CYLINDRICAL_SURFACE('',#29505,5.);
#1589=CYLINDRICAL_SURFACE('',#29511,5.4);
#1590=CYLINDRICAL_SURFACE('',#29528,1.);
#1591=CYLINDRICAL_SURFACE('',#29533,1.);
#1592=CYLINDRICAL_SURFACE('',#29536,1.486725);
#1593=CYLINDRICAL_SURFACE('',#29538,1.486725);
#1594=CYLINDRICAL_SURFACE('',#29539,1.486725);
#1595=CYLINDRICAL_SURFACE('',#29540,1.486725);
#1596=CYLINDRICAL_SURFACE('',#29541,1.486725);
#1597=CYLINDRICAL_SURFACE('',#29543,1.2866);
#1598=CYLINDRICAL_SURFACE('',#29545,1.2866);
#1599=CYLINDRICAL_SURFACE('',#29546,1.2866);
#1600=CYLINDRICAL_SURFACE('',#29547,1.2866);
#1601=CYLINDRICAL_SURFACE('',#29671,2.25);
#1602=CYLINDRICAL_SURFACE('',#29673,2.25);
#1603=CYLINDRICAL_SURFACE('',#29675,2.25);
#1604=CYLINDRICAL_SURFACE('',#29677,2.25);
#1605=CYLINDRICAL_SURFACE('',#29679,2.25);
#1606=CYLINDRICAL_SURFACE('',#29681,2.25);
#1607=CYLINDRICAL_SURFACE('',#29683,2.25);
#1608=CYLINDRICAL_SURFACE('',#29685,2.25);
#1609=CYLINDRICAL_SURFACE('',#29687,2.25);
#1610=CYLINDRICAL_SURFACE('',#29689,2.25);
#1611=CYLINDRICAL_SURFACE('',#29691,2.25);
#1612=CYLINDRICAL_SURFACE('',#29693,2.25);
#1613=CYLINDRICAL_SURFACE('',#29695,2.25);
#1614=CYLINDRICAL_SURFACE('',#29697,2.25);
#1615=CYLINDRICAL_SURFACE('',#29699,2.25);
#1616=CYLINDRICAL_SURFACE('',#29701,2.25);
#1617=CYLINDRICAL_SURFACE('',#29703,2.25);
#1618=CYLINDRICAL_SURFACE('',#29705,2.25);
#1619=CYLINDRICAL_SURFACE('',#29707,2.25);
#1620=CYLINDRICAL_SURFACE('',#29709,2.25);
#1621=CYLINDRICAL_SURFACE('',#29711,2.25);
#1622=CYLINDRICAL_SURFACE('',#29713,2.25);
#1623=CYLINDRICAL_SURFACE('',#29715,2.25);
#1624=CYLINDRICAL_SURFACE('',#29717,1.2866);
#1625=CYLINDRICAL_SURFACE('',#29719,1.486725);
#1626=CYLINDRICAL_SURFACE('',#29725,2.65);
#1627=CYLINDRICAL_SURFACE('',#29734,2.25);
#1628=CYLINDRICAL_SURFACE('',#29737,0.3933);
#1629=CYLINDRICAL_SURFACE('',#29739,0.3933);
#1630=CYLINDRICAL_SURFACE('',#29740,0.3933);
#1631=CYLINDRICAL_SURFACE('',#29741,0.3933);
#1632=CYLINDRICAL_SURFACE('',#29742,0.3933);
#1633=CYLINDRICAL_SURFACE('',#29743,0.3933);
#1634=CYLINDRICAL_SURFACE('',#29744,0.3933);
#1635=CYLINDRICAL_SURFACE('',#29745,0.3933);
#1636=CYLINDRICAL_SURFACE('',#29746,0.3933);
#1637=CYLINDRICAL_SURFACE('',#29747,0.3933);
#1638=CYLINDRICAL_SURFACE('',#29748,0.3933);
#1639=CYLINDRICAL_SURFACE('',#29749,0.3933);
#1640=CYLINDRICAL_SURFACE('',#29750,0.3933);
#1641=CYLINDRICAL_SURFACE('',#29751,0.3933);
#1642=CYLINDRICAL_SURFACE('',#29752,0.3933);
#1643=CYLINDRICAL_SURFACE('',#29753,0.322275);
#1644=CYLINDRICAL_SURFACE('',#29755,0.322275);
#1645=CYLINDRICAL_SURFACE('',#29756,0.322275);
#1646=CYLINDRICAL_SURFACE('',#29757,0.322275);
#1647=CYLINDRICAL_SURFACE('',#29758,0.322275);
#1648=CYLINDRICAL_SURFACE('',#29759,0.322275);
#1649=CYLINDRICAL_SURFACE('',#29760,0.322275);
#1650=CYLINDRICAL_SURFACE('',#29761,0.322275);
#1651=CYLINDRICAL_SURFACE('',#29762,0.322275);
#1652=CYLINDRICAL_SURFACE('',#29763,0.322275);
#1653=CYLINDRICAL_SURFACE('',#29764,0.322275);
#1654=CYLINDRICAL_SURFACE('',#29765,0.322275);
#1655=CYLINDRICAL_SURFACE('',#29766,0.322275);
#1656=CYLINDRICAL_SURFACE('',#29767,0.322275);
#1657=CYLINDRICAL_SURFACE('',#29768,0.322275);
#1658=CYLINDRICAL_SURFACE('',#29842,1.1);
#1659=CYLINDRICAL_SURFACE('',#29866,0.322275);
#1660=CYLINDRICAL_SURFACE('',#29870,0.3933);
#1661=CYLINDRICAL_SURFACE('',#29879,0.4);
#1662=CYLINDRICAL_SURFACE('',#29897,0.6);
#1663=CYLINDRICAL_SURFACE('',#29898,0.300000000000001);
#1664=CYLINDRICAL_SURFACE('',#29904,0.300000000000001);
#1665=CYLINDRICAL_SURFACE('',#29967,2.9);
#1666=CYLINDRICAL_SURFACE('',#29973,3.15);
#1667=CYLINDRICAL_SURFACE('',#29977,3.3);
#1668=CYLINDRICAL_SURFACE('',#29983,0.25);
#1669=CYLINDRICAL_SURFACE('',#29984,1.25);
#1670=CYLINDRICAL_SURFACE('',#29990,0.599999999999994);
#1671=CYLINDRICAL_SURFACE('',#30000,1.7);
#1672=CYLINDRICAL_SURFACE('',#30065,1.5);
#1673=CYLINDRICAL_SURFACE('',#30068,1.5);
#1674=CYLINDRICAL_SURFACE('',#30093,0.875);
#1675=CYLINDRICAL_SURFACE('',#30100,0.875);
#1676=CYLINDRICAL_SURFACE('',#30108,0.875);
#1677=CYLINDRICAL_SURFACE('',#30113,0.875);
#1678=CYLINDRICAL_SURFACE('',#30118,0.899999999999999);
#1679=CYLINDRICAL_SURFACE('',#30122,0.899999999999999);
#1680=CYLINDRICAL_SURFACE('',#30161,1.5);
#1681=CYLINDRICAL_SURFACE('',#30163,1.5);
#1682=CYLINDRICAL_SURFACE('',#30170,0.199999999999999);
#1683=CYLINDRICAL_SURFACE('',#30183,0.199999999999999);
#1684=CYLINDRICAL_SURFACE('',#30185,0.4925);
#1685=CYLINDRICAL_SURFACE('',#30187,0.4925);
#1686=CYLINDRICAL_SURFACE('',#30188,0.4925);
#1687=CYLINDRICAL_SURFACE('',#30189,0.4925);
#1688=CYLINDRICAL_SURFACE('',#30190,0.4925);
#1689=CYLINDRICAL_SURFACE('',#30191,0.4925);
#1690=CYLINDRICAL_SURFACE('',#30192,0.4925);
#1691=CYLINDRICAL_SURFACE('',#30193,0.4925);
#1692=CYLINDRICAL_SURFACE('',#30194,0.4925);
#1693=CYLINDRICAL_SURFACE('',#30195,0.4925);
#1694=CYLINDRICAL_SURFACE('',#30196,0.4925);
#1695=CYLINDRICAL_SURFACE('',#30197,0.40705);
#1696=CYLINDRICAL_SURFACE('',#30199,0.40705);
#1697=CYLINDRICAL_SURFACE('',#30200,0.40705);
#1698=CYLINDRICAL_SURFACE('',#30201,0.40705);
#1699=CYLINDRICAL_SURFACE('',#30202,0.40705);
#1700=CYLINDRICAL_SURFACE('',#30203,0.40705);
#1701=CYLINDRICAL_SURFACE('',#30204,0.40705);
#1702=CYLINDRICAL_SURFACE('',#30205,0.40705);
#1703=CYLINDRICAL_SURFACE('',#30206,0.40705);
#1704=CYLINDRICAL_SURFACE('',#30207,0.40705);
#1705=CYLINDRICAL_SURFACE('',#30208,0.40705);
#1706=CYLINDRICAL_SURFACE('',#30226,1.25);
#1707=CYLINDRICAL_SURFACE('',#30229,0.40705);
#1708=CYLINDRICAL_SURFACE('',#30237,0.4925);
#1709=CYLINDRICAL_SURFACE('',#30285,0.7911);
#1710=CYLINDRICAL_SURFACE('',#30287,0.7911);
#1711=CYLINDRICAL_SURFACE('',#30288,0.7911);
#1712=CYLINDRICAL_SURFACE('',#30289,0.7911);
#1713=CYLINDRICAL_SURFACE('',#30290,0.7911);
#1714=CYLINDRICAL_SURFACE('',#30291,0.7911);
#1715=CYLINDRICAL_SURFACE('',#30292,0.7911);
#1716=CYLINDRICAL_SURFACE('',#30293,0.7911);
#1717=CYLINDRICAL_SURFACE('',#30294,0.7911);
#1718=CYLINDRICAL_SURFACE('',#30295,0.7911);
#1719=CYLINDRICAL_SURFACE('',#30296,0.7911);
#1720=CYLINDRICAL_SURFACE('',#30297,0.7911);
#1721=CYLINDRICAL_SURFACE('',#30298,0.7911);
#1722=CYLINDRICAL_SURFACE('',#30299,0.7911);
#1723=CYLINDRICAL_SURFACE('',#30300,0.7911);
#1724=CYLINDRICAL_SURFACE('',#30301,0.7911);
#1725=CYLINDRICAL_SURFACE('',#30302,0.7911);
#1726=CYLINDRICAL_SURFACE('',#30303,0.7911);
#1727=CYLINDRICAL_SURFACE('',#30304,0.7911);
#1728=CYLINDRICAL_SURFACE('',#30305,0.7911);
#1729=CYLINDRICAL_SURFACE('',#30306,0.7911);
#1730=CYLINDRICAL_SURFACE('',#30307,0.7911);
#1731=CYLINDRICAL_SURFACE('',#30308,0.7911);
#1732=CYLINDRICAL_SURFACE('',#30309,0.7911);
#1733=CYLINDRICAL_SURFACE('',#30310,0.7911);
#1734=CYLINDRICAL_SURFACE('',#30311,0.7911);
#1735=CYLINDRICAL_SURFACE('',#30312,0.7911);
#1736=CYLINDRICAL_SURFACE('',#30313,0.7911);
#1737=CYLINDRICAL_SURFACE('',#30314,0.7911);
#1738=CYLINDRICAL_SURFACE('',#30315,0.7911);
#1739=CYLINDRICAL_SURFACE('',#30316,0.7911);
#1740=CYLINDRICAL_SURFACE('',#30317,0.7911);
#1741=CYLINDRICAL_SURFACE('',#30318,0.7911);
#1742=CYLINDRICAL_SURFACE('',#30319,0.7911);
#1743=CYLINDRICAL_SURFACE('',#30320,0.7911);
#1744=CYLINDRICAL_SURFACE('',#30321,0.7911);
#1745=CYLINDRICAL_SURFACE('',#30322,0.7911);
#1746=CYLINDRICAL_SURFACE('',#30323,0.7911);
#1747=CYLINDRICAL_SURFACE('',#30324,0.7911);
#1748=CYLINDRICAL_SURFACE('',#30325,0.7911);
#1749=CYLINDRICAL_SURFACE('',#30326,0.7911);
#1750=CYLINDRICAL_SURFACE('',#30327,0.7911);
#1751=CYLINDRICAL_SURFACE('',#30328,0.7911);
#1752=CYLINDRICAL_SURFACE('',#30329,0.7911);
#1753=CYLINDRICAL_SURFACE('',#30330,0.7911);
#1754=CYLINDRICAL_SURFACE('',#30331,0.7911);
#1755=CYLINDRICAL_SURFACE('',#30332,0.7911);
#1756=CYLINDRICAL_SURFACE('',#30333,0.7911);
#1757=CYLINDRICAL_SURFACE('',#30334,0.7911);
#1758=CYLINDRICAL_SURFACE('',#30335,0.7911);
#1759=CYLINDRICAL_SURFACE('',#30336,0.7911);
#1760=CYLINDRICAL_SURFACE('',#30337,0.7911);
#1761=CYLINDRICAL_SURFACE('',#30338,0.7911);
#1762=CYLINDRICAL_SURFACE('',#30339,0.7911);
#1763=CYLINDRICAL_SURFACE('',#30340,0.7911);
#1764=CYLINDRICAL_SURFACE('',#30341,0.7911);
#1765=CYLINDRICAL_SURFACE('',#30342,0.7911);
#1766=CYLINDRICAL_SURFACE('',#30343,0.7911);
#1767=CYLINDRICAL_SURFACE('',#30344,0.7911);
#1768=CYLINDRICAL_SURFACE('',#30345,0.7911);
#1769=CYLINDRICAL_SURFACE('',#30347,0.6767);
#1770=CYLINDRICAL_SURFACE('',#30349,0.6767);
#1771=CYLINDRICAL_SURFACE('',#30350,0.6767);
#1772=CYLINDRICAL_SURFACE('',#30351,0.6767);
#1773=CYLINDRICAL_SURFACE('',#30352,0.6767);
#1774=CYLINDRICAL_SURFACE('',#30353,0.6767);
#1775=CYLINDRICAL_SURFACE('',#30354,0.6767);
#1776=CYLINDRICAL_SURFACE('',#30355,0.6767);
#1777=CYLINDRICAL_SURFACE('',#30356,0.6767);
#1778=CYLINDRICAL_SURFACE('',#30357,0.6767);
#1779=CYLINDRICAL_SURFACE('',#30358,0.6767);
#1780=CYLINDRICAL_SURFACE('',#30359,0.6767);
#1781=CYLINDRICAL_SURFACE('',#30360,0.6767);
#1782=CYLINDRICAL_SURFACE('',#30361,0.6767);
#1783=CYLINDRICAL_SURFACE('',#30362,0.6767);
#1784=CYLINDRICAL_SURFACE('',#30363,0.6767);
#1785=CYLINDRICAL_SURFACE('',#30364,0.6767);
#1786=CYLINDRICAL_SURFACE('',#30365,0.6767);
#1787=CYLINDRICAL_SURFACE('',#30366,0.6767);
#1788=CYLINDRICAL_SURFACE('',#30367,0.6767);
#1789=CYLINDRICAL_SURFACE('',#30368,0.6767);
#1790=CYLINDRICAL_SURFACE('',#30369,0.6767);
#1791=CYLINDRICAL_SURFACE('',#30370,0.6767);
#1792=CYLINDRICAL_SURFACE('',#30371,0.6767);
#1793=CYLINDRICAL_SURFACE('',#30372,0.6767);
#1794=CYLINDRICAL_SURFACE('',#30373,0.6767);
#1795=CYLINDRICAL_SURFACE('',#30374,0.6767);
#1796=CYLINDRICAL_SURFACE('',#30375,0.6767);
#1797=CYLINDRICAL_SURFACE('',#30376,0.6767);
#1798=CYLINDRICAL_SURFACE('',#30377,0.6767);
#1799=CYLINDRICAL_SURFACE('',#30378,0.6767);
#1800=CYLINDRICAL_SURFACE('',#30379,0.6767);
#1801=CYLINDRICAL_SURFACE('',#30380,0.6767);
#1802=CYLINDRICAL_SURFACE('',#30381,0.6767);
#1803=CYLINDRICAL_SURFACE('',#30382,0.6767);
#1804=CYLINDRICAL_SURFACE('',#30383,0.6767);
#1805=CYLINDRICAL_SURFACE('',#30384,0.6767);
#1806=CYLINDRICAL_SURFACE('',#30385,0.6767);
#1807=CYLINDRICAL_SURFACE('',#30386,0.6767);
#1808=CYLINDRICAL_SURFACE('',#30387,0.6767);
#1809=CYLINDRICAL_SURFACE('',#30388,0.6767);
#1810=CYLINDRICAL_SURFACE('',#30389,0.6767);
#1811=CYLINDRICAL_SURFACE('',#30390,0.6767);
#1812=CYLINDRICAL_SURFACE('',#30391,0.6767);
#1813=CYLINDRICAL_SURFACE('',#30392,0.6767);
#1814=CYLINDRICAL_SURFACE('',#30393,0.6767);
#1815=CYLINDRICAL_SURFACE('',#30394,0.6767);
#1816=CYLINDRICAL_SURFACE('',#30395,0.6767);
#1817=CYLINDRICAL_SURFACE('',#30396,0.6767);
#1818=CYLINDRICAL_SURFACE('',#30397,0.6767);
#1819=CYLINDRICAL_SURFACE('',#30398,0.6767);
#1820=CYLINDRICAL_SURFACE('',#30399,0.6767);
#1821=CYLINDRICAL_SURFACE('',#30400,0.6767);
#1822=CYLINDRICAL_SURFACE('',#30401,0.6767);
#1823=CYLINDRICAL_SURFACE('',#30402,0.6767);
#1824=CYLINDRICAL_SURFACE('',#30403,0.6767);
#1825=CYLINDRICAL_SURFACE('',#30404,0.6767);
#1826=CYLINDRICAL_SURFACE('',#30405,0.6767);
#1827=CYLINDRICAL_SURFACE('',#30406,0.6767);
#1828=CYLINDRICAL_SURFACE('',#30425,0.6767);
#1829=CYLINDRICAL_SURFACE('',#30431,0.7911);
#1830=CYLINDRICAL_SURFACE('',#30448,0.805);
#1831=CYLINDRICAL_SURFACE('',#30465,0.85);
#1832=CYLINDRICAL_SURFACE('',#30470,1.5);
#1833=CYLINDRICAL_SURFACE('',#30489,1.40000000000001);
#1834=CYLINDRICAL_SURFACE('',#30494,0.52);
#1835=CYLINDRICAL_SURFACE('',#30506,1.40000000000001);
#1836=CYLINDRICAL_SURFACE('',#30512,1.30000000000003);
#1837=CYLINDRICAL_SURFACE('',#30516,1.40000000000001);
#1838=CYLINDRICAL_SURFACE('',#30520,1.3);
#1839=CYLINDRICAL_SURFACE('',#30524,1.40000000000001);
#1840=CYLINDRICAL_SURFACE('',#30528,1.30000000000003);
#1841=CYLINDRICAL_SURFACE('',#30535,1.60000000000001);
#1842=CYLINDRICAL_SURFACE('',#30541,0.999999999999985);
#1843=CYLINDRICAL_SURFACE('',#30548,1.19999999999999);
#1844=CYLINDRICAL_SURFACE('',#30568,0.875);
#1845=CYLINDRICAL_SURFACE('',#30572,0.875);
#1846=CYLINDRICAL_SURFACE('',#30576,0.875);
#1847=CYLINDRICAL_SURFACE('',#30580,0.875);
#1848=CYLINDRICAL_SURFACE('',#30584,0.875);
#1849=CYLINDRICAL_SURFACE('',#30588,1.3);
#1850=CYLINDRICAL_SURFACE('',#30592,1.3);
#1851=CYLINDRICAL_SURFACE('',#30608,0.875);
#1852=CYLINDRICAL_SURFACE('',#30612,0.875);
#1853=CYLINDRICAL_SURFACE('',#30616,0.875);
#1854=CYLINDRICAL_SURFACE('',#30620,0.875);
#1855=CYLINDRICAL_SURFACE('',#30624,0.875);
#1856=CYLINDRICAL_SURFACE('',#30642,0.3);
#1857=CYLINDRICAL_SURFACE('',#30645,0.3);
#1858=CYLINDRICAL_SURFACE('',#30654,1.3);
#1859=CYLINDRICAL_SURFACE('',#30658,1.3);
#1860=CYLINDRICAL_SURFACE('',#30662,1.3);
#1861=CYLINDRICAL_SURFACE('',#30666,1.3);
#1862=CYLINDRICAL_SURFACE('',#30670,1.3);
#1863=CYLINDRICAL_SURFACE('',#30674,1.3);
#1864=CYLINDRICAL_SURFACE('',#30678,1.3);
#1865=CYLINDRICAL_SURFACE('',#30682,1.3);
#1866=CYLINDRICAL_SURFACE('',#30686,1.3);
#1867=CYLINDRICAL_SURFACE('',#30707,1.3);
#1868=CYLINDRICAL_SURFACE('',#30738,0.8);
#1869=CYLINDRICAL_SURFACE('',#30741,0.8);
#1870=CYLINDRICAL_SURFACE('',#30769,0.8);
#1871=CYLINDRICAL_SURFACE('',#30785,0.3);
#1872=CYLINDRICAL_SURFACE('',#30786,0.3);
#1873=CYLINDRICAL_SURFACE('',#30789,0.8);
#1874=FACE_BOUND('',#4567,.T.);
#1875=FACE_BOUND('',#4568,.T.);
#1876=FACE_BOUND('',#4569,.T.);
#1877=FACE_BOUND('',#4570,.T.);
#1878=FACE_BOUND('',#4580,.T.);
#1879=FACE_BOUND('',#4581,.T.);
#1880=FACE_BOUND('',#4582,.T.);
#1881=FACE_BOUND('',#4583,.T.);
#1882=FACE_BOUND('',#4589,.T.);
#1883=FACE_BOUND('',#4590,.T.);
#1884=FACE_BOUND('',#4591,.T.);
#1885=FACE_BOUND('',#4592,.T.);
#1886=FACE_BOUND('',#4608,.T.);
#1887=FACE_BOUND('',#4609,.T.);
#1888=FACE_BOUND('',#4610,.T.);
#1889=FACE_BOUND('',#4611,.T.);
#1890=FACE_BOUND('',#4627,.T.);
#1891=FACE_BOUND('',#4638,.T.);
#1892=FACE_BOUND('',#4639,.T.);
#1893=FACE_BOUND('',#4640,.T.);
#1894=FACE_BOUND('',#4641,.T.);
#1895=FACE_BOUND('',#4642,.T.);
#1896=FACE_BOUND('',#4644,.T.);
#1897=FACE_BOUND('',#4711,.T.);
#1898=FACE_BOUND('',#4724,.T.);
#1899=FACE_BOUND('',#4787,.T.);
#1900=FACE_BOUND('',#4788,.T.);
#1901=FACE_BOUND('',#4791,.T.);
#1902=FACE_BOUND('',#4792,.T.);
#1903=FACE_BOUND('',#4815,.T.);
#1904=FACE_BOUND('',#4848,.T.);
#1905=FACE_BOUND('',#4962,.T.);
#1906=FACE_BOUND('',#4963,.T.);
#1907=FACE_BOUND('',#5001,.T.);
#1908=FACE_BOUND('',#5002,.T.);
#1909=FACE_BOUND('',#5010,.T.);
#1910=FACE_BOUND('',#5064,.T.);
#1911=FACE_BOUND('',#5070,.T.);
#1912=FACE_BOUND('',#5091,.T.);
#1913=FACE_BOUND('',#5097,.T.);
#1914=FACE_BOUND('',#5135,.T.);
#1915=FACE_BOUND('',#5136,.T.);
#1916=FACE_BOUND('',#5140,.T.);
#1917=FACE_BOUND('',#5141,.T.);
#1918=FACE_BOUND('',#5174,.T.);
#1919=FACE_BOUND('',#5175,.T.);
#1920=FACE_BOUND('',#5176,.T.);
#1921=FACE_BOUND('',#5192,.T.);
#1922=FACE_BOUND('',#5208,.T.);
#1923=FACE_BOUND('',#5215,.T.);
#1924=FACE_BOUND('',#5229,.T.);
#1925=FACE_BOUND('',#5254,.T.);
#1926=FACE_BOUND('',#5260,.T.);
#1927=FACE_BOUND('',#5262,.T.);
#1928=FACE_BOUND('',#5395,.T.);
#1929=FACE_BOUND('',#5397,.T.);
#1930=FACE_BOUND('',#5494,.T.);
#1931=FACE_BOUND('',#5501,.T.);
#1932=FACE_BOUND('',#5509,.T.);
#1933=FACE_BOUND('',#5577,.T.);
#1934=FACE_BOUND('',#5578,.T.);
#1935=FACE_BOUND('',#5579,.T.);
#1936=FACE_BOUND('',#5580,.T.);
#1937=FACE_BOUND('',#5581,.T.);
#1938=FACE_BOUND('',#5582,.T.);
#1939=FACE_BOUND('',#5583,.T.);
#1940=FACE_BOUND('',#5584,.T.);
#1941=FACE_BOUND('',#5585,.T.);
#1942=FACE_BOUND('',#5586,.T.);
#1943=FACE_BOUND('',#5587,.T.);
#1944=FACE_BOUND('',#5588,.T.);
#1945=FACE_BOUND('',#5593,.T.);
#1946=FACE_BOUND('',#5595,.T.);
#1947=FACE_BOUND('',#5599,.T.);
#1948=FACE_BOUND('',#5603,.T.);
#1949=FACE_BOUND('',#5604,.T.);
#1950=FACE_BOUND('',#5607,.T.);
#1951=FACE_BOUND('',#5612,.T.);
#1952=FACE_BOUND('',#5617,.T.);
#1953=FACE_BOUND('',#5670,.T.);
#1954=FACE_BOUND('',#5671,.T.);
#1955=FACE_BOUND('',#5677,.T.);
#1956=FACE_BOUND('',#5678,.T.);
#1957=FACE_BOUND('',#5684,.T.);
#1958=FACE_BOUND('',#5685,.T.);
#1959=FACE_BOUND('',#5692,.T.);
#1960=FACE_BOUND('',#5693,.T.);
#1961=FACE_BOUND('',#5699,.T.);
#1962=FACE_BOUND('',#5700,.T.);
#1963=FACE_BOUND('',#5717,.T.);
#1964=FACE_BOUND('',#5718,.T.);
#1965=FACE_BOUND('',#5719,.T.);
#1966=FACE_BOUND('',#5720,.T.);
#1967=FACE_BOUND('',#5744,.T.);
#1968=FACE_BOUND('',#5745,.T.);
#1969=FACE_BOUND('',#5746,.T.);
#1970=FACE_BOUND('',#5752,.T.);
#1971=FACE_BOUND('',#5753,.T.);
#1972=FACE_BOUND('',#5758,.T.);
#1973=FACE_BOUND('',#5759,.T.);
#1974=FACE_BOUND('',#5784,.T.);
#1975=FACE_BOUND('',#5790,.T.);
#1976=FACE_BOUND('',#5998,.T.);
#1977=FACE_BOUND('',#5999,.T.);
#1978=FACE_BOUND('',#6039,.T.);
#1979=FACE_BOUND('',#6040,.T.);
#1980=FACE_BOUND('',#6052,.T.);
#1981=FACE_BOUND('',#6062,.T.);
#1982=FACE_BOUND('',#6063,.T.);
#1983=FACE_BOUND('',#6064,.T.);
#1984=FACE_BOUND('',#6070,.T.);
#1985=FACE_BOUND('',#6073,.T.);
#1986=FACE_BOUND('',#6084,.T.);
#1987=FACE_BOUND('',#6088,.T.);
#1988=FACE_BOUND('',#6098,.T.);
#1989=FACE_BOUND('',#6101,.T.);
#1990=FACE_BOUND('',#6105,.T.);
#1991=FACE_BOUND('',#6107,.T.);
#1992=FACE_BOUND('',#6110,.T.);
#1993=FACE_BOUND('',#6113,.T.);
#1994=FACE_BOUND('',#6116,.T.);
#1995=FACE_BOUND('',#6119,.T.);
#1996=FACE_BOUND('',#6122,.T.);
#1997=FACE_BOUND('',#6124,.T.);
#1998=FACE_BOUND('',#6129,.T.);
#1999=FACE_BOUND('',#6142,.T.);
#2000=FACE_BOUND('',#6143,.T.);
#2001=FACE_BOUND('',#6144,.T.);
#2002=FACE_BOUND('',#6145,.T.);
#2003=FACE_BOUND('',#6146,.T.);
#2004=FACE_BOUND('',#6147,.T.);
#2005=FACE_BOUND('',#6148,.T.);
#2006=FACE_BOUND('',#6149,.T.);
#2007=FACE_BOUND('',#6150,.T.);
#2008=FACE_BOUND('',#6151,.T.);
#2009=FACE_BOUND('',#6152,.T.);
#2010=FACE_BOUND('',#6168,.T.);
#2011=FACE_BOUND('',#6169,.T.);
#2012=FACE_BOUND('',#6170,.T.);
#2013=FACE_BOUND('',#6171,.T.);
#2014=FACE_BOUND('',#6172,.T.);
#2015=FACE_BOUND('',#6173,.T.);
#2016=FACE_BOUND('',#6174,.T.);
#2017=FACE_BOUND('',#6175,.T.);
#2018=FACE_BOUND('',#6176,.T.);
#2019=FACE_BOUND('',#6177,.T.);
#2020=FACE_BOUND('',#6178,.T.);
#2021=FACE_BOUND('',#6200,.T.);
#2022=FACE_BOUND('',#6221,.T.);
#2023=FACE_BOUND('',#6222,.T.);
#2024=FACE_BOUND('',#6223,.T.);
#2025=FACE_BOUND('',#6224,.T.);
#2026=FACE_BOUND('',#6225,.T.);
#2027=FACE_BOUND('',#6226,.T.);
#2028=FACE_BOUND('',#6227,.T.);
#2029=FACE_BOUND('',#6228,.T.);
#2030=FACE_BOUND('',#6229,.T.);
#2031=FACE_BOUND('',#6230,.T.);
#2032=FACE_BOUND('',#6231,.T.);
#2033=FACE_BOUND('',#6240,.T.);
#2034=FACE_BOUND('',#6241,.T.);
#2035=FACE_BOUND('',#6242,.T.);
#2036=FACE_BOUND('',#6243,.T.);
#2037=FACE_BOUND('',#6244,.T.);
#2038=FACE_BOUND('',#6245,.T.);
#2039=FACE_BOUND('',#6246,.T.);
#2040=FACE_BOUND('',#6247,.T.);
#2041=FACE_BOUND('',#6248,.T.);
#2042=FACE_BOUND('',#6249,.T.);
#2043=FACE_BOUND('',#6250,.T.);
#2044=FACE_BOUND('',#6288,.T.);
#2045=CIRCLE('',#28705,0.975000000000001);
#2046=CIRCLE('',#28706,0.875);
#2047=CIRCLE('',#28708,0.975000000000001);
#2048=CIRCLE('',#28709,0.975000000000001);
#2049=CIRCLE('',#28710,0.975000000000001);
#2050=CIRCLE('',#28712,0.875);
#2051=CIRCLE('',#28714,0.875);
#2052=CIRCLE('',#28716,0.875);
#2053=CIRCLE('',#28718,0.875);
#2054=CIRCLE('',#28720,0.875);
#2055=CIRCLE('',#28722,0.875);
#2056=CIRCLE('',#28724,0.875);
#2057=CIRCLE('',#28726,0.975000000000001);
#2058=CIRCLE('',#28728,0.975000000000001);
#2059=CIRCLE('',#28729,0.975000000000001);
#2060=CIRCLE('',#28730,0.975000000000001);
#2061=CIRCLE('',#28735,0.975000000000001);
#2062=CIRCLE('',#28736,0.875);
#2063=CIRCLE('',#28738,0.975000000000001);
#2064=CIRCLE('',#28739,0.975000000000001);
#2065=CIRCLE('',#28740,0.975000000000001);
#2066=CIRCLE('',#28742,0.875);
#2067=CIRCLE('',#28744,0.875);
#2068=CIRCLE('',#28746,0.875);
#2069=CIRCLE('',#28748,0.875);
#2070=CIRCLE('',#28750,0.875);
#2071=CIRCLE('',#28752,0.875);
#2072=CIRCLE('',#28754,0.875);
#2073=CIRCLE('',#28756,1.8);
#2074=CIRCLE('',#28757,1.8);
#2075=CIRCLE('',#28758,1.9);
#2076=CIRCLE('',#28760,0.8);
#2077=CIRCLE('',#28761,0.8);
#2078=CIRCLE('',#28763,1.8);
#2079=CIRCLE('',#28764,1.8);
#2080=CIRCLE('',#28766,0.975000000000001);
#2081=CIRCLE('',#28768,0.975000000000001);
#2082=CIRCLE('',#28769,0.975000000000001);
#2083=CIRCLE('',#28770,0.975000000000001);
#2084=CIRCLE('',#28775,0.8);
#2085=CIRCLE('',#28776,0.700000000000011);
#2086=CIRCLE('',#28779,0.700000000000011);
#2087=CIRCLE('',#28782,0.8);
#2088=CIRCLE('',#28783,0.700000000000011);
#2089=CIRCLE('',#28786,0.8);
#2090=CIRCLE('',#28787,0.700000000000011);
#2091=CIRCLE('',#28790,0.8);
#2092=CIRCLE('',#28793,0.8);
#2093=CIRCLE('',#28795,0.499999999999985);
#2094=CIRCLE('',#28796,0.499999999999985);
#2095=CIRCLE('',#28797,0.499999999999985);
#2096=CIRCLE('',#28798,0.499999999999986);
#2097=CIRCLE('',#28800,0.700000000000011);
#2098=CIRCLE('',#28803,0.700000000000011);
#2099=CIRCLE('',#28806,0.8);
#2100=CIRCLE('',#28807,0.700000000000011);
#2101=CIRCLE('',#28810,0.700000000000011);
#2102=CIRCLE('',#28814,1.9);
#2103=CIRCLE('',#28815,1.9);
#2104=CIRCLE('',#28816,1.9);
#2105=CIRCLE('',#28818,0.499999999999986);
#2106=CIRCLE('',#28819,0.499999999999985);
#2107=CIRCLE('',#28820,0.499999999999985);
#2108=CIRCLE('',#28821,0.499999999999985);
#2109=CIRCLE('',#28823,1.8);
#2110=CIRCLE('',#28824,1.8);
#2111=CIRCLE('',#28826,1.8);
#2112=CIRCLE('',#28827,1.8);
#2113=CIRCLE('',#28829,1.8);
#2114=CIRCLE('',#28830,1.8);
#2115=CIRCLE('',#28832,1.8);
#2116=CIRCLE('',#28833,1.8);
#2117=CIRCLE('',#28836,0.4);
#2118=CIRCLE('',#28839,0.4);
#2119=CIRCLE('',#28842,0.4);
#2120=CIRCLE('',#28845,0.4);
#2121=CIRCLE('',#28847,0.4);
#2122=CIRCLE('',#28850,0.4);
#2123=CIRCLE('',#28852,1.9);
#2124=CIRCLE('',#28853,1.9);
#2125=CIRCLE('',#28854,1.9);
#2126=CIRCLE('',#28855,1.9);
#2127=CIRCLE('',#28859,0.4);
#2128=CIRCLE('',#28862,0.4);
#2129=CIRCLE('',#28873,1.8);
#2130=CIRCLE('',#28874,1.8);
#2131=CIRCLE('',#28876,1.8);
#2132=CIRCLE('',#28877,1.8);
#2133=CIRCLE('',#28880,0.8);
#2134=CIRCLE('',#28881,0.700000000000011);
#2135=CIRCLE('',#28884,0.8);
#2136=CIRCLE('',#28885,0.700000000000011);
#2137=CIRCLE('',#28888,0.8);
#2138=CIRCLE('',#28889,0.700000000000011);
#2139=CIRCLE('',#28892,0.8);
#2140=CIRCLE('',#28893,0.700000000000011);
#2141=CIRCLE('',#28896,0.8);
#2142=CIRCLE('',#28899,0.8);
#2143=CIRCLE('',#28901,0.499999999999986);
#2144=CIRCLE('',#28902,0.499999999999985);
#2145=CIRCLE('',#28903,0.499999999999985);
#2146=CIRCLE('',#28904,0.499999999999985);
#2147=CIRCLE('',#28906,0.700000000000011);
#2148=CIRCLE('',#28909,0.700000000000011);
#2149=CIRCLE('',#28912,0.8);
#2150=CIRCLE('',#28913,0.700000000000011);
#2151=CIRCLE('',#28916,0.8);
#2152=CIRCLE('',#28917,0.700000000000011);
#2153=CIRCLE('',#28922,1.9);
#2154=CIRCLE('',#28923,1.9);
#2155=CIRCLE('',#28924,1.9);
#2156=CIRCLE('',#28925,1.9);
#2157=CIRCLE('',#28927,0.499999999999985);
#2158=CIRCLE('',#28928,0.499999999999985);
#2159=CIRCLE('',#28929,0.499999999999985);
#2160=CIRCLE('',#28930,0.499999999999986);
#2161=CIRCLE('',#28932,1.8);
#2162=CIRCLE('',#28933,1.8);
#2163=CIRCLE('',#28935,1.8);
#2164=CIRCLE('',#28936,1.8);
#2165=CIRCLE('',#28939,0.4);
#2166=CIRCLE('',#28942,0.4);
#2167=CIRCLE('',#28945,0.4);
#2168=CIRCLE('',#28948,0.4);
#2169=CIRCLE('',#28950,0.4);
#2170=CIRCLE('',#28953,0.4);
#2171=CIRCLE('',#28955,1.9);
#2172=CIRCLE('',#28956,1.9);
#2173=CIRCLE('',#28957,1.9);
#2174=CIRCLE('',#28958,1.9);
#2175=CIRCLE('',#28965,0.4);
#2176=CIRCLE('',#28968,0.4);
#2177=CIRCLE('',#28974,1.8);
#2178=CIRCLE('',#28975,1.8);
#2179=CIRCLE('',#28977,1.8);
#2180=CIRCLE('',#28978,1.8);
#2181=CIRCLE('',#28981,1.8);
#2182=CIRCLE('',#28982,1.8);
#2183=CIRCLE('',#28984,1.8);
#2184=CIRCLE('',#28985,1.8);
#2185=CIRCLE('',#28988,1.8);
#2186=CIRCLE('',#28989,1.8);
#2187=CIRCLE('',#28991,1.8);
#2188=CIRCLE('',#28992,1.8);
#2189=CIRCLE('',#28995,0.605);
#2190=CIRCLE('',#28996,0.504999999999999);
#2191=CIRCLE('',#28998,0.504999999999999);
#2192=CIRCLE('',#29000,0.605);
#2193=CIRCLE('',#29002,0.605);
#2194=CIRCLE('',#29004,0.605);
#2195=CIRCLE('',#29006,0.504999999999999);
#2196=CIRCLE('',#29008,0.504999999999999);
#2197=CIRCLE('',#29117,0.605);
#2198=CIRCLE('',#29118,0.605);
#2199=CIRCLE('',#29148,2.5);
#2200=CIRCLE('',#29149,2.5);
#2201=CIRCLE('',#29150,2.42928932188135);
#2202=CIRCLE('',#29151,2.42928932188135);
#2203=CIRCLE('',#29153,2.37071067811866);
#2204=CIRCLE('',#29154,2.37071067811866);
#2205=CIRCLE('',#29156,2.5);
#2206=CIRCLE('',#29158,2.2);
#2207=CIRCLE('',#29161,0.504999999999999);
#2208=CIRCLE('',#29163,0.504999999999999);
#2209=CIRCLE('',#29165,0.605);
#2210=CIRCLE('',#29167,0.605);
#2211=CIRCLE('',#29169,0.504999999999999);
#2212=CIRCLE('',#29171,0.504999999999999);
#2213=CIRCLE('',#29174,2.75714285714286);
#2214=CIRCLE('',#29232,0.799999999999999);
#2215=CIRCLE('',#29233,0.8);
#2216=CIRCLE('',#29239,0.8);
#2217=CIRCLE('',#29240,0.799999999999999);
#2218=CIRCLE('',#29261,0.799999999999999);
#2219=CIRCLE('',#29262,0.8);
#2220=CIRCLE('',#29268,0.8);
#2221=CIRCLE('',#29269,0.799999999999999);
#2222=CIRCLE('',#29272,0.7);
#2223=CIRCLE('',#29275,0.699999999999999);
#2224=CIRCLE('',#29277,0.7);
#2225=CIRCLE('',#29281,0.699999999999999);
#2226=CIRCLE('',#29287,0.699999999999999);
#2227=CIRCLE('',#29290,0.7);
#2228=CIRCLE('',#29292,0.699999999999999);
#2229=CIRCLE('',#29296,0.7);
#2230=CIRCLE('',#29316,0.975000000000001);
#2231=CIRCLE('',#29317,0.975000000000001);
#2232=CIRCLE('',#29321,0.975000000000001);
#2233=CIRCLE('',#29322,0.975000000000001);
#2234=CIRCLE('',#29327,0.875);
#2235=CIRCLE('',#29329,0.875);
#2236=CIRCLE('',#29332,0.875);
#2237=CIRCLE('',#29334,0.875);
#2238=CIRCLE('',#29348,0.770710678118652);
#2239=CIRCLE('',#29349,0.599999999999999);
#2240=CIRCLE('',#29352,0.770710678118652);
#2241=CIRCLE('',#29353,0.599999999999999);
#2242=CIRCLE('',#29356,0.770710678118652);
#2243=CIRCLE('',#29357,0.599999999999999);
#2244=CIRCLE('',#29360,0.770710678118652);
#2245=CIRCLE('',#29361,0.599999999999999);
#2246=CIRCLE('',#29365,0.929289321881342);
#2247=CIRCLE('',#29368,0.929289321881342);
#2248=CIRCLE('',#29370,5.4);
#2249=CIRCLE('',#29371,1.8);
#2250=CIRCLE('',#29372,1.);
#2251=CIRCLE('',#29375,0.2);
#2252=CIRCLE('',#29376,0.2);
#2253=CIRCLE('',#29380,1.);
#2254=CIRCLE('',#29383,0.929289321881336);
#2255=CIRCLE('',#29384,1.);
#2256=CIRCLE('',#29387,0.929289321881336);
#2257=CIRCLE('',#29388,1.);
#2258=CIRCLE('',#29391,1.);
#2259=CIRCLE('',#29393,1.);
#2260=CIRCLE('',#29396,1.);
#2261=CIRCLE('',#29398,0.504999999999995);
#2262=CIRCLE('',#29403,0.5);
#2263=CIRCLE('',#29404,0.400000000000011);
#2264=CIRCLE('',#29407,0.5);
#2265=CIRCLE('',#29408,0.400000000000012);
#2266=CIRCLE('',#29411,1.65);
#2267=CIRCLE('',#29415,0.5);
#2268=CIRCLE('',#29416,0.400000000000012);
#2269=CIRCLE('',#29419,0.5);
#2270=CIRCLE('',#29420,0.400000000000011);
#2271=CIRCLE('',#29423,0.5);
#2272=CIRCLE('',#29426,0.5);
#2273=CIRCLE('',#29427,0.400000000000011);
#2274=CIRCLE('',#29430,0.5);
#2275=CIRCLE('',#29431,0.400000000000012);
#2276=CIRCLE('',#29434,0.5);
#2277=CIRCLE('',#29437,0.5);
#2278=CIRCLE('',#29438,0.400000000000012);
#2279=CIRCLE('',#29441,0.5);
#2280=CIRCLE('',#29442,0.400000000000011);
#2281=CIRCLE('',#29450,1.65);
#2282=CIRCLE('',#29452,0.9);
#2283=CIRCLE('',#29453,1.);
#2284=CIRCLE('',#29455,0.51);
#2285=CIRCLE('',#29458,0.41);
#2286=CIRCLE('',#29460,0.41);
#2287=CIRCLE('',#29462,0.405000000000001);
#2288=CIRCLE('',#29464,0.405000000000001);
#2289=CIRCLE('',#29472,1.65);
#2290=CIRCLE('',#29476,1.65);
#2291=CIRCLE('',#29478,1.65);
#2292=CIRCLE('',#29481,1.65);
#2293=CIRCLE('',#29483,1.65);
#2294=CIRCLE('',#29484,1.65);
#2295=CIRCLE('',#29485,1.65);
#2296=CIRCLE('',#29487,1.8);
#2297=CIRCLE('',#29490,2.755);
#2298=CIRCLE('',#29491,2.655);
#2299=CIRCLE('',#29493,2.655);
#2300=CIRCLE('',#29495,5.3);
#2301=CIRCLE('',#29497,5.);
#2302=CIRCLE('',#29499,5.);
#2303=CIRCLE('',#29502,5.);
#2304=CIRCLE('',#29503,0.4);
#2305=CIRCLE('',#29504,5.);
#2306=CIRCLE('',#29506,5.);
#2307=CIRCLE('',#29508,5.3);
#2308=CIRCLE('',#29510,5.4);
#2309=CIRCLE('',#29512,5.4);
#2310=CIRCLE('',#29516,0.9);
#2311=CIRCLE('',#29519,1.);
#2312=CIRCLE('',#29520,0.9);
#2313=CIRCLE('',#29523,1.);
#2314=CIRCLE('',#29524,0.9);
#2315=CIRCLE('',#29527,0.9);
#2316=CIRCLE('',#29537,1.486725);
#2317=CIRCLE('',#29542,1.486725);
#2318=CIRCLE('',#29544,1.2866);
#2319=CIRCLE('',#29551,2.25);
#2320=CIRCLE('',#29555,2.25);
#2321=CIRCLE('',#29559,2.25);
#2322=CIRCLE('',#29563,2.25);
#2323=CIRCLE('',#29567,2.25);
#2324=CIRCLE('',#29571,2.25);
#2325=CIRCLE('',#29572,2.25);
#2326=CIRCLE('',#29576,2.25);
#2327=CIRCLE('',#29580,2.25);
#2328=CIRCLE('',#29584,2.25);
#2329=CIRCLE('',#29588,2.25);
#2330=CIRCLE('',#29592,2.25);
#2331=CIRCLE('',#29596,2.25);
#2332=CIRCLE('',#29600,2.25);
#2333=CIRCLE('',#29604,2.25);
#2334=CIRCLE('',#29608,2.25);
#2335=CIRCLE('',#29612,2.25);
#2336=CIRCLE('',#29616,2.25);
#2337=CIRCLE('',#29620,2.25);
#2338=CIRCLE('',#29624,2.25);
#2339=CIRCLE('',#29628,2.25);
#2340=CIRCLE('',#29632,2.25);
#2341=CIRCLE('',#29636,2.25);
#2342=CIRCLE('',#29640,2.25);
#2343=CIRCLE('',#29644,2.25);
#2344=CIRCLE('',#29646,2.1);
#2345=CIRCLE('',#29647,2.25);
#2346=CIRCLE('',#29648,2.25);
#2347=CIRCLE('',#29649,2.25);
#2348=CIRCLE('',#29650,2.25);
#2349=CIRCLE('',#29651,2.25);
#2350=CIRCLE('',#29652,2.25);
#2351=CIRCLE('',#29653,2.25);
#2352=CIRCLE('',#29654,2.25);
#2353=CIRCLE('',#29655,2.25);
#2354=CIRCLE('',#29656,2.25);
#2355=CIRCLE('',#29657,2.25);
#2356=CIRCLE('',#29658,2.25);
#2357=CIRCLE('',#29659,2.25);
#2358=CIRCLE('',#29660,2.25);
#2359=CIRCLE('',#29661,2.25);
#2360=CIRCLE('',#29662,2.25);
#2361=CIRCLE('',#29663,2.25);
#2362=CIRCLE('',#29664,2.25);
#2363=CIRCLE('',#29665,2.25);
#2364=CIRCLE('',#29666,2.25);
#2365=CIRCLE('',#29667,2.25);
#2366=CIRCLE('',#29668,2.25);
#2367=CIRCLE('',#29669,2.25);
#2368=CIRCLE('',#29670,2.25);
#2369=CIRCLE('',#29672,2.25);
#2370=CIRCLE('',#29674,2.25);
#2371=CIRCLE('',#29676,2.25);
#2372=CIRCLE('',#29678,2.25);
#2373=CIRCLE('',#29680,2.25);
#2374=CIRCLE('',#29682,2.25);
#2375=CIRCLE('',#29684,2.25);
#2376=CIRCLE('',#29686,2.25);
#2377=CIRCLE('',#29688,2.25);
#2378=CIRCLE('',#29690,2.25);
#2379=CIRCLE('',#29692,2.25);
#2380=CIRCLE('',#29694,2.25);
#2381=CIRCLE('',#29696,2.25);
#2382=CIRCLE('',#29698,2.25);
#2383=CIRCLE('',#29700,2.25);
#2384=CIRCLE('',#29702,2.25);
#2385=CIRCLE('',#29704,2.25);
#2386=CIRCLE('',#29706,2.25);
#2387=CIRCLE('',#29708,2.25);
#2388=CIRCLE('',#29710,2.25);
#2389=CIRCLE('',#29712,2.25);
#2390=CIRCLE('',#29714,2.25);
#2391=CIRCLE('',#29716,2.25);
#2392=CIRCLE('',#29718,1.2866);
#2393=CIRCLE('',#29720,1.486725);
#2394=CIRCLE('',#29722,2.55);
#2395=CIRCLE('',#29724,2.65);
#2396=CIRCLE('',#29726,2.65);
#2397=CIRCLE('',#29728,2.5);
#2398=CIRCLE('',#29731,2.15);
#2399=CIRCLE('',#29733,2.25);
#2400=CIRCLE('',#29738,0.3933);
#2401=CIRCLE('',#29754,0.322275);
#2402=CIRCLE('',#29771,1.1);
#2403=CIRCLE('',#29775,1.1);
#2404=CIRCLE('',#29779,1.1);
#2405=CIRCLE('',#29783,1.1);
#2406=CIRCLE('',#29787,1.1);
#2407=CIRCLE('',#29791,1.1);
#2408=CIRCLE('',#29795,1.1);
#2409=CIRCLE('',#29799,1.1);
#2410=CIRCLE('',#29803,1.1);
#2411=CIRCLE('',#29807,1.1);
#2412=CIRCLE('',#29811,1.1);
#2413=CIRCLE('',#29815,1.1);
#2414=CIRCLE('',#29819,1.1);
#2415=CIRCLE('',#29823,1.1);
#2416=CIRCLE('',#29824,1.1);
#2417=CIRCLE('',#29828,1.1);
#2418=CIRCLE('',#29832,1.1);
#2419=CIRCLE('',#29836,1.1);
#2420=CIRCLE('',#29840,1.1);
#2421=CIRCLE('',#29843,1.1);
#2422=CIRCLE('',#29844,1.1);
#2423=CIRCLE('',#29845,1.1);
#2424=CIRCLE('',#29846,1.1);
#2425=CIRCLE('',#29847,1.1);
#2426=CIRCLE('',#29848,1.1);
#2427=CIRCLE('',#29849,1.1);
#2428=CIRCLE('',#29850,1.1);
#2429=CIRCLE('',#29851,1.1);
#2430=CIRCLE('',#29852,1.1);
#2431=CIRCLE('',#29853,1.1);
#2432=CIRCLE('',#29854,1.1);
#2433=CIRCLE('',#29855,1.1);
#2434=CIRCLE('',#29856,1.1);
#2435=CIRCLE('',#29857,1.1);
#2436=CIRCLE('',#29858,1.1);
#2437=CIRCLE('',#29859,1.1);
#2438=CIRCLE('',#29860,1.1);
#2439=CIRCLE('',#29861,1.1);
#2440=CIRCLE('',#29863,0.3933);
#2441=CIRCLE('',#29864,0.3933);
#2442=CIRCLE('',#29865,0.322275);
#2443=CIRCLE('',#29868,0.35);
#2444=CIRCLE('',#29871,0.3933);
#2445=CIRCLE('',#29873,0.9);
#2446=CIRCLE('',#29876,1.);
#2447=CIRCLE('',#29880,0.4);
#2448=CIRCLE('',#29881,0.4);
#2449=CIRCLE('',#29884,0.6);
#2450=CIRCLE('',#29893,0.6);
#2451=CIRCLE('',#29895,0.6);
#2452=CIRCLE('',#29896,0.6);
#2453=CIRCLE('',#29899,0.300000000000001);
#2454=CIRCLE('',#29900,0.300000000000001);
#2455=CIRCLE('',#29905,0.300000000000001);
#2456=CIRCLE('',#29906,0.300000000000001);
#2457=CIRCLE('',#29966,2.9);
#2458=CIRCLE('',#29968,2.9);
#2459=CIRCLE('',#29970,2.95);
#2460=CIRCLE('',#29972,3.15);
#2461=CIRCLE('',#29974,3.15);
#2462=CIRCLE('',#29976,3.3);
#2463=CIRCLE('',#29978,3.3);
#2464=CIRCLE('',#29980,3.2);
#2465=CIRCLE('',#29985,1.25);
#2466=CIRCLE('',#29986,1.25);
#2467=CIRCLE('',#29988,0.299999999999997);
#2468=CIRCLE('',#29989,1.5);
#2469=CIRCLE('',#29991,0.599999999999994);
#2470=CIRCLE('',#29992,0.599999999999994);
#2471=CIRCLE('',#29994,0.5);
#2472=CIRCLE('',#29997,1.59999999999999);
#2473=CIRCLE('',#29999,1.7);
#2474=CIRCLE('',#30001,1.7);
#2475=CIRCLE('',#30003,1.59999999999999);
#2476=CIRCLE('',#30006,1.09999999999999);
#2477=CIRCLE('',#30009,0.15);
#2478=CIRCLE('',#30010,0.15);
#2479=CIRCLE('',#30049,1.5);
#2480=CIRCLE('',#30050,1.4);
#2481=CIRCLE('',#30053,1.5);
#2482=CIRCLE('',#30054,1.4);
#2483=CIRCLE('',#30057,1.5);
#2484=CIRCLE('',#30058,1.4);
#2485=CIRCLE('',#30061,1.5);
#2486=CIRCLE('',#30062,1.4);
#2487=CIRCLE('',#30066,1.5);
#2488=CIRCLE('',#30069,1.5);
#2489=CIRCLE('',#30071,1.);
#2490=CIRCLE('',#30072,1.);
#2491=CIRCLE('',#30078,0.975000000000001);
#2492=CIRCLE('',#30079,0.975000000000001);
#2493=CIRCLE('',#30085,0.975000000000001);
#2494=CIRCLE('',#30086,0.975000000000001);
#2495=CIRCLE('',#30091,0.975000000000001);
#2496=CIRCLE('',#30092,0.875);
#2497=CIRCLE('',#30094,0.875);
#2498=CIRCLE('',#30096,0.975000000000001);
#2499=CIRCLE('',#30099,0.875);
#2500=CIRCLE('',#30101,0.875);
#2501=CIRCLE('',#30103,0.975000000000001);
#2502=CIRCLE('',#30105,0.975000000000001);
#2503=CIRCLE('',#30107,0.875);
#2504=CIRCLE('',#30109,0.875);
#2505=CIRCLE('',#30112,0.875);
#2506=CIRCLE('',#30114,0.875);
#2507=CIRCLE('',#30117,0.899999999999999);
#2508=CIRCLE('',#30119,0.899999999999999);
#2509=CIRCLE('',#30121,0.899999999999999);
#2510=CIRCLE('',#30123,0.899999999999999);
#2511=CIRCLE('',#30126,1.37071067811866);
#2512=CIRCLE('',#30127,1.2);
#2513=CIRCLE('',#30130,1.37071067811866);
#2514=CIRCLE('',#30131,1.2);
#2515=CIRCLE('',#30134,1.2);
#2516=CIRCLE('',#30135,1.2);
#2517=CIRCLE('',#30136,1.);
#2518=CIRCLE('',#30137,1.);
#2519=CIRCLE('',#30140,1.37071067811866);
#2520=CIRCLE('',#30143,1.37071067811866);
#2521=CIRCLE('',#30155,1.5);
#2522=CIRCLE('',#30158,1.5);
#2523=CIRCLE('',#30166,0.199999999999999);
#2524=CIRCLE('',#30167,1.10000000000001);
#2525=CIRCLE('',#30169,0.199999999999999);
#2526=CIRCLE('',#30171,0.199999999999999);
#2527=CIRCLE('',#30174,0.2);
#2528=CIRCLE('',#30176,0.199999999999999);
#2529=CIRCLE('',#30177,1.09999999999999);
#2530=CIRCLE('',#30178,0.199999999999999);
#2531=CIRCLE('',#30180,0.2);
#2532=CIRCLE('',#30182,0.199999999999999);
#2533=CIRCLE('',#30186,0.4925);
#2534=CIRCLE('',#30198,0.40705);
#2535=CIRCLE('',#30210,0.5);
#2536=CIRCLE('',#30211,0.5);
#2537=CIRCLE('',#30212,1.25);
#2538=CIRCLE('',#30214,1.05);
#2539=CIRCLE('',#30215,0.85);
#2540=CIRCLE('',#30216,0.85);
#2541=CIRCLE('',#30218,0.6);
#2542=CIRCLE('',#30221,0.6);
#2543=CIRCLE('',#30224,1.25);
#2544=CIRCLE('',#30225,0.4925);
#2545=CIRCLE('',#30227,1.25);
#2546=CIRCLE('',#30230,0.40705);
#2547=CIRCLE('',#30232,0.4925);
#2548=CIRCLE('',#30233,0.4925);
#2549=CIRCLE('',#30235,0.42);
#2550=CIRCLE('',#30286,0.7911);
#2551=CIRCLE('',#30346,0.7911);
#2552=CIRCLE('',#30348,0.6767);
#2553=CIRCLE('',#30419,0.7911);
#2554=CIRCLE('',#30420,0.7911);
#2555=CIRCLE('',#30422,0.7911);
#2556=CIRCLE('',#30423,0.7911);
#2557=CIRCLE('',#30424,0.6767);
#2558=CIRCLE('',#30427,0.8511);
#2559=CIRCLE('',#30428,0.06);
#2560=CIRCLE('',#30429,0.7911);
#2561=CIRCLE('',#30433,1.14);
#2562=CIRCLE('',#30442,0.7);
#2563=CIRCLE('',#30446,0.805);
#2564=CIRCLE('',#30447,0.885);
#2565=CIRCLE('',#30449,0.805);
#2566=CIRCLE('',#30451,1.14);
#2567=CIRCLE('',#30453,0.885);
#2568=CIRCLE('',#30455,1.14);
#2569=CIRCLE('',#30466,0.85);
#2570=CIRCLE('',#30467,0.85);
#2571=CIRCLE('',#30469,1.5);
#2572=CIRCLE('',#30471,1.5);
#2573=CIRCLE('',#30473,1.46);
#2574=CIRCLE('',#30475,0.89);
#2575=CIRCLE('',#30479,1.1);
#2576=CIRCLE('',#30480,1.27071067811866);
#2577=CIRCLE('',#30481,1.27071067811866);
#2578=CIRCLE('',#30483,1.32928932188137);
#2579=CIRCLE('',#30484,1.32928932188137);
#2580=CIRCLE('',#30487,1.40000000000001);
#2581=CIRCLE('',#30488,1.40000000000001);
#2582=CIRCLE('',#30490,1.40000000000001);
#2583=CIRCLE('',#30492,0.619999999999999);
#2584=CIRCLE('',#30493,0.52);
#2585=CIRCLE('',#30495,0.52);
#2586=CIRCLE('',#30497,1.09999999999999);
#2587=CIRCLE('',#30499,0.619999999999999);
#2588=CIRCLE('',#30501,1.09999999999999);
#2589=CIRCLE('',#30503,1.40000000000001);
#2590=CIRCLE('',#30504,1.40000000000001);
#2591=CIRCLE('',#30505,1.30000000000001);
#2592=CIRCLE('',#30507,1.40000000000001);
#2593=CIRCLE('',#30509,1.);
#2594=CIRCLE('',#30511,1.30000000000002);
#2595=CIRCLE('',#30513,1.30000000000002);
#2596=CIRCLE('',#30515,1.40000000000001);
#2597=CIRCLE('',#30517,1.40000000000001);
#2598=CIRCLE('',#30519,1.29999999999999);
#2599=CIRCLE('',#30521,1.29999999999999);
#2600=CIRCLE('',#30523,1.40000000000001);
#2601=CIRCLE('',#30525,1.40000000000001);
#2602=CIRCLE('',#30527,1.30000000000002);
#2603=CIRCLE('',#30529,1.30000000000002);
#2604=CIRCLE('',#30532,1.5);
#2605=CIRCLE('',#30534,1.6);
#2606=CIRCLE('',#30536,1.60000000000002);
#2607=CIRCLE('',#30538,1.5);
#2608=CIRCLE('',#30540,0.999999999999996);
#2609=CIRCLE('',#30546,1.19999999999999);
#2610=CIRCLE('',#30549,1.19999999999999);
#2611=CIRCLE('',#30555,0.975000000000001);
#2612=CIRCLE('',#30556,0.875);
#2613=CIRCLE('',#30558,0.975000000000001);
#2614=CIRCLE('',#30559,0.975000000000001);
#2615=CIRCLE('',#30560,1.4);
#2616=CIRCLE('',#30561,1.4);
#2617=CIRCLE('',#30562,1.4);
#2618=CIRCLE('',#30563,1.4);
#2619=CIRCLE('',#30564,1.4);
#2620=CIRCLE('',#30565,1.4);
#2621=CIRCLE('',#30566,0.975000000000001);
#2622=CIRCLE('',#30567,0.975000000000001);
#2623=CIRCLE('',#30569,0.875);
#2624=CIRCLE('',#30571,0.875);
#2625=CIRCLE('',#30573,0.875);
#2626=CIRCLE('',#30575,0.875);
#2627=CIRCLE('',#30577,0.875);
#2628=CIRCLE('',#30579,0.875);
#2629=CIRCLE('',#30581,0.875);
#2630=CIRCLE('',#30583,0.875);
#2631=CIRCLE('',#30585,0.875);
#2632=CIRCLE('',#30587,1.3);
#2633=CIRCLE('',#30589,1.3);
#2634=CIRCLE('',#30591,1.3);
#2635=CIRCLE('',#30593,1.3);
#2636=CIRCLE('',#30595,0.975000000000001);
#2637=CIRCLE('',#30596,0.875);
#2638=CIRCLE('',#30598,0.975000000000001);
#2639=CIRCLE('',#30599,0.975000000000001);
#2640=CIRCLE('',#30600,1.4);
#2641=CIRCLE('',#30601,1.4);
#2642=CIRCLE('',#30602,1.4);
#2643=CIRCLE('',#30603,1.4);
#2644=CIRCLE('',#30604,1.4);
#2645=CIRCLE('',#30605,1.4);
#2646=CIRCLE('',#30606,0.975000000000001);
#2647=CIRCLE('',#30607,0.975000000000001);
#2648=CIRCLE('',#30609,0.875);
#2649=CIRCLE('',#30611,0.875);
#2650=CIRCLE('',#30613,0.875);
#2651=CIRCLE('',#30615,0.875);
#2652=CIRCLE('',#30617,0.875);
#2653=CIRCLE('',#30619,0.875);
#2654=CIRCLE('',#30621,0.875);
#2655=CIRCLE('',#30623,0.875);
#2656=CIRCLE('',#30625,0.875);
#2657=CIRCLE('',#30628,0.3);
#2658=CIRCLE('',#30629,0.400000000000004);
#2659=CIRCLE('',#30632,0.3);
#2660=CIRCLE('',#30633,0.4);
#2661=CIRCLE('',#30636,0.3);
#2662=CIRCLE('',#30637,0.400000000000003);
#2663=CIRCLE('',#30640,0.3);
#2664=CIRCLE('',#30641,0.400000000000003);
#2665=CIRCLE('',#30643,0.3);
#2666=CIRCLE('',#30646,0.3);
#2667=CIRCLE('',#30648,0.699999999999997);
#2668=CIRCLE('',#30649,0.699999999999997);
#2669=CIRCLE('',#30650,0.7);
#2670=CIRCLE('',#30651,0.700000000000001);
#2671=CIRCLE('',#30653,1.3);
#2672=CIRCLE('',#30655,1.3);
#2673=CIRCLE('',#30657,1.3);
#2674=CIRCLE('',#30659,1.3);
#2675=CIRCLE('',#30661,1.3);
#2676=CIRCLE('',#30663,1.3);
#2677=CIRCLE('',#30665,1.3);
#2678=CIRCLE('',#30667,1.3);
#2679=CIRCLE('',#30669,1.3);
#2680=CIRCLE('',#30671,1.3);
#2681=CIRCLE('',#30673,1.3);
#2682=CIRCLE('',#30675,1.3);
#2683=CIRCLE('',#30677,1.3);
#2684=CIRCLE('',#30679,1.3);
#2685=CIRCLE('',#30681,1.3);
#2686=CIRCLE('',#30683,1.3);
#2687=CIRCLE('',#30685,1.3);
#2688=CIRCLE('',#30687,1.3);
#2689=CIRCLE('',#30689,0.975000000000001);
#2690=CIRCLE('',#30691,0.975000000000001);
#2691=CIRCLE('',#30692,0.975000000000001);
#2692=CIRCLE('',#30693,1.4);
#2693=CIRCLE('',#30694,1.4);
#2694=CIRCLE('',#30695,1.4);
#2695=CIRCLE('',#30696,1.4);
#2696=CIRCLE('',#30697,1.4);
#2697=CIRCLE('',#30698,1.4);
#2698=CIRCLE('',#30699,0.975000000000001);
#2699=CIRCLE('',#30700,0.975000000000001);
#2700=CIRCLE('',#30706,1.3);
#2701=CIRCLE('',#30708,1.3);
#2702=CIRCLE('',#30710,0.975000000000001);
#2703=CIRCLE('',#30712,0.975000000000001);
#2704=CIRCLE('',#30713,0.975000000000001);
#2705=CIRCLE('',#30714,1.4);
#2706=CIRCLE('',#30715,1.4);
#2707=CIRCLE('',#30716,1.4);
#2708=CIRCLE('',#30717,1.4);
#2709=CIRCLE('',#30718,1.4);
#2710=CIRCLE('',#30719,1.4);
#2711=CIRCLE('',#30720,0.975000000000001);
#2712=CIRCLE('',#30721,0.975000000000001);
#2713=CIRCLE('',#30728,0.8);
#2714=CIRCLE('',#30731,0.8);
#2715=CIRCLE('',#30734,0.8);
#2716=CIRCLE('',#30737,0.8);
#2717=CIRCLE('',#30739,0.8);
#2718=CIRCLE('',#30742,0.8);
#2719=CIRCLE('',#30756,0.8);
#2720=CIRCLE('',#30757,0.7);
#2721=CIRCLE('',#30760,0.8);
#2722=CIRCLE('',#30761,0.700000000000001);
#2723=CIRCLE('',#30764,0.699999999999997);
#2724=CIRCLE('',#30767,0.699999999999997);
#2725=CIRCLE('',#30771,0.4);
#2726=CIRCLE('',#30772,0.400000000000003);
#2727=CIRCLE('',#30773,0.400000000000003);
#2728=CIRCLE('',#30774,0.400000000000004);
#2729=CIRCLE('',#30776,0.3);
#2730=CIRCLE('',#30779,0.3);
#2731=CONICAL_SURFACE('',#28704,0.925000000000001,0.785398163397457);
#2732=CONICAL_SURFACE('',#28713,0.925000000000001,0.785398163397457);
#2733=CONICAL_SURFACE('',#28717,0.925000000000001,0.785398163397457);
#2734=CONICAL_SURFACE('',#28721,0.925000000000001,0.785398163397457);
#2735=CONICAL_SURFACE('',#28725,0.925000000000001,0.785398163397457);
#2736=CONICAL_SURFACE('',#28731,0.925000000000001,0.785398163397457);
#2737=CONICAL_SURFACE('',#28732,0.925000000000001,0.785398163397457);
#2738=CONICAL_SURFACE('',#28733,0.925000000000001,0.785398163397457);
#2739=CONICAL_SURFACE('',#28734,0.925000000000001,0.785398163397457);
#2740=CONICAL_SURFACE('',#28743,0.925000000000001,0.785398163397457);
#2741=CONICAL_SURFACE('',#28747,0.925000000000001,0.785398163397457);
#2742=CONICAL_SURFACE('',#28751,0.925000000000001,0.785398163397457);
#2743=CONICAL_SURFACE('',#28755,1.85,0.785398163397422);
#2744=CONICAL_SURFACE('',#28765,0.925000000000001,0.785398163397457);
#2745=CONICAL_SURFACE('',#28771,0.925000000000001,0.785398163397457);
#2746=CONICAL_SURFACE('',#28772,0.925000000000001,0.785398163397457);
#2747=CONICAL_SURFACE('',#28773,0.925000000000001,0.785398163397457);
#2748=CONICAL_SURFACE('',#28774,0.750000000000006,0.78539816339742);
#2749=CONICAL_SURFACE('',#28778,0.750000000000006,0.78539816339742);
#2750=CONICAL_SURFACE('',#28781,0.750000000000006,0.78539816339742);
#2751=CONICAL_SURFACE('',#28785,0.750000000000005,0.785398163397422);
#2752=CONICAL_SURFACE('',#28799,0.750000000000006,0.785398163397384);
#2753=CONICAL_SURFACE('',#28802,0.750000000000005,0.785398163397387);
#2754=CONICAL_SURFACE('',#28805,0.750000000000006,0.785398163397384);
#2755=CONICAL_SURFACE('',#28809,0.750000000000006,0.785398163397384);
#2756=CONICAL_SURFACE('',#28822,1.85,0.785398163397422);
#2757=CONICAL_SURFACE('',#28828,1.85,0.785398163397422);
#2758=CONICAL_SURFACE('',#28835,0.449999999999992,0.785398163397365);
#2759=CONICAL_SURFACE('',#28838,0.449999999999993,0.785398163397367);
#2760=CONICAL_SURFACE('',#28841,0.449999999999993,0.785398163397367);
#2761=CONICAL_SURFACE('',#28844,0.449999999999993,0.785398163397371);
#2762=CONICAL_SURFACE('',#28856,1.85,0.785398163397422);
#2763=CONICAL_SURFACE('',#28858,0.449999999999992,0.785398163397401);
#2764=CONICAL_SURFACE('',#28861,0.449999999999993,0.785398163397403);
#2765=CONICAL_SURFACE('',#28864,0.449999999999993,0.785398163397403);
#2766=CONICAL_SURFACE('',#28866,0.449999999999993,0.785398163397406);
#2767=CONICAL_SURFACE('',#28870,1.85,0.785398163397422);
#2768=CONICAL_SURFACE('',#28871,1.85,0.785398163397422);
#2769=CONICAL_SURFACE('',#28872,1.85,0.785398163397422);
#2770=CONICAL_SURFACE('',#28878,1.85,0.785398163397422);
#2771=CONICAL_SURFACE('',#28879,0.750000000000006,0.785398163397384);
#2772=CONICAL_SURFACE('',#28883,0.750000000000006,0.785398163397384);
#2773=CONICAL_SURFACE('',#28887,0.750000000000005,0.785398163397387);
#2774=CONICAL_SURFACE('',#28891,0.750000000000006,0.785398163397384);
#2775=CONICAL_SURFACE('',#28905,0.750000000000006,0.78539816339742);
#2776=CONICAL_SURFACE('',#28908,0.750000000000006,0.78539816339742);
#2777=CONICAL_SURFACE('',#28911,0.750000000000005,0.785398163397422);
#2778=CONICAL_SURFACE('',#28915,0.750000000000006,0.78539816339742);
#2779=CONICAL_SURFACE('',#28931,1.85,0.785398163397422);
#2780=CONICAL_SURFACE('',#28938,0.449999999999992,0.785398163397401);
#2781=CONICAL_SURFACE('',#28941,0.449999999999993,0.785398163397403);
#2782=CONICAL_SURFACE('',#28944,0.449999999999993,0.785398163397403);
#2783=CONICAL_SURFACE('',#28947,0.449999999999993,0.785398163397406);
#2784=CONICAL_SURFACE('',#28960,0.449999999999992,0.785398163397365);
#2785=CONICAL_SURFACE('',#28962,0.449999999999993,0.785398163397367);
#2786=CONICAL_SURFACE('',#28964,0.449999999999993,0.785398163397367);
#2787=CONICAL_SURFACE('',#28967,0.449999999999993,0.785398163397371);
#2788=CONICAL_SURFACE('',#28972,1.85,0.785398163397422);
#2789=CONICAL_SURFACE('',#28973,1.85,0.785398163397422);
#2790=CONICAL_SURFACE('',#28979,1.85,0.785398163397422);
#2791=CONICAL_SURFACE('',#28980,1.85,0.785398163397422);
#2792=CONICAL_SURFACE('',#28986,1.85,0.785398163397422);
#2793=CONICAL_SURFACE('',#28987,1.85,0.785398163397422);
#2794=CONICAL_SURFACE('',#28993,1.85,0.785398163397422);
#2795=CONICAL_SURFACE('',#28994,0.555,0.785398163397484);
#2796=CONICAL_SURFACE('',#29001,0.555,0.785398163397484);
#2797=CONICAL_SURFACE('',#29005,0.555,0.785398163397484);
#2798=CONICAL_SURFACE('',#29009,0.555,0.785398163397484);
#2799=CONICAL_SURFACE('',#29147,2.46464466094067,0.392699081698708);
#2800=CONICAL_SURFACE('',#29152,2.4,0.785398163397442);
#2801=CONICAL_SURFACE('',#29157,2.28535533905933,1.17809724509617);
#2802=CONICAL_SURFACE('',#29160,0.555,0.785398163397484);
#2803=CONICAL_SURFACE('',#29164,0.555,0.785398163397484);
#2804=CONICAL_SURFACE('',#29168,0.555,0.785398163397484);
#2805=CONICAL_SURFACE('',#29172,0.555,0.785398163397484);
#2806=CONICAL_SURFACE('',#29173,2.65,0.708626272127678);
#2807=CONICAL_SURFACE('',#29271,0.75,0.785398163397475);
#2808=CONICAL_SURFACE('',#29274,0.749999999999999,0.785398163397475);
#2809=CONICAL_SURFACE('',#29280,0.749999999999999,0.785398163397475);
#2810=CONICAL_SURFACE('',#29283,0.75,0.785398163397475);
#2811=CONICAL_SURFACE('',#29286,0.749999999999999,0.785398163397475);
#2812=CONICAL_SURFACE('',#29289,0.75,0.785398163397475);
#2813=CONICAL_SURFACE('',#29295,0.75,0.785398163397475);
#2814=CONICAL_SURFACE('',#29298,0.749999999999999,0.785398163397475);
#2815=CONICAL_SURFACE('',#29326,0.925000000000001,0.785398163397457);
#2816=CONICAL_SURFACE('',#29330,0.925000000000001,0.785398163397457);
#2817=CONICAL_SURFACE('',#29331,0.925000000000001,0.785398163397457);
#2818=CONICAL_SURFACE('',#29335,0.925000000000001,0.785398163397457);
#2819=CONICAL_SURFACE('',#29347,0.685355339059325,1.17809724509615);
#2820=CONICAL_SURFACE('',#29351,0.685355339059325,1.17809724509615);
#2821=CONICAL_SURFACE('',#29355,0.685355339059325,1.17809724509615);
#2822=CONICAL_SURFACE('',#29359,0.685355339059325,1.17809724509615);
#2823=CONICAL_SURFACE('',#29364,0.85,0.785398163397452);
#2824=CONICAL_SURFACE('',#29367,0.85,0.785398163397452);
#2825=CONICAL_SURFACE('',#29379,0.964644660940671,0.392699081698743);
#2826=CONICAL_SURFACE('',#29382,0.964644660940668,0.392699081698775);
#2827=CONICAL_SURFACE('',#29386,0.964644660940668,0.392699081698775);
#2828=CONICAL_SURFACE('',#29390,0.964644660940671,0.392699081698743);
#2829=CONICAL_SURFACE('',#29399,0.85,0.785398163397452);
#2830=CONICAL_SURFACE('',#29402,0.450000000000006,0.785398163397392);
#2831=CONICAL_SURFACE('',#29406,0.450000000000006,0.785398163397389);
#2832=CONICAL_SURFACE('',#29414,0.450000000000006,0.785398163397389);
#2833=CONICAL_SURFACE('',#29418,0.450000000000006,0.785398163397392);
#2834=CONICAL_SURFACE('',#29425,0.450000000000006,0.785398163397392);
#2835=CONICAL_SURFACE('',#29429,0.450000000000006,0.785398163397389);
#2836=CONICAL_SURFACE('',#29436,0.450000000000006,0.785398163397389);
#2837=CONICAL_SURFACE('',#29440,0.450000000000006,0.785398163397392);
#2838=CONICAL_SURFACE('',#29451,0.95,0.785398163397475);
#2839=CONICAL_SURFACE('',#29457,0.46,0.785398163397475);
#2840=CONICAL_SURFACE('',#29461,0.454999999999998,0.785398163397422);
#2841=CONICAL_SURFACE('',#29465,0.405000000000001,1.02974425867666);
#2842=CONICAL_SURFACE('',#29466,0.205,1.02974425867666);
#2843=CONICAL_SURFACE('',#29486,1.725,0.785398163397431);
#2844=CONICAL_SURFACE('',#29489,2.705,0.785398163397477);
#2845=CONICAL_SURFACE('',#29509,5.35,0.785398163397479);
#2846=CONICAL_SURFACE('',#29513,5.35,0.785398163397479);
#2847=CONICAL_SURFACE('',#29515,0.95,0.785398163397475);
#2848=CONICAL_SURFACE('',#29518,0.95,0.785398163397475);
#2849=CONICAL_SURFACE('',#29522,0.95,0.785398163397475);
#2850=CONICAL_SURFACE('',#29526,0.95,0.785398163397475);
#2851=CONICAL_SURFACE('',#29531,0.85,0.785398163397452);
#2852=CONICAL_SURFACE('',#29645,2.175,0.785398163397429);
#2853=CONICAL_SURFACE('',#29723,2.6,0.785398163397477);
#2854=CONICAL_SURFACE('',#29727,2.575,0.785398163397429);
#2855=CONICAL_SURFACE('',#29732,2.2,0.785398163397477);
#2856=CONICAL_SURFACE('',#29869,0.375,0.785398163397448);
#2857=CONICAL_SURFACE('',#29874,1.,0.785398163397445);
#2858=CONICAL_SURFACE('',#29875,1.05,0.463647609000806);
#2859=CONICAL_SURFACE('',#29971,3.05,0.785398163397449);
#2860=CONICAL_SURFACE('',#29979,3.25,0.785398163397447);
#2861=CONICAL_SURFACE('',#29995,0.549999999999997,0.785398163397422);
#2862=CONICAL_SURFACE('',#29998,1.65000000000001,0.785398163397493);
#2863=CONICAL_SURFACE('',#30002,1.65000000000001,0.785398163397484);
#2864=CONICAL_SURFACE('',#30005,1.175,0.785398163397466);
#2865=CONICAL_SURFACE('',#30048,1.45,0.785398163397448);
#2866=CONICAL_SURFACE('',#30052,1.45,0.78539816339746);
#2867=CONICAL_SURFACE('',#30056,1.45,0.78539816339746);
#2868=CONICAL_SURFACE('',#30060,1.45,0.785398163397448);
#2869=CONICAL_SURFACE('',#30090,0.925000000000001,0.785398163397457);
#2870=CONICAL_SURFACE('',#30097,0.925000000000001,0.785398163397457);
#2871=CONICAL_SURFACE('',#30098,0.925000000000001,0.785398163397457);
#2872=CONICAL_SURFACE('',#30102,0.925000000000001,0.785398163397457);
#2873=CONICAL_SURFACE('',#30106,0.925000000000001,0.785398163397457);
#2874=CONICAL_SURFACE('',#30110,0.925000000000001,0.785398163397457);
#2875=CONICAL_SURFACE('',#30111,0.925000000000001,0.785398163397457);
#2876=CONICAL_SURFACE('',#30115,0.925000000000001,0.785398163397457);
#2877=CONICAL_SURFACE('',#30116,0.949999999999999,0.785398163397455);
#2878=CONICAL_SURFACE('',#30120,0.949999999999999,0.785398163397455);
#2879=CONICAL_SURFACE('',#30125,1.28535533905933,1.17809724509618);
#2880=CONICAL_SURFACE('',#30129,1.28535533905933,1.17809724509618);
#2881=CONICAL_SURFACE('',#30139,1.28535533905933,1.17809724509618);
#2882=CONICAL_SURFACE('',#30142,1.28535533905933,1.17809724509618);
#2883=CONICAL_SURFACE('',#30145,0.949999999999999,0.785398163397455);
#2884=CONICAL_SURFACE('',#30146,0.949999999999999,0.785398163397455);
#2885=CONICAL_SURFACE('',#30150,1.4,0.785398163397448);
#2886=CONICAL_SURFACE('',#30152,1.4,0.785398163397448);
#2887=CONICAL_SURFACE('',#30154,1.4,0.785398163397448);
#2888=CONICAL_SURFACE('',#30157,1.4,0.785398163397448);
#2889=CONICAL_SURFACE('',#30219,0.75,0.463647609000806);
#2890=CONICAL_SURFACE('',#30220,0.75,0.463647609000806);
#2891=CONICAL_SURFACE('',#30228,1.15,0.785398163397448);
#2892=CONICAL_SURFACE('',#30236,0.46,0.785398163397448);
#2893=CONICAL_SURFACE('',#30432,1.28782032302755,1.0471975511966);
#2894=CONICAL_SURFACE('',#30443,0.75,0.785398163397451);
#2895=CONICAL_SURFACE('',#30445,0.845,0.785398163397448);
#2896=CONICAL_SURFACE('',#30452,0.845,0.785398163397448);
#2897=CONICAL_SURFACE('',#30456,1.28782032302755,1.0471975511966);
#2898=CONICAL_SURFACE('',#30460,1.28782032302755,1.0471975511966);
#2899=CONICAL_SURFACE('',#30472,1.48,0.785398163397449);
#2900=CONICAL_SURFACE('',#30476,0.87,0.785398163397449);
#2901=CONICAL_SURFACE('',#30478,1.18535533905933,1.17809724509622);
#2902=CONICAL_SURFACE('',#30482,1.30000000000001,0.78539816339746);
#2903=CONICAL_SURFACE('',#30486,1.36464466094069,0.392699081698615);
#2904=CONICAL_SURFACE('',#30491,0.569999999999999,0.785398163397448);
#2905=CONICAL_SURFACE('',#30498,0.569999999999999,0.785398163397448);
#2906=CONICAL_SURFACE('',#30502,1.35000000000001,0.785398163397418);
#2907=CONICAL_SURFACE('',#30533,1.54999999999999,0.785398163397423);
#2908=CONICAL_SURFACE('',#30537,1.54999999999999,0.785398163397517);
#2909=CONICAL_SURFACE('',#30545,1.14999999999999,0.785398163397454);
#2910=CONICAL_SURFACE('',#30551,1.14999999999999,0.785398163397454);
#2911=CONICAL_SURFACE('',#30554,0.925000000000001,0.785398163397455);
#2912=CONICAL_SURFACE('',#30570,0.925000000000001,0.785398163397455);
#2913=CONICAL_SURFACE('',#30574,0.925000000000001,0.785398163397455);
#2914=CONICAL_SURFACE('',#30578,0.925000000000001,0.785398163397455);
#2915=CONICAL_SURFACE('',#30582,0.925000000000001,0.785398163397455);
#2916=CONICAL_SURFACE('',#30586,1.35,0.785398163397455);
#2917=CONICAL_SURFACE('',#30590,1.35,0.785398163397455);
#2918=CONICAL_SURFACE('',#30594,0.925000000000001,0.785398163397455);
#2919=CONICAL_SURFACE('',#30610,0.925000000000001,0.785398163397455);
#2920=CONICAL_SURFACE('',#30614,0.925000000000001,0.785398163397455);
#2921=CONICAL_SURFACE('',#30618,0.925000000000001,0.785398163397455);
#2922=CONICAL_SURFACE('',#30622,0.925000000000001,0.785398163397455);
#2923=CONICAL_SURFACE('',#30627,0.350000000000002,0.785398163397469);
#2924=CONICAL_SURFACE('',#30631,0.35,0.785398163397446);
#2925=CONICAL_SURFACE('',#30635,0.350000000000001,0.785398163397461);
#2926=CONICAL_SURFACE('',#30639,0.350000000000001,0.785398163397461);
#2927=CONICAL_SURFACE('',#30652,1.35,0.785398163397455);
#2928=CONICAL_SURFACE('',#30656,1.35,0.785398163397455);
#2929=CONICAL_SURFACE('',#30660,1.35,0.785398163397455);
#2930=CONICAL_SURFACE('',#30664,1.35,0.785398163397455);
#2931=CONICAL_SURFACE('',#30668,1.35,0.785398163397455);
#2932=CONICAL_SURFACE('',#30672,1.35,0.785398163397455);
#2933=CONICAL_SURFACE('',#30676,1.35,0.785398163397455);
#2934=CONICAL_SURFACE('',#30680,1.35,0.785398163397455);
#2935=CONICAL_SURFACE('',#30684,1.35,0.785398163397455);
#2936=CONICAL_SURFACE('',#30688,0.925000000000001,0.785398163397455);
#2937=CONICAL_SURFACE('',#30701,0.925000000000001,0.785398163397455);
#2938=CONICAL_SURFACE('',#30702,0.925000000000001,0.785398163397455);
#2939=CONICAL_SURFACE('',#30703,0.925000000000001,0.785398163397455);
#2940=CONICAL_SURFACE('',#30704,0.925000000000001,0.785398163397455);
#2941=CONICAL_SURFACE('',#30705,1.35,0.785398163397455);
#2942=CONICAL_SURFACE('',#30709,0.925000000000001,0.785398163397455);
#2943=CONICAL_SURFACE('',#30722,0.925000000000001,0.785398163397455);
#2944=CONICAL_SURFACE('',#30723,0.925000000000001,0.785398163397455);
#2945=CONICAL_SURFACE('',#30724,0.925000000000001,0.785398163397455);
#2946=CONICAL_SURFACE('',#30725,0.925000000000001,0.785398163397455);
#2947=CONICAL_SURFACE('',#30727,0.75,0.785398163397444);
#2948=CONICAL_SURFACE('',#30730,0.75,0.785398163397447);
#2949=CONICAL_SURFACE('',#30733,0.749999999999998,0.785398163397465);
#2950=CONICAL_SURFACE('',#30736,0.749999999999998,0.785398163397465);
#2951=CONICAL_SURFACE('',#30743,1.35,0.785398163397455);
#2952=CONICAL_SURFACE('',#30744,1.35,0.785398163397455);
#2953=CONICAL_SURFACE('',#30745,1.35,0.785398163397455);
#2954=CONICAL_SURFACE('',#30746,1.35,0.785398163397455);
#2955=CONICAL_SURFACE('',#30747,1.35,0.785398163397455);
#2956=CONICAL_SURFACE('',#30748,1.35,0.785398163397455);
#2957=CONICAL_SURFACE('',#30749,1.35,0.785398163397455);
#2958=CONICAL_SURFACE('',#30750,1.35,0.785398163397455);
#2959=CONICAL_SURFACE('',#30751,1.35,0.785398163397455);
#2960=CONICAL_SURFACE('',#30752,1.35,0.785398163397455);
#2961=CONICAL_SURFACE('',#30753,1.35,0.785398163397455);
#2962=CONICAL_SURFACE('',#30754,1.35,0.785398163397455);
#2963=CONICAL_SURFACE('',#30755,0.75,0.785398163397475);
#2964=CONICAL_SURFACE('',#30759,0.75,0.785398163397472);
#2965=CONICAL_SURFACE('',#30763,0.749999999999998,0.785398163397494);
#2966=CONICAL_SURFACE('',#30766,0.749999999999998,0.785398163397494);
#2967=CONICAL_SURFACE('',#30775,0.35,0.785398163397474);
#2968=CONICAL_SURFACE('',#30778,0.350000000000002,0.785398163397498);
#2969=CONICAL_SURFACE('',#30781,0.350000000000001,0.78539816339749);
#2970=CONICAL_SURFACE('',#30783,0.350000000000001,0.78539816339749);
#2971=FACE_OUTER_BOUND('',#4551,.T.);
#2972=FACE_OUTER_BOUND('',#4552,.T.);
#2973=FACE_OUTER_BOUND('',#4553,.T.);
#2974=FACE_OUTER_BOUND('',#4554,.T.);
#2975=FACE_OUTER_BOUND('',#4555,.T.);
#2976=FACE_OUTER_BOUND('',#4556,.T.);
#2977=FACE_OUTER_BOUND('',#4557,.T.);
#2978=FACE_OUTER_BOUND('',#4558,.T.);
#2979=FACE_OUTER_BOUND('',#4559,.T.);
#2980=FACE_OUTER_BOUND('',#4560,.T.);
#2981=FACE_OUTER_BOUND('',#4561,.T.);
#2982=FACE_OUTER_BOUND('',#4562,.T.);
#2983=FACE_OUTER_BOUND('',#4563,.T.);
#2984=FACE_OUTER_BOUND('',#4564,.T.);
#2985=FACE_OUTER_BOUND('',#4565,.T.);
#2986=FACE_OUTER_BOUND('',#4566,.T.);
#2987=FACE_OUTER_BOUND('',#4571,.T.);
#2988=FACE_OUTER_BOUND('',#4572,.T.);
#2989=FACE_OUTER_BOUND('',#4573,.T.);
#2990=FACE_OUTER_BOUND('',#4574,.T.);
#2991=FACE_OUTER_BOUND('',#4575,.T.);
#2992=FACE_OUTER_BOUND('',#4576,.T.);
#2993=FACE_OUTER_BOUND('',#4577,.T.);
#2994=FACE_OUTER_BOUND('',#4578,.T.);
#2995=FACE_OUTER_BOUND('',#4579,.T.);
#2996=FACE_OUTER_BOUND('',#4584,.T.);
#2997=FACE_OUTER_BOUND('',#4585,.T.);
#2998=FACE_OUTER_BOUND('',#4586,.T.);
#2999=FACE_OUTER_BOUND('',#4587,.T.);
#3000=FACE_OUTER_BOUND('',#4588,.T.);
#3001=FACE_OUTER_BOUND('',#4593,.T.);
#3002=FACE_OUTER_BOUND('',#4594,.T.);
#3003=FACE_OUTER_BOUND('',#4595,.T.);
#3004=FACE_OUTER_BOUND('',#4596,.T.);
#3005=FACE_OUTER_BOUND('',#4597,.T.);
#3006=FACE_OUTER_BOUND('',#4598,.T.);
#3007=FACE_OUTER_BOUND('',#4599,.T.);
#3008=FACE_OUTER_BOUND('',#4600,.T.);
#3009=FACE_OUTER_BOUND('',#4601,.T.);
#3010=FACE_OUTER_BOUND('',#4602,.T.);
#3011=FACE_OUTER_BOUND('',#4603,.T.);
#3012=FACE_OUTER_BOUND('',#4604,.T.);
#3013=FACE_OUTER_BOUND('',#4605,.T.);
#3014=FACE_OUTER_BOUND('',#4606,.T.);
#3015=FACE_OUTER_BOUND('',#4607,.T.);
#3016=FACE_OUTER_BOUND('',#4612,.T.);
#3017=FACE_OUTER_BOUND('',#4613,.T.);
#3018=FACE_OUTER_BOUND('',#4614,.T.);
#3019=FACE_OUTER_BOUND('',#4615,.T.);
#3020=FACE_OUTER_BOUND('',#4616,.T.);
#3021=FACE_OUTER_BOUND('',#4617,.T.);
#3022=FACE_OUTER_BOUND('',#4618,.T.);
#3023=FACE_OUTER_BOUND('',#4619,.T.);
#3024=FACE_OUTER_BOUND('',#4620,.T.);
#3025=FACE_OUTER_BOUND('',#4621,.T.);
#3026=FACE_OUTER_BOUND('',#4622,.T.);
#3027=FACE_OUTER_BOUND('',#4623,.T.);
#3028=FACE_OUTER_BOUND('',#4624,.T.);
#3029=FACE_OUTER_BOUND('',#4625,.T.);
#3030=FACE_OUTER_BOUND('',#4626,.T.);
#3031=FACE_OUTER_BOUND('',#4628,.T.);
#3032=FACE_OUTER_BOUND('',#4629,.T.);
#3033=FACE_OUTER_BOUND('',#4630,.T.);
#3034=FACE_OUTER_BOUND('',#4631,.T.);
#3035=FACE_OUTER_BOUND('',#4632,.T.);
#3036=FACE_OUTER_BOUND('',#4633,.T.);
#3037=FACE_OUTER_BOUND('',#4634,.T.);
#3038=FACE_OUTER_BOUND('',#4635,.T.);
#3039=FACE_OUTER_BOUND('',#4636,.T.);
#3040=FACE_OUTER_BOUND('',#4637,.T.);
#3041=FACE_OUTER_BOUND('',#4643,.T.);
#3042=FACE_OUTER_BOUND('',#4645,.T.);
#3043=FACE_OUTER_BOUND('',#4646,.T.);
#3044=FACE_OUTER_BOUND('',#4647,.T.);
#3045=FACE_OUTER_BOUND('',#4648,.T.);
#3046=FACE_OUTER_BOUND('',#4649,.T.);
#3047=FACE_OUTER_BOUND('',#4650,.T.);
#3048=FACE_OUTER_BOUND('',#4651,.T.);
#3049=FACE_OUTER_BOUND('',#4652,.T.);
#3050=FACE_OUTER_BOUND('',#4653,.T.);
#3051=FACE_OUTER_BOUND('',#4654,.T.);
#3052=FACE_OUTER_BOUND('',#4655,.T.);
#3053=FACE_OUTER_BOUND('',#4656,.T.);
#3054=FACE_OUTER_BOUND('',#4657,.T.);
#3055=FACE_OUTER_BOUND('',#4658,.T.);
#3056=FACE_OUTER_BOUND('',#4659,.T.);
#3057=FACE_OUTER_BOUND('',#4660,.T.);
#3058=FACE_OUTER_BOUND('',#4661,.T.);
#3059=FACE_OUTER_BOUND('',#4662,.T.);
#3060=FACE_OUTER_BOUND('',#4663,.T.);
#3061=FACE_OUTER_BOUND('',#4664,.T.);
#3062=FACE_OUTER_BOUND('',#4665,.T.);
#3063=FACE_OUTER_BOUND('',#4666,.T.);
#3064=FACE_OUTER_BOUND('',#4667,.T.);
#3065=FACE_OUTER_BOUND('',#4668,.T.);
#3066=FACE_OUTER_BOUND('',#4669,.T.);
#3067=FACE_OUTER_BOUND('',#4670,.T.);
#3068=FACE_OUTER_BOUND('',#4671,.T.);
#3069=FACE_OUTER_BOUND('',#4672,.T.);
#3070=FACE_OUTER_BOUND('',#4673,.T.);
#3071=FACE_OUTER_BOUND('',#4674,.T.);
#3072=FACE_OUTER_BOUND('',#4675,.T.);
#3073=FACE_OUTER_BOUND('',#4676,.T.);
#3074=FACE_OUTER_BOUND('',#4677,.T.);
#3075=FACE_OUTER_BOUND('',#4678,.T.);
#3076=FACE_OUTER_BOUND('',#4679,.T.);
#3077=FACE_OUTER_BOUND('',#4680,.T.);
#3078=FACE_OUTER_BOUND('',#4681,.T.);
#3079=FACE_OUTER_BOUND('',#4682,.T.);
#3080=FACE_OUTER_BOUND('',#4683,.T.);
#3081=FACE_OUTER_BOUND('',#4684,.T.);
#3082=FACE_OUTER_BOUND('',#4685,.T.);
#3083=FACE_OUTER_BOUND('',#4686,.T.);
#3084=FACE_OUTER_BOUND('',#4687,.T.);
#3085=FACE_OUTER_BOUND('',#4688,.T.);
#3086=FACE_OUTER_BOUND('',#4689,.T.);
#3087=FACE_OUTER_BOUND('',#4690,.T.);
#3088=FACE_OUTER_BOUND('',#4691,.T.);
#3089=FACE_OUTER_BOUND('',#4692,.T.);
#3090=FACE_OUTER_BOUND('',#4693,.T.);
#3091=FACE_OUTER_BOUND('',#4694,.T.);
#3092=FACE_OUTER_BOUND('',#4695,.T.);
#3093=FACE_OUTER_BOUND('',#4696,.T.);
#3094=FACE_OUTER_BOUND('',#4697,.T.);
#3095=FACE_OUTER_BOUND('',#4698,.T.);
#3096=FACE_OUTER_BOUND('',#4699,.T.);
#3097=FACE_OUTER_BOUND('',#4700,.T.);
#3098=FACE_OUTER_BOUND('',#4701,.T.);
#3099=FACE_OUTER_BOUND('',#4702,.T.);
#3100=FACE_OUTER_BOUND('',#4703,.T.);
#3101=FACE_OUTER_BOUND('',#4704,.T.);
#3102=FACE_OUTER_BOUND('',#4705,.T.);
#3103=FACE_OUTER_BOUND('',#4706,.T.);
#3104=FACE_OUTER_BOUND('',#4707,.T.);
#3105=FACE_OUTER_BOUND('',#4708,.T.);
#3106=FACE_OUTER_BOUND('',#4709,.T.);
#3107=FACE_OUTER_BOUND('',#4710,.T.);
#3108=FACE_OUTER_BOUND('',#4712,.T.);
#3109=FACE_OUTER_BOUND('',#4713,.T.);
#3110=FACE_OUTER_BOUND('',#4714,.T.);
#3111=FACE_OUTER_BOUND('',#4715,.T.);
#3112=FACE_OUTER_BOUND('',#4716,.T.);
#3113=FACE_OUTER_BOUND('',#4717,.T.);
#3114=FACE_OUTER_BOUND('',#4718,.T.);
#3115=FACE_OUTER_BOUND('',#4719,.T.);
#3116=FACE_OUTER_BOUND('',#4720,.T.);
#3117=FACE_OUTER_BOUND('',#4721,.T.);
#3118=FACE_OUTER_BOUND('',#4722,.T.);
#3119=FACE_OUTER_BOUND('',#4723,.T.);
#3120=FACE_OUTER_BOUND('',#4725,.T.);
#3121=FACE_OUTER_BOUND('',#4726,.T.);
#3122=FACE_OUTER_BOUND('',#4727,.T.);
#3123=FACE_OUTER_BOUND('',#4728,.T.);
#3124=FACE_OUTER_BOUND('',#4729,.T.);
#3125=FACE_OUTER_BOUND('',#4730,.T.);
#3126=FACE_OUTER_BOUND('',#4731,.T.);
#3127=FACE_OUTER_BOUND('',#4732,.T.);
#3128=FACE_OUTER_BOUND('',#4733,.T.);
#3129=FACE_OUTER_BOUND('',#4734,.T.);
#3130=FACE_OUTER_BOUND('',#4735,.T.);
#3131=FACE_OUTER_BOUND('',#4736,.T.);
#3132=FACE_OUTER_BOUND('',#4737,.T.);
#3133=FACE_OUTER_BOUND('',#4738,.T.);
#3134=FACE_OUTER_BOUND('',#4739,.T.);
#3135=FACE_OUTER_BOUND('',#4740,.T.);
#3136=FACE_OUTER_BOUND('',#4741,.T.);
#3137=FACE_OUTER_BOUND('',#4742,.T.);
#3138=FACE_OUTER_BOUND('',#4743,.T.);
#3139=FACE_OUTER_BOUND('',#4744,.T.);
#3140=FACE_OUTER_BOUND('',#4745,.T.);
#3141=FACE_OUTER_BOUND('',#4746,.T.);
#3142=FACE_OUTER_BOUND('',#4747,.T.);
#3143=FACE_OUTER_BOUND('',#4748,.T.);
#3144=FACE_OUTER_BOUND('',#4749,.T.);
#3145=FACE_OUTER_BOUND('',#4750,.T.);
#3146=FACE_OUTER_BOUND('',#4751,.T.);
#3147=FACE_OUTER_BOUND('',#4752,.T.);
#3148=FACE_OUTER_BOUND('',#4753,.T.);
#3149=FACE_OUTER_BOUND('',#4754,.T.);
#3150=FACE_OUTER_BOUND('',#4755,.T.);
#3151=FACE_OUTER_BOUND('',#4756,.T.);
#3152=FACE_OUTER_BOUND('',#4757,.T.);
#3153=FACE_OUTER_BOUND('',#4758,.T.);
#3154=FACE_OUTER_BOUND('',#4759,.T.);
#3155=FACE_OUTER_BOUND('',#4760,.T.);
#3156=FACE_OUTER_BOUND('',#4761,.T.);
#3157=FACE_OUTER_BOUND('',#4762,.T.);
#3158=FACE_OUTER_BOUND('',#4763,.T.);
#3159=FACE_OUTER_BOUND('',#4764,.T.);
#3160=FACE_OUTER_BOUND('',#4765,.T.);
#3161=FACE_OUTER_BOUND('',#4766,.T.);
#3162=FACE_OUTER_BOUND('',#4767,.T.);
#3163=FACE_OUTER_BOUND('',#4768,.T.);
#3164=FACE_OUTER_BOUND('',#4769,.T.);
#3165=FACE_OUTER_BOUND('',#4770,.T.);
#3166=FACE_OUTER_BOUND('',#4771,.T.);
#3167=FACE_OUTER_BOUND('',#4772,.T.);
#3168=FACE_OUTER_BOUND('',#4773,.T.);
#3169=FACE_OUTER_BOUND('',#4774,.T.);
#3170=FACE_OUTER_BOUND('',#4775,.T.);
#3171=FACE_OUTER_BOUND('',#4776,.T.);
#3172=FACE_OUTER_BOUND('',#4777,.T.);
#3173=FACE_OUTER_BOUND('',#4778,.T.);
#3174=FACE_OUTER_BOUND('',#4779,.T.);
#3175=FACE_OUTER_BOUND('',#4780,.T.);
#3176=FACE_OUTER_BOUND('',#4781,.T.);
#3177=FACE_OUTER_BOUND('',#4782,.T.);
#3178=FACE_OUTER_BOUND('',#4783,.T.);
#3179=FACE_OUTER_BOUND('',#4784,.T.);
#3180=FACE_OUTER_BOUND('',#4785,.T.);
#3181=FACE_OUTER_BOUND('',#4786,.T.);
#3182=FACE_OUTER_BOUND('',#4789,.T.);
#3183=FACE_OUTER_BOUND('',#4790,.T.);
#3184=FACE_OUTER_BOUND('',#4793,.T.);
#3185=FACE_OUTER_BOUND('',#4794,.T.);
#3186=FACE_OUTER_BOUND('',#4795,.T.);
#3187=FACE_OUTER_BOUND('',#4796,.T.);
#3188=FACE_OUTER_BOUND('',#4797,.T.);
#3189=FACE_OUTER_BOUND('',#4798,.T.);
#3190=FACE_OUTER_BOUND('',#4799,.T.);
#3191=FACE_OUTER_BOUND('',#4800,.T.);
#3192=FACE_OUTER_BOUND('',#4801,.T.);
#3193=FACE_OUTER_BOUND('',#4802,.T.);
#3194=FACE_OUTER_BOUND('',#4803,.T.);
#3195=FACE_OUTER_BOUND('',#4804,.T.);
#3196=FACE_OUTER_BOUND('',#4805,.T.);
#3197=FACE_OUTER_BOUND('',#4806,.T.);
#3198=FACE_OUTER_BOUND('',#4807,.T.);
#3199=FACE_OUTER_BOUND('',#4808,.T.);
#3200=FACE_OUTER_BOUND('',#4809,.T.);
#3201=FACE_OUTER_BOUND('',#4810,.T.);
#3202=FACE_OUTER_BOUND('',#4811,.T.);
#3203=FACE_OUTER_BOUND('',#4812,.T.);
#3204=FACE_OUTER_BOUND('',#4813,.T.);
#3205=FACE_OUTER_BOUND('',#4814,.T.);
#3206=FACE_OUTER_BOUND('',#4816,.T.);
#3207=FACE_OUTER_BOUND('',#4817,.T.);
#3208=FACE_OUTER_BOUND('',#4818,.T.);
#3209=FACE_OUTER_BOUND('',#4819,.T.);
#3210=FACE_OUTER_BOUND('',#4820,.T.);
#3211=FACE_OUTER_BOUND('',#4821,.T.);
#3212=FACE_OUTER_BOUND('',#4822,.T.);
#3213=FACE_OUTER_BOUND('',#4823,.T.);
#3214=FACE_OUTER_BOUND('',#4824,.T.);
#3215=FACE_OUTER_BOUND('',#4825,.T.);
#3216=FACE_OUTER_BOUND('',#4826,.T.);
#3217=FACE_OUTER_BOUND('',#4827,.T.);
#3218=FACE_OUTER_BOUND('',#4828,.T.);
#3219=FACE_OUTER_BOUND('',#4829,.T.);
#3220=FACE_OUTER_BOUND('',#4830,.T.);
#3221=FACE_OUTER_BOUND('',#4831,.T.);
#3222=FACE_OUTER_BOUND('',#4832,.T.);
#3223=FACE_OUTER_BOUND('',#4833,.T.);
#3224=FACE_OUTER_BOUND('',#4834,.T.);
#3225=FACE_OUTER_BOUND('',#4835,.T.);
#3226=FACE_OUTER_BOUND('',#4836,.T.);
#3227=FACE_OUTER_BOUND('',#4837,.T.);
#3228=FACE_OUTER_BOUND('',#4838,.T.);
#3229=FACE_OUTER_BOUND('',#4839,.T.);
#3230=FACE_OUTER_BOUND('',#4840,.T.);
#3231=FACE_OUTER_BOUND('',#4841,.T.);
#3232=FACE_OUTER_BOUND('',#4842,.T.);
#3233=FACE_OUTER_BOUND('',#4843,.T.);
#3234=FACE_OUTER_BOUND('',#4844,.T.);
#3235=FACE_OUTER_BOUND('',#4845,.T.);
#3236=FACE_OUTER_BOUND('',#4846,.T.);
#3237=FACE_OUTER_BOUND('',#4847,.T.);
#3238=FACE_OUTER_BOUND('',#4849,.T.);
#3239=FACE_OUTER_BOUND('',#4850,.T.);
#3240=FACE_OUTER_BOUND('',#4851,.T.);
#3241=FACE_OUTER_BOUND('',#4852,.T.);
#3242=FACE_OUTER_BOUND('',#4853,.T.);
#3243=FACE_OUTER_BOUND('',#4854,.T.);
#3244=FACE_OUTER_BOUND('',#4855,.T.);
#3245=FACE_OUTER_BOUND('',#4856,.T.);
#3246=FACE_OUTER_BOUND('',#4857,.T.);
#3247=FACE_OUTER_BOUND('',#4858,.T.);
#3248=FACE_OUTER_BOUND('',#4859,.T.);
#3249=FACE_OUTER_BOUND('',#4860,.T.);
#3250=FACE_OUTER_BOUND('',#4861,.T.);
#3251=FACE_OUTER_BOUND('',#4862,.T.);
#3252=FACE_OUTER_BOUND('',#4863,.T.);
#3253=FACE_OUTER_BOUND('',#4864,.T.);
#3254=FACE_OUTER_BOUND('',#4865,.T.);
#3255=FACE_OUTER_BOUND('',#4866,.T.);
#3256=FACE_OUTER_BOUND('',#4867,.T.);
#3257=FACE_OUTER_BOUND('',#4868,.T.);
#3258=FACE_OUTER_BOUND('',#4869,.T.);
#3259=FACE_OUTER_BOUND('',#4870,.T.);
#3260=FACE_OUTER_BOUND('',#4871,.T.);
#3261=FACE_OUTER_BOUND('',#4872,.T.);
#3262=FACE_OUTER_BOUND('',#4873,.T.);
#3263=FACE_OUTER_BOUND('',#4874,.T.);
#3264=FACE_OUTER_BOUND('',#4875,.T.);
#3265=FACE_OUTER_BOUND('',#4876,.T.);
#3266=FACE_OUTER_BOUND('',#4877,.T.);
#3267=FACE_OUTER_BOUND('',#4878,.T.);
#3268=FACE_OUTER_BOUND('',#4879,.T.);
#3269=FACE_OUTER_BOUND('',#4880,.T.);
#3270=FACE_OUTER_BOUND('',#4881,.T.);
#3271=FACE_OUTER_BOUND('',#4882,.T.);
#3272=FACE_OUTER_BOUND('',#4883,.T.);
#3273=FACE_OUTER_BOUND('',#4884,.T.);
#3274=FACE_OUTER_BOUND('',#4885,.T.);
#3275=FACE_OUTER_BOUND('',#4886,.T.);
#3276=FACE_OUTER_BOUND('',#4887,.T.);
#3277=FACE_OUTER_BOUND('',#4888,.T.);
#3278=FACE_OUTER_BOUND('',#4889,.T.);
#3279=FACE_OUTER_BOUND('',#4890,.T.);
#3280=FACE_OUTER_BOUND('',#4891,.T.);
#3281=FACE_OUTER_BOUND('',#4892,.T.);
#3282=FACE_OUTER_BOUND('',#4893,.T.);
#3283=FACE_OUTER_BOUND('',#4894,.T.);
#3284=FACE_OUTER_BOUND('',#4895,.T.);
#3285=FACE_OUTER_BOUND('',#4896,.T.);
#3286=FACE_OUTER_BOUND('',#4897,.T.);
#3287=FACE_OUTER_BOUND('',#4898,.T.);
#3288=FACE_OUTER_BOUND('',#4899,.T.);
#3289=FACE_OUTER_BOUND('',#4900,.T.);
#3290=FACE_OUTER_BOUND('',#4901,.T.);
#3291=FACE_OUTER_BOUND('',#4902,.T.);
#3292=FACE_OUTER_BOUND('',#4903,.T.);
#3293=FACE_OUTER_BOUND('',#4904,.T.);
#3294=FACE_OUTER_BOUND('',#4905,.T.);
#3295=FACE_OUTER_BOUND('',#4906,.T.);
#3296=FACE_OUTER_BOUND('',#4907,.T.);
#3297=FACE_OUTER_BOUND('',#4908,.T.);
#3298=FACE_OUTER_BOUND('',#4909,.T.);
#3299=FACE_OUTER_BOUND('',#4910,.T.);
#3300=FACE_OUTER_BOUND('',#4911,.T.);
#3301=FACE_OUTER_BOUND('',#4912,.T.);
#3302=FACE_OUTER_BOUND('',#4913,.T.);
#3303=FACE_OUTER_BOUND('',#4914,.T.);
#3304=FACE_OUTER_BOUND('',#4915,.T.);
#3305=FACE_OUTER_BOUND('',#4916,.T.);
#3306=FACE_OUTER_BOUND('',#4917,.T.);
#3307=FACE_OUTER_BOUND('',#4918,.T.);
#3308=FACE_OUTER_BOUND('',#4919,.T.);
#3309=FACE_OUTER_BOUND('',#4920,.T.);
#3310=FACE_OUTER_BOUND('',#4921,.T.);
#3311=FACE_OUTER_BOUND('',#4922,.T.);
#3312=FACE_OUTER_BOUND('',#4923,.T.);
#3313=FACE_OUTER_BOUND('',#4924,.T.);
#3314=FACE_OUTER_BOUND('',#4925,.T.);
#3315=FACE_OUTER_BOUND('',#4926,.T.);
#3316=FACE_OUTER_BOUND('',#4927,.T.);
#3317=FACE_OUTER_BOUND('',#4928,.T.);
#3318=FACE_OUTER_BOUND('',#4929,.T.);
#3319=FACE_OUTER_BOUND('',#4930,.T.);
#3320=FACE_OUTER_BOUND('',#4931,.T.);
#3321=FACE_OUTER_BOUND('',#4932,.T.);
#3322=FACE_OUTER_BOUND('',#4933,.T.);
#3323=FACE_OUTER_BOUND('',#4934,.T.);
#3324=FACE_OUTER_BOUND('',#4935,.T.);
#3325=FACE_OUTER_BOUND('',#4936,.T.);
#3326=FACE_OUTER_BOUND('',#4937,.T.);
#3327=FACE_OUTER_BOUND('',#4938,.T.);
#3328=FACE_OUTER_BOUND('',#4939,.T.);
#3329=FACE_OUTER_BOUND('',#4940,.T.);
#3330=FACE_OUTER_BOUND('',#4941,.T.);
#3331=FACE_OUTER_BOUND('',#4942,.T.);
#3332=FACE_OUTER_BOUND('',#4943,.T.);
#3333=FACE_OUTER_BOUND('',#4944,.T.);
#3334=FACE_OUTER_BOUND('',#4945,.T.);
#3335=FACE_OUTER_BOUND('',#4946,.T.);
#3336=FACE_OUTER_BOUND('',#4947,.T.);
#3337=FACE_OUTER_BOUND('',#4948,.T.);
#3338=FACE_OUTER_BOUND('',#4949,.T.);
#3339=FACE_OUTER_BOUND('',#4950,.T.);
#3340=FACE_OUTER_BOUND('',#4951,.T.);
#3341=FACE_OUTER_BOUND('',#4952,.T.);
#3342=FACE_OUTER_BOUND('',#4953,.T.);
#3343=FACE_OUTER_BOUND('',#4954,.T.);
#3344=FACE_OUTER_BOUND('',#4955,.T.);
#3345=FACE_OUTER_BOUND('',#4956,.T.);
#3346=FACE_OUTER_BOUND('',#4957,.T.);
#3347=FACE_OUTER_BOUND('',#4958,.T.);
#3348=FACE_OUTER_BOUND('',#4959,.T.);
#3349=FACE_OUTER_BOUND('',#4960,.T.);
#3350=FACE_OUTER_BOUND('',#4961,.T.);
#3351=FACE_OUTER_BOUND('',#4964,.T.);
#3352=FACE_OUTER_BOUND('',#4965,.T.);
#3353=FACE_OUTER_BOUND('',#4966,.T.);
#3354=FACE_OUTER_BOUND('',#4967,.T.);
#3355=FACE_OUTER_BOUND('',#4968,.T.);
#3356=FACE_OUTER_BOUND('',#4969,.T.);
#3357=FACE_OUTER_BOUND('',#4970,.T.);
#3358=FACE_OUTER_BOUND('',#4971,.T.);
#3359=FACE_OUTER_BOUND('',#4972,.T.);
#3360=FACE_OUTER_BOUND('',#4973,.T.);
#3361=FACE_OUTER_BOUND('',#4974,.T.);
#3362=FACE_OUTER_BOUND('',#4975,.T.);
#3363=FACE_OUTER_BOUND('',#4976,.T.);
#3364=FACE_OUTER_BOUND('',#4977,.T.);
#3365=FACE_OUTER_BOUND('',#4978,.T.);
#3366=FACE_OUTER_BOUND('',#4979,.T.);
#3367=FACE_OUTER_BOUND('',#4980,.T.);
#3368=FACE_OUTER_BOUND('',#4981,.T.);
#3369=FACE_OUTER_BOUND('',#4982,.T.);
#3370=FACE_OUTER_BOUND('',#4983,.T.);
#3371=FACE_OUTER_BOUND('',#4984,.T.);
#3372=FACE_OUTER_BOUND('',#4985,.T.);
#3373=FACE_OUTER_BOUND('',#4986,.T.);
#3374=FACE_OUTER_BOUND('',#4987,.T.);
#3375=FACE_OUTER_BOUND('',#4988,.T.);
#3376=FACE_OUTER_BOUND('',#4989,.T.);
#3377=FACE_OUTER_BOUND('',#4990,.T.);
#3378=FACE_OUTER_BOUND('',#4991,.T.);
#3379=FACE_OUTER_BOUND('',#4992,.T.);
#3380=FACE_OUTER_BOUND('',#4993,.T.);
#3381=FACE_OUTER_BOUND('',#4994,.T.);
#3382=FACE_OUTER_BOUND('',#4995,.T.);
#3383=FACE_OUTER_BOUND('',#4996,.T.);
#3384=FACE_OUTER_BOUND('',#4997,.T.);
#3385=FACE_OUTER_BOUND('',#4998,.T.);
#3386=FACE_OUTER_BOUND('',#4999,.T.);
#3387=FACE_OUTER_BOUND('',#5000,.T.);
#3388=FACE_OUTER_BOUND('',#5003,.T.);
#3389=FACE_OUTER_BOUND('',#5004,.T.);
#3390=FACE_OUTER_BOUND('',#5005,.T.);
#3391=FACE_OUTER_BOUND('',#5006,.T.);
#3392=FACE_OUTER_BOUND('',#5007,.T.);
#3393=FACE_OUTER_BOUND('',#5008,.T.);
#3394=FACE_OUTER_BOUND('',#5009,.T.);
#3395=FACE_OUTER_BOUND('',#5011,.T.);
#3396=FACE_OUTER_BOUND('',#5012,.T.);
#3397=FACE_OUTER_BOUND('',#5013,.T.);
#3398=FACE_OUTER_BOUND('',#5014,.T.);
#3399=FACE_OUTER_BOUND('',#5015,.T.);
#3400=FACE_OUTER_BOUND('',#5016,.T.);
#3401=FACE_OUTER_BOUND('',#5017,.T.);
#3402=FACE_OUTER_BOUND('',#5018,.T.);
#3403=FACE_OUTER_BOUND('',#5019,.T.);
#3404=FACE_OUTER_BOUND('',#5020,.T.);
#3405=FACE_OUTER_BOUND('',#5021,.T.);
#3406=FACE_OUTER_BOUND('',#5022,.T.);
#3407=FACE_OUTER_BOUND('',#5023,.T.);
#3408=FACE_OUTER_BOUND('',#5024,.T.);
#3409=FACE_OUTER_BOUND('',#5025,.T.);
#3410=FACE_OUTER_BOUND('',#5026,.T.);
#3411=FACE_OUTER_BOUND('',#5027,.T.);
#3412=FACE_OUTER_BOUND('',#5028,.T.);
#3413=FACE_OUTER_BOUND('',#5029,.T.);
#3414=FACE_OUTER_BOUND('',#5030,.T.);
#3415=FACE_OUTER_BOUND('',#5031,.T.);
#3416=FACE_OUTER_BOUND('',#5032,.T.);
#3417=FACE_OUTER_BOUND('',#5033,.T.);
#3418=FACE_OUTER_BOUND('',#5034,.T.);
#3419=FACE_OUTER_BOUND('',#5035,.T.);
#3420=FACE_OUTER_BOUND('',#5036,.T.);
#3421=FACE_OUTER_BOUND('',#5037,.T.);
#3422=FACE_OUTER_BOUND('',#5038,.T.);
#3423=FACE_OUTER_BOUND('',#5039,.T.);
#3424=FACE_OUTER_BOUND('',#5040,.T.);
#3425=FACE_OUTER_BOUND('',#5041,.T.);
#3426=FACE_OUTER_BOUND('',#5042,.T.);
#3427=FACE_OUTER_BOUND('',#5043,.T.);
#3428=FACE_OUTER_BOUND('',#5044,.T.);
#3429=FACE_OUTER_BOUND('',#5045,.T.);
#3430=FACE_OUTER_BOUND('',#5046,.T.);
#3431=FACE_OUTER_BOUND('',#5047,.T.);
#3432=FACE_OUTER_BOUND('',#5048,.T.);
#3433=FACE_OUTER_BOUND('',#5049,.T.);
#3434=FACE_OUTER_BOUND('',#5050,.T.);
#3435=FACE_OUTER_BOUND('',#5051,.T.);
#3436=FACE_OUTER_BOUND('',#5052,.T.);
#3437=FACE_OUTER_BOUND('',#5053,.T.);
#3438=FACE_OUTER_BOUND('',#5054,.T.);
#3439=FACE_OUTER_BOUND('',#5055,.T.);
#3440=FACE_OUTER_BOUND('',#5056,.T.);
#3441=FACE_OUTER_BOUND('',#5057,.T.);
#3442=FACE_OUTER_BOUND('',#5058,.T.);
#3443=FACE_OUTER_BOUND('',#5059,.T.);
#3444=FACE_OUTER_BOUND('',#5060,.T.);
#3445=FACE_OUTER_BOUND('',#5061,.T.);
#3446=FACE_OUTER_BOUND('',#5062,.T.);
#3447=FACE_OUTER_BOUND('',#5063,.T.);
#3448=FACE_OUTER_BOUND('',#5065,.T.);
#3449=FACE_OUTER_BOUND('',#5066,.T.);
#3450=FACE_OUTER_BOUND('',#5067,.T.);
#3451=FACE_OUTER_BOUND('',#5068,.T.);
#3452=FACE_OUTER_BOUND('',#5069,.T.);
#3453=FACE_OUTER_BOUND('',#5071,.T.);
#3454=FACE_OUTER_BOUND('',#5072,.T.);
#3455=FACE_OUTER_BOUND('',#5073,.T.);
#3456=FACE_OUTER_BOUND('',#5074,.T.);
#3457=FACE_OUTER_BOUND('',#5075,.T.);
#3458=FACE_OUTER_BOUND('',#5076,.T.);
#3459=FACE_OUTER_BOUND('',#5077,.T.);
#3460=FACE_OUTER_BOUND('',#5078,.T.);
#3461=FACE_OUTER_BOUND('',#5079,.T.);
#3462=FACE_OUTER_BOUND('',#5080,.T.);
#3463=FACE_OUTER_BOUND('',#5081,.T.);
#3464=FACE_OUTER_BOUND('',#5082,.T.);
#3465=FACE_OUTER_BOUND('',#5083,.T.);
#3466=FACE_OUTER_BOUND('',#5084,.T.);
#3467=FACE_OUTER_BOUND('',#5085,.T.);
#3468=FACE_OUTER_BOUND('',#5086,.T.);
#3469=FACE_OUTER_BOUND('',#5087,.T.);
#3470=FACE_OUTER_BOUND('',#5088,.T.);
#3471=FACE_OUTER_BOUND('',#5089,.T.);
#3472=FACE_OUTER_BOUND('',#5090,.T.);
#3473=FACE_OUTER_BOUND('',#5092,.T.);
#3474=FACE_OUTER_BOUND('',#5093,.T.);
#3475=FACE_OUTER_BOUND('',#5094,.T.);
#3476=FACE_OUTER_BOUND('',#5095,.T.);
#3477=FACE_OUTER_BOUND('',#5096,.T.);
#3478=FACE_OUTER_BOUND('',#5098,.T.);
#3479=FACE_OUTER_BOUND('',#5099,.T.);
#3480=FACE_OUTER_BOUND('',#5100,.T.);
#3481=FACE_OUTER_BOUND('',#5101,.T.);
#3482=FACE_OUTER_BOUND('',#5102,.T.);
#3483=FACE_OUTER_BOUND('',#5103,.T.);
#3484=FACE_OUTER_BOUND('',#5104,.T.);
#3485=FACE_OUTER_BOUND('',#5105,.T.);
#3486=FACE_OUTER_BOUND('',#5106,.T.);
#3487=FACE_OUTER_BOUND('',#5107,.T.);
#3488=FACE_OUTER_BOUND('',#5108,.T.);
#3489=FACE_OUTER_BOUND('',#5109,.T.);
#3490=FACE_OUTER_BOUND('',#5110,.T.);
#3491=FACE_OUTER_BOUND('',#5111,.T.);
#3492=FACE_OUTER_BOUND('',#5112,.T.);
#3493=FACE_OUTER_BOUND('',#5113,.T.);
#3494=FACE_OUTER_BOUND('',#5114,.T.);
#3495=FACE_OUTER_BOUND('',#5115,.T.);
#3496=FACE_OUTER_BOUND('',#5116,.T.);
#3497=FACE_OUTER_BOUND('',#5117,.T.);
#3498=FACE_OUTER_BOUND('',#5118,.T.);
#3499=FACE_OUTER_BOUND('',#5119,.T.);
#3500=FACE_OUTER_BOUND('',#5120,.T.);
#3501=FACE_OUTER_BOUND('',#5121,.T.);
#3502=FACE_OUTER_BOUND('',#5122,.T.);
#3503=FACE_OUTER_BOUND('',#5123,.T.);
#3504=FACE_OUTER_BOUND('',#5124,.T.);
#3505=FACE_OUTER_BOUND('',#5125,.T.);
#3506=FACE_OUTER_BOUND('',#5126,.T.);
#3507=FACE_OUTER_BOUND('',#5127,.T.);
#3508=FACE_OUTER_BOUND('',#5128,.T.);
#3509=FACE_OUTER_BOUND('',#5129,.T.);
#3510=FACE_OUTER_BOUND('',#5130,.T.);
#3511=FACE_OUTER_BOUND('',#5131,.T.);
#3512=FACE_OUTER_BOUND('',#5132,.T.);
#3513=FACE_OUTER_BOUND('',#5133,.T.);
#3514=FACE_OUTER_BOUND('',#5134,.T.);
#3515=FACE_OUTER_BOUND('',#5137,.T.);
#3516=FACE_OUTER_BOUND('',#5138,.T.);
#3517=FACE_OUTER_BOUND('',#5139,.T.);
#3518=FACE_OUTER_BOUND('',#5142,.T.);
#3519=FACE_OUTER_BOUND('',#5143,.T.);
#3520=FACE_OUTER_BOUND('',#5144,.T.);
#3521=FACE_OUTER_BOUND('',#5145,.T.);
#3522=FACE_OUTER_BOUND('',#5146,.T.);
#3523=FACE_OUTER_BOUND('',#5147,.T.);
#3524=FACE_OUTER_BOUND('',#5148,.T.);
#3525=FACE_OUTER_BOUND('',#5149,.T.);
#3526=FACE_OUTER_BOUND('',#5150,.T.);
#3527=FACE_OUTER_BOUND('',#5151,.T.);
#3528=FACE_OUTER_BOUND('',#5152,.T.);
#3529=FACE_OUTER_BOUND('',#5153,.T.);
#3530=FACE_OUTER_BOUND('',#5154,.T.);
#3531=FACE_OUTER_BOUND('',#5155,.T.);
#3532=FACE_OUTER_BOUND('',#5156,.T.);
#3533=FACE_OUTER_BOUND('',#5157,.T.);
#3534=FACE_OUTER_BOUND('',#5158,.T.);
#3535=FACE_OUTER_BOUND('',#5159,.T.);
#3536=FACE_OUTER_BOUND('',#5160,.T.);
#3537=FACE_OUTER_BOUND('',#5161,.T.);
#3538=FACE_OUTER_BOUND('',#5162,.T.);
#3539=FACE_OUTER_BOUND('',#5163,.T.);
#3540=FACE_OUTER_BOUND('',#5164,.T.);
#3541=FACE_OUTER_BOUND('',#5165,.T.);
#3542=FACE_OUTER_BOUND('',#5166,.T.);
#3543=FACE_OUTER_BOUND('',#5167,.T.);
#3544=FACE_OUTER_BOUND('',#5168,.T.);
#3545=FACE_OUTER_BOUND('',#5169,.T.);
#3546=FACE_OUTER_BOUND('',#5170,.T.);
#3547=FACE_OUTER_BOUND('',#5171,.T.);
#3548=FACE_OUTER_BOUND('',#5172,.T.);
#3549=FACE_OUTER_BOUND('',#5173,.T.);
#3550=FACE_OUTER_BOUND('',#5177,.T.);
#3551=FACE_OUTER_BOUND('',#5178,.T.);
#3552=FACE_OUTER_BOUND('',#5179,.T.);
#3553=FACE_OUTER_BOUND('',#5180,.T.);
#3554=FACE_OUTER_BOUND('',#5181,.T.);
#3555=FACE_OUTER_BOUND('',#5182,.T.);
#3556=FACE_OUTER_BOUND('',#5183,.T.);
#3557=FACE_OUTER_BOUND('',#5184,.T.);
#3558=FACE_OUTER_BOUND('',#5185,.T.);
#3559=FACE_OUTER_BOUND('',#5186,.T.);
#3560=FACE_OUTER_BOUND('',#5187,.T.);
#3561=FACE_OUTER_BOUND('',#5188,.T.);
#3562=FACE_OUTER_BOUND('',#5189,.T.);
#3563=FACE_OUTER_BOUND('',#5190,.T.);
#3564=FACE_OUTER_BOUND('',#5191,.T.);
#3565=FACE_OUTER_BOUND('',#5193,.T.);
#3566=FACE_OUTER_BOUND('',#5194,.T.);
#3567=FACE_OUTER_BOUND('',#5195,.T.);
#3568=FACE_OUTER_BOUND('',#5196,.T.);
#3569=FACE_OUTER_BOUND('',#5197,.T.);
#3570=FACE_OUTER_BOUND('',#5198,.T.);
#3571=FACE_OUTER_BOUND('',#5199,.T.);
#3572=FACE_OUTER_BOUND('',#5200,.T.);
#3573=FACE_OUTER_BOUND('',#5201,.T.);
#3574=FACE_OUTER_BOUND('',#5202,.T.);
#3575=FACE_OUTER_BOUND('',#5203,.T.);
#3576=FACE_OUTER_BOUND('',#5204,.T.);
#3577=FACE_OUTER_BOUND('',#5205,.T.);
#3578=FACE_OUTER_BOUND('',#5206,.T.);
#3579=FACE_OUTER_BOUND('',#5207,.T.);
#3580=FACE_OUTER_BOUND('',#5209,.T.);
#3581=FACE_OUTER_BOUND('',#5210,.T.);
#3582=FACE_OUTER_BOUND('',#5211,.T.);
#3583=FACE_OUTER_BOUND('',#5212,.T.);
#3584=FACE_OUTER_BOUND('',#5213,.T.);
#3585=FACE_OUTER_BOUND('',#5214,.T.);
#3586=FACE_OUTER_BOUND('',#5216,.T.);
#3587=FACE_OUTER_BOUND('',#5217,.T.);
#3588=FACE_OUTER_BOUND('',#5218,.T.);
#3589=FACE_OUTER_BOUND('',#5219,.T.);
#3590=FACE_OUTER_BOUND('',#5220,.T.);
#3591=FACE_OUTER_BOUND('',#5221,.T.);
#3592=FACE_OUTER_BOUND('',#5222,.T.);
#3593=FACE_OUTER_BOUND('',#5223,.T.);
#3594=FACE_OUTER_BOUND('',#5224,.T.);
#3595=FACE_OUTER_BOUND('',#5225,.T.);
#3596=FACE_OUTER_BOUND('',#5226,.T.);
#3597=FACE_OUTER_BOUND('',#5227,.T.);
#3598=FACE_OUTER_BOUND('',#5228,.T.);
#3599=FACE_OUTER_BOUND('',#5230,.T.);
#3600=FACE_OUTER_BOUND('',#5231,.T.);
#3601=FACE_OUTER_BOUND('',#5232,.T.);
#3602=FACE_OUTER_BOUND('',#5233,.T.);
#3603=FACE_OUTER_BOUND('',#5234,.T.);
#3604=FACE_OUTER_BOUND('',#5235,.T.);
#3605=FACE_OUTER_BOUND('',#5236,.T.);
#3606=FACE_OUTER_BOUND('',#5237,.T.);
#3607=FACE_OUTER_BOUND('',#5238,.T.);
#3608=FACE_OUTER_BOUND('',#5239,.T.);
#3609=FACE_OUTER_BOUND('',#5240,.T.);
#3610=FACE_OUTER_BOUND('',#5241,.T.);
#3611=FACE_OUTER_BOUND('',#5242,.T.);
#3612=FACE_OUTER_BOUND('',#5243,.T.);
#3613=FACE_OUTER_BOUND('',#5244,.T.);
#3614=FACE_OUTER_BOUND('',#5245,.T.);
#3615=FACE_OUTER_BOUND('',#5246,.T.);
#3616=FACE_OUTER_BOUND('',#5247,.T.);
#3617=FACE_OUTER_BOUND('',#5248,.T.);
#3618=FACE_OUTER_BOUND('',#5249,.T.);
#3619=FACE_OUTER_BOUND('',#5250,.T.);
#3620=FACE_OUTER_BOUND('',#5251,.T.);
#3621=FACE_OUTER_BOUND('',#5252,.T.);
#3622=FACE_OUTER_BOUND('',#5253,.T.);
#3623=FACE_OUTER_BOUND('',#5255,.T.);
#3624=FACE_OUTER_BOUND('',#5256,.T.);
#3625=FACE_OUTER_BOUND('',#5257,.T.);
#3626=FACE_OUTER_BOUND('',#5258,.T.);
#3627=FACE_OUTER_BOUND('',#5259,.T.);
#3628=FACE_OUTER_BOUND('',#5261,.T.);
#3629=FACE_OUTER_BOUND('',#5263,.T.);
#3630=FACE_OUTER_BOUND('',#5264,.T.);
#3631=FACE_OUTER_BOUND('',#5265,.T.);
#3632=FACE_OUTER_BOUND('',#5266,.T.);
#3633=FACE_OUTER_BOUND('',#5267,.T.);
#3634=FACE_OUTER_BOUND('',#5268,.T.);
#3635=FACE_OUTER_BOUND('',#5269,.T.);
#3636=FACE_OUTER_BOUND('',#5270,.T.);
#3637=FACE_OUTER_BOUND('',#5271,.T.);
#3638=FACE_OUTER_BOUND('',#5272,.T.);
#3639=FACE_OUTER_BOUND('',#5273,.T.);
#3640=FACE_OUTER_BOUND('',#5274,.T.);
#3641=FACE_OUTER_BOUND('',#5275,.T.);
#3642=FACE_OUTER_BOUND('',#5276,.T.);
#3643=FACE_OUTER_BOUND('',#5277,.T.);
#3644=FACE_OUTER_BOUND('',#5278,.T.);
#3645=FACE_OUTER_BOUND('',#5279,.T.);
#3646=FACE_OUTER_BOUND('',#5280,.T.);
#3647=FACE_OUTER_BOUND('',#5281,.T.);
#3648=FACE_OUTER_BOUND('',#5282,.T.);
#3649=FACE_OUTER_BOUND('',#5283,.T.);
#3650=FACE_OUTER_BOUND('',#5284,.T.);
#3651=FACE_OUTER_BOUND('',#5285,.T.);
#3652=FACE_OUTER_BOUND('',#5286,.T.);
#3653=FACE_OUTER_BOUND('',#5287,.T.);
#3654=FACE_OUTER_BOUND('',#5288,.T.);
#3655=FACE_OUTER_BOUND('',#5289,.T.);
#3656=FACE_OUTER_BOUND('',#5290,.T.);
#3657=FACE_OUTER_BOUND('',#5291,.T.);
#3658=FACE_OUTER_BOUND('',#5292,.T.);
#3659=FACE_OUTER_BOUND('',#5293,.T.);
#3660=FACE_OUTER_BOUND('',#5294,.T.);
#3661=FACE_OUTER_BOUND('',#5295,.T.);
#3662=FACE_OUTER_BOUND('',#5296,.T.);
#3663=FACE_OUTER_BOUND('',#5297,.T.);
#3664=FACE_OUTER_BOUND('',#5298,.T.);
#3665=FACE_OUTER_BOUND('',#5299,.T.);
#3666=FACE_OUTER_BOUND('',#5300,.T.);
#3667=FACE_OUTER_BOUND('',#5301,.T.);
#3668=FACE_OUTER_BOUND('',#5302,.T.);
#3669=FACE_OUTER_BOUND('',#5303,.T.);
#3670=FACE_OUTER_BOUND('',#5304,.T.);
#3671=FACE_OUTER_BOUND('',#5305,.T.);
#3672=FACE_OUTER_BOUND('',#5306,.T.);
#3673=FACE_OUTER_BOUND('',#5307,.T.);
#3674=FACE_OUTER_BOUND('',#5308,.T.);
#3675=FACE_OUTER_BOUND('',#5309,.T.);
#3676=FACE_OUTER_BOUND('',#5310,.T.);
#3677=FACE_OUTER_BOUND('',#5311,.T.);
#3678=FACE_OUTER_BOUND('',#5312,.T.);
#3679=FACE_OUTER_BOUND('',#5313,.T.);
#3680=FACE_OUTER_BOUND('',#5314,.T.);
#3681=FACE_OUTER_BOUND('',#5315,.T.);
#3682=FACE_OUTER_BOUND('',#5316,.T.);
#3683=FACE_OUTER_BOUND('',#5317,.T.);
#3684=FACE_OUTER_BOUND('',#5318,.T.);
#3685=FACE_OUTER_BOUND('',#5319,.T.);
#3686=FACE_OUTER_BOUND('',#5320,.T.);
#3687=FACE_OUTER_BOUND('',#5321,.T.);
#3688=FACE_OUTER_BOUND('',#5322,.T.);
#3689=FACE_OUTER_BOUND('',#5323,.T.);
#3690=FACE_OUTER_BOUND('',#5324,.T.);
#3691=FACE_OUTER_BOUND('',#5325,.T.);
#3692=FACE_OUTER_BOUND('',#5326,.T.);
#3693=FACE_OUTER_BOUND('',#5327,.T.);
#3694=FACE_OUTER_BOUND('',#5328,.T.);
#3695=FACE_OUTER_BOUND('',#5329,.T.);
#3696=FACE_OUTER_BOUND('',#5330,.T.);
#3697=FACE_OUTER_BOUND('',#5331,.T.);
#3698=FACE_OUTER_BOUND('',#5332,.T.);
#3699=FACE_OUTER_BOUND('',#5333,.T.);
#3700=FACE_OUTER_BOUND('',#5334,.T.);
#3701=FACE_OUTER_BOUND('',#5335,.T.);
#3702=FACE_OUTER_BOUND('',#5336,.T.);
#3703=FACE_OUTER_BOUND('',#5337,.T.);
#3704=FACE_OUTER_BOUND('',#5338,.T.);
#3705=FACE_OUTER_BOUND('',#5339,.T.);
#3706=FACE_OUTER_BOUND('',#5340,.T.);
#3707=FACE_OUTER_BOUND('',#5341,.T.);
#3708=FACE_OUTER_BOUND('',#5342,.T.);
#3709=FACE_OUTER_BOUND('',#5343,.T.);
#3710=FACE_OUTER_BOUND('',#5344,.T.);
#3711=FACE_OUTER_BOUND('',#5345,.T.);
#3712=FACE_OUTER_BOUND('',#5346,.T.);
#3713=FACE_OUTER_BOUND('',#5347,.T.);
#3714=FACE_OUTER_BOUND('',#5348,.T.);
#3715=FACE_OUTER_BOUND('',#5349,.T.);
#3716=FACE_OUTER_BOUND('',#5350,.T.);
#3717=FACE_OUTER_BOUND('',#5351,.T.);
#3718=FACE_OUTER_BOUND('',#5352,.T.);
#3719=FACE_OUTER_BOUND('',#5353,.T.);
#3720=FACE_OUTER_BOUND('',#5354,.T.);
#3721=FACE_OUTER_BOUND('',#5355,.T.);
#3722=FACE_OUTER_BOUND('',#5356,.T.);
#3723=FACE_OUTER_BOUND('',#5357,.T.);
#3724=FACE_OUTER_BOUND('',#5358,.T.);
#3725=FACE_OUTER_BOUND('',#5359,.T.);
#3726=FACE_OUTER_BOUND('',#5360,.T.);
#3727=FACE_OUTER_BOUND('',#5361,.T.);
#3728=FACE_OUTER_BOUND('',#5362,.T.);
#3729=FACE_OUTER_BOUND('',#5363,.T.);
#3730=FACE_OUTER_BOUND('',#5364,.T.);
#3731=FACE_OUTER_BOUND('',#5365,.T.);
#3732=FACE_OUTER_BOUND('',#5366,.T.);
#3733=FACE_OUTER_BOUND('',#5367,.T.);
#3734=FACE_OUTER_BOUND('',#5368,.T.);
#3735=FACE_OUTER_BOUND('',#5369,.T.);
#3736=FACE_OUTER_BOUND('',#5370,.T.);
#3737=FACE_OUTER_BOUND('',#5371,.T.);
#3738=FACE_OUTER_BOUND('',#5372,.T.);
#3739=FACE_OUTER_BOUND('',#5373,.T.);
#3740=FACE_OUTER_BOUND('',#5374,.T.);
#3741=FACE_OUTER_BOUND('',#5375,.T.);
#3742=FACE_OUTER_BOUND('',#5376,.T.);
#3743=FACE_OUTER_BOUND('',#5377,.T.);
#3744=FACE_OUTER_BOUND('',#5378,.T.);
#3745=FACE_OUTER_BOUND('',#5379,.T.);
#3746=FACE_OUTER_BOUND('',#5380,.T.);
#3747=FACE_OUTER_BOUND('',#5381,.T.);
#3748=FACE_OUTER_BOUND('',#5382,.T.);
#3749=FACE_OUTER_BOUND('',#5383,.T.);
#3750=FACE_OUTER_BOUND('',#5384,.T.);
#3751=FACE_OUTER_BOUND('',#5385,.T.);
#3752=FACE_OUTER_BOUND('',#5386,.T.);
#3753=FACE_OUTER_BOUND('',#5387,.T.);
#3754=FACE_OUTER_BOUND('',#5388,.T.);
#3755=FACE_OUTER_BOUND('',#5389,.T.);
#3756=FACE_OUTER_BOUND('',#5390,.T.);
#3757=FACE_OUTER_BOUND('',#5391,.T.);
#3758=FACE_OUTER_BOUND('',#5392,.T.);
#3759=FACE_OUTER_BOUND('',#5393,.T.);
#3760=FACE_OUTER_BOUND('',#5394,.T.);
#3761=FACE_OUTER_BOUND('',#5396,.T.);
#3762=FACE_OUTER_BOUND('',#5398,.T.);
#3763=FACE_OUTER_BOUND('',#5399,.T.);
#3764=FACE_OUTER_BOUND('',#5400,.T.);
#3765=FACE_OUTER_BOUND('',#5401,.T.);
#3766=FACE_OUTER_BOUND('',#5402,.T.);
#3767=FACE_OUTER_BOUND('',#5403,.T.);
#3768=FACE_OUTER_BOUND('',#5404,.T.);
#3769=FACE_OUTER_BOUND('',#5405,.T.);
#3770=FACE_OUTER_BOUND('',#5406,.T.);
#3771=FACE_OUTER_BOUND('',#5407,.T.);
#3772=FACE_OUTER_BOUND('',#5408,.T.);
#3773=FACE_OUTER_BOUND('',#5409,.T.);
#3774=FACE_OUTER_BOUND('',#5410,.T.);
#3775=FACE_OUTER_BOUND('',#5411,.T.);
#3776=FACE_OUTER_BOUND('',#5412,.T.);
#3777=FACE_OUTER_BOUND('',#5413,.T.);
#3778=FACE_OUTER_BOUND('',#5414,.T.);
#3779=FACE_OUTER_BOUND('',#5415,.T.);
#3780=FACE_OUTER_BOUND('',#5416,.T.);
#3781=FACE_OUTER_BOUND('',#5417,.T.);
#3782=FACE_OUTER_BOUND('',#5418,.T.);
#3783=FACE_OUTER_BOUND('',#5419,.T.);
#3784=FACE_OUTER_BOUND('',#5420,.T.);
#3785=FACE_OUTER_BOUND('',#5421,.T.);
#3786=FACE_OUTER_BOUND('',#5422,.T.);
#3787=FACE_OUTER_BOUND('',#5423,.T.);
#3788=FACE_OUTER_BOUND('',#5424,.T.);
#3789=FACE_OUTER_BOUND('',#5425,.T.);
#3790=FACE_OUTER_BOUND('',#5426,.T.);
#3791=FACE_OUTER_BOUND('',#5427,.T.);
#3792=FACE_OUTER_BOUND('',#5428,.T.);
#3793=FACE_OUTER_BOUND('',#5429,.T.);
#3794=FACE_OUTER_BOUND('',#5430,.T.);
#3795=FACE_OUTER_BOUND('',#5431,.T.);
#3796=FACE_OUTER_BOUND('',#5432,.T.);
#3797=FACE_OUTER_BOUND('',#5433,.T.);
#3798=FACE_OUTER_BOUND('',#5434,.T.);
#3799=FACE_OUTER_BOUND('',#5435,.T.);
#3800=FACE_OUTER_BOUND('',#5436,.T.);
#3801=FACE_OUTER_BOUND('',#5437,.T.);
#3802=FACE_OUTER_BOUND('',#5438,.T.);
#3803=FACE_OUTER_BOUND('',#5439,.T.);
#3804=FACE_OUTER_BOUND('',#5440,.T.);
#3805=FACE_OUTER_BOUND('',#5441,.T.);
#3806=FACE_OUTER_BOUND('',#5442,.T.);
#3807=FACE_OUTER_BOUND('',#5443,.T.);
#3808=FACE_OUTER_BOUND('',#5444,.T.);
#3809=FACE_OUTER_BOUND('',#5445,.T.);
#3810=FACE_OUTER_BOUND('',#5446,.T.);
#3811=FACE_OUTER_BOUND('',#5447,.T.);
#3812=FACE_OUTER_BOUND('',#5448,.T.);
#3813=FACE_OUTER_BOUND('',#5449,.T.);
#3814=FACE_OUTER_BOUND('',#5450,.T.);
#3815=FACE_OUTER_BOUND('',#5451,.T.);
#3816=FACE_OUTER_BOUND('',#5452,.T.);
#3817=FACE_OUTER_BOUND('',#5453,.T.);
#3818=FACE_OUTER_BOUND('',#5454,.T.);
#3819=FACE_OUTER_BOUND('',#5455,.T.);
#3820=FACE_OUTER_BOUND('',#5456,.T.);
#3821=FACE_OUTER_BOUND('',#5457,.T.);
#3822=FACE_OUTER_BOUND('',#5458,.T.);
#3823=FACE_OUTER_BOUND('',#5459,.T.);
#3824=FACE_OUTER_BOUND('',#5460,.T.);
#3825=FACE_OUTER_BOUND('',#5461,.T.);
#3826=FACE_OUTER_BOUND('',#5462,.T.);
#3827=FACE_OUTER_BOUND('',#5463,.T.);
#3828=FACE_OUTER_BOUND('',#5464,.T.);
#3829=FACE_OUTER_BOUND('',#5465,.T.);
#3830=FACE_OUTER_BOUND('',#5466,.T.);
#3831=FACE_OUTER_BOUND('',#5467,.T.);
#3832=FACE_OUTER_BOUND('',#5468,.T.);
#3833=FACE_OUTER_BOUND('',#5469,.T.);
#3834=FACE_OUTER_BOUND('',#5470,.T.);
#3835=FACE_OUTER_BOUND('',#5471,.T.);
#3836=FACE_OUTER_BOUND('',#5472,.T.);
#3837=FACE_OUTER_BOUND('',#5473,.T.);
#3838=FACE_OUTER_BOUND('',#5474,.T.);
#3839=FACE_OUTER_BOUND('',#5475,.T.);
#3840=FACE_OUTER_BOUND('',#5476,.T.);
#3841=FACE_OUTER_BOUND('',#5477,.T.);
#3842=FACE_OUTER_BOUND('',#5478,.T.);
#3843=FACE_OUTER_BOUND('',#5479,.T.);
#3844=FACE_OUTER_BOUND('',#5480,.T.);
#3845=FACE_OUTER_BOUND('',#5481,.T.);
#3846=FACE_OUTER_BOUND('',#5482,.T.);
#3847=FACE_OUTER_BOUND('',#5483,.T.);
#3848=FACE_OUTER_BOUND('',#5484,.T.);
#3849=FACE_OUTER_BOUND('',#5485,.T.);
#3850=FACE_OUTER_BOUND('',#5486,.T.);
#3851=FACE_OUTER_BOUND('',#5487,.T.);
#3852=FACE_OUTER_BOUND('',#5488,.T.);
#3853=FACE_OUTER_BOUND('',#5489,.T.);
#3854=FACE_OUTER_BOUND('',#5490,.T.);
#3855=FACE_OUTER_BOUND('',#5491,.T.);
#3856=FACE_OUTER_BOUND('',#5492,.T.);
#3857=FACE_OUTER_BOUND('',#5493,.T.);
#3858=FACE_OUTER_BOUND('',#5495,.T.);
#3859=FACE_OUTER_BOUND('',#5496,.T.);
#3860=FACE_OUTER_BOUND('',#5497,.T.);
#3861=FACE_OUTER_BOUND('',#5498,.T.);
#3862=FACE_OUTER_BOUND('',#5499,.T.);
#3863=FACE_OUTER_BOUND('',#5500,.T.);
#3864=FACE_OUTER_BOUND('',#5502,.T.);
#3865=FACE_OUTER_BOUND('',#5503,.T.);
#3866=FACE_OUTER_BOUND('',#5504,.T.);
#3867=FACE_OUTER_BOUND('',#5505,.T.);
#3868=FACE_OUTER_BOUND('',#5506,.T.);
#3869=FACE_OUTER_BOUND('',#5507,.T.);
#3870=FACE_OUTER_BOUND('',#5508,.T.);
#3871=FACE_OUTER_BOUND('',#5510,.T.);
#3872=FACE_OUTER_BOUND('',#5511,.T.);
#3873=FACE_OUTER_BOUND('',#5512,.T.);
#3874=FACE_OUTER_BOUND('',#5513,.T.);
#3875=FACE_OUTER_BOUND('',#5514,.T.);
#3876=FACE_OUTER_BOUND('',#5515,.T.);
#3877=FACE_OUTER_BOUND('',#5516,.T.);
#3878=FACE_OUTER_BOUND('',#5517,.T.);
#3879=FACE_OUTER_BOUND('',#5518,.T.);
#3880=FACE_OUTER_BOUND('',#5519,.T.);
#3881=FACE_OUTER_BOUND('',#5520,.T.);
#3882=FACE_OUTER_BOUND('',#5521,.T.);
#3883=FACE_OUTER_BOUND('',#5522,.T.);
#3884=FACE_OUTER_BOUND('',#5523,.T.);
#3885=FACE_OUTER_BOUND('',#5524,.T.);
#3886=FACE_OUTER_BOUND('',#5525,.T.);
#3887=FACE_OUTER_BOUND('',#5526,.T.);
#3888=FACE_OUTER_BOUND('',#5527,.T.);
#3889=FACE_OUTER_BOUND('',#5528,.T.);
#3890=FACE_OUTER_BOUND('',#5529,.T.);
#3891=FACE_OUTER_BOUND('',#5530,.T.);
#3892=FACE_OUTER_BOUND('',#5531,.T.);
#3893=FACE_OUTER_BOUND('',#5532,.T.);
#3894=FACE_OUTER_BOUND('',#5533,.T.);
#3895=FACE_OUTER_BOUND('',#5534,.T.);
#3896=FACE_OUTER_BOUND('',#5535,.T.);
#3897=FACE_OUTER_BOUND('',#5536,.T.);
#3898=FACE_OUTER_BOUND('',#5537,.T.);
#3899=FACE_OUTER_BOUND('',#5538,.T.);
#3900=FACE_OUTER_BOUND('',#5539,.T.);
#3901=FACE_OUTER_BOUND('',#5540,.T.);
#3902=FACE_OUTER_BOUND('',#5541,.T.);
#3903=FACE_OUTER_BOUND('',#5542,.T.);
#3904=FACE_OUTER_BOUND('',#5543,.T.);
#3905=FACE_OUTER_BOUND('',#5544,.T.);
#3906=FACE_OUTER_BOUND('',#5545,.T.);
#3907=FACE_OUTER_BOUND('',#5546,.T.);
#3908=FACE_OUTER_BOUND('',#5547,.T.);
#3909=FACE_OUTER_BOUND('',#5548,.T.);
#3910=FACE_OUTER_BOUND('',#5549,.T.);
#3911=FACE_OUTER_BOUND('',#5550,.T.);
#3912=FACE_OUTER_BOUND('',#5551,.T.);
#3913=FACE_OUTER_BOUND('',#5552,.T.);
#3914=FACE_OUTER_BOUND('',#5553,.T.);
#3915=FACE_OUTER_BOUND('',#5554,.T.);
#3916=FACE_OUTER_BOUND('',#5555,.T.);
#3917=FACE_OUTER_BOUND('',#5556,.T.);
#3918=FACE_OUTER_BOUND('',#5557,.T.);
#3919=FACE_OUTER_BOUND('',#5558,.T.);
#3920=FACE_OUTER_BOUND('',#5559,.T.);
#3921=FACE_OUTER_BOUND('',#5560,.T.);
#3922=FACE_OUTER_BOUND('',#5561,.T.);
#3923=FACE_OUTER_BOUND('',#5562,.T.);
#3924=FACE_OUTER_BOUND('',#5563,.T.);
#3925=FACE_OUTER_BOUND('',#5564,.T.);
#3926=FACE_OUTER_BOUND('',#5565,.T.);
#3927=FACE_OUTER_BOUND('',#5566,.T.);
#3928=FACE_OUTER_BOUND('',#5567,.T.);
#3929=FACE_OUTER_BOUND('',#5568,.T.);
#3930=FACE_OUTER_BOUND('',#5569,.T.);
#3931=FACE_OUTER_BOUND('',#5570,.T.);
#3932=FACE_OUTER_BOUND('',#5571,.T.);
#3933=FACE_OUTER_BOUND('',#5572,.T.);
#3934=FACE_OUTER_BOUND('',#5573,.T.);
#3935=FACE_OUTER_BOUND('',#5574,.T.);
#3936=FACE_OUTER_BOUND('',#5575,.T.);
#3937=FACE_OUTER_BOUND('',#5576,.T.);
#3938=FACE_OUTER_BOUND('',#5589,.T.);
#3939=FACE_OUTER_BOUND('',#5590,.T.);
#3940=FACE_OUTER_BOUND('',#5591,.T.);
#3941=FACE_OUTER_BOUND('',#5592,.T.);
#3942=FACE_OUTER_BOUND('',#5594,.T.);
#3943=FACE_OUTER_BOUND('',#5596,.T.);
#3944=FACE_OUTER_BOUND('',#5597,.T.);
#3945=FACE_OUTER_BOUND('',#5598,.T.);
#3946=FACE_OUTER_BOUND('',#5600,.T.);
#3947=FACE_OUTER_BOUND('',#5601,.T.);
#3948=FACE_OUTER_BOUND('',#5602,.T.);
#3949=FACE_OUTER_BOUND('',#5605,.T.);
#3950=FACE_OUTER_BOUND('',#5606,.T.);
#3951=FACE_OUTER_BOUND('',#5608,.T.);
#3952=FACE_OUTER_BOUND('',#5609,.T.);
#3953=FACE_OUTER_BOUND('',#5610,.T.);
#3954=FACE_OUTER_BOUND('',#5611,.T.);
#3955=FACE_OUTER_BOUND('',#5613,.T.);
#3956=FACE_OUTER_BOUND('',#5614,.T.);
#3957=FACE_OUTER_BOUND('',#5615,.T.);
#3958=FACE_OUTER_BOUND('',#5616,.T.);
#3959=FACE_OUTER_BOUND('',#5618,.T.);
#3960=FACE_OUTER_BOUND('',#5619,.T.);
#3961=FACE_OUTER_BOUND('',#5620,.T.);
#3962=FACE_OUTER_BOUND('',#5621,.T.);
#3963=FACE_OUTER_BOUND('',#5622,.T.);
#3964=FACE_OUTER_BOUND('',#5623,.T.);
#3965=FACE_OUTER_BOUND('',#5624,.T.);
#3966=FACE_OUTER_BOUND('',#5625,.T.);
#3967=FACE_OUTER_BOUND('',#5626,.T.);
#3968=FACE_OUTER_BOUND('',#5627,.T.);
#3969=FACE_OUTER_BOUND('',#5628,.T.);
#3970=FACE_OUTER_BOUND('',#5629,.T.);
#3971=FACE_OUTER_BOUND('',#5630,.T.);
#3972=FACE_OUTER_BOUND('',#5631,.T.);
#3973=FACE_OUTER_BOUND('',#5632,.T.);
#3974=FACE_OUTER_BOUND('',#5633,.T.);
#3975=FACE_OUTER_BOUND('',#5634,.T.);
#3976=FACE_OUTER_BOUND('',#5635,.T.);
#3977=FACE_OUTER_BOUND('',#5636,.T.);
#3978=FACE_OUTER_BOUND('',#5637,.T.);
#3979=FACE_OUTER_BOUND('',#5638,.T.);
#3980=FACE_OUTER_BOUND('',#5639,.T.);
#3981=FACE_OUTER_BOUND('',#5640,.T.);
#3982=FACE_OUTER_BOUND('',#5641,.T.);
#3983=FACE_OUTER_BOUND('',#5642,.T.);
#3984=FACE_OUTER_BOUND('',#5643,.T.);
#3985=FACE_OUTER_BOUND('',#5644,.T.);
#3986=FACE_OUTER_BOUND('',#5645,.T.);
#3987=FACE_OUTER_BOUND('',#5646,.T.);
#3988=FACE_OUTER_BOUND('',#5647,.T.);
#3989=FACE_OUTER_BOUND('',#5648,.T.);
#3990=FACE_OUTER_BOUND('',#5649,.T.);
#3991=FACE_OUTER_BOUND('',#5650,.T.);
#3992=FACE_OUTER_BOUND('',#5651,.T.);
#3993=FACE_OUTER_BOUND('',#5652,.T.);
#3994=FACE_OUTER_BOUND('',#5653,.T.);
#3995=FACE_OUTER_BOUND('',#5654,.T.);
#3996=FACE_OUTER_BOUND('',#5655,.T.);
#3997=FACE_OUTER_BOUND('',#5656,.T.);
#3998=FACE_OUTER_BOUND('',#5657,.T.);
#3999=FACE_OUTER_BOUND('',#5658,.T.);
#4000=FACE_OUTER_BOUND('',#5659,.T.);
#4001=FACE_OUTER_BOUND('',#5660,.T.);
#4002=FACE_OUTER_BOUND('',#5661,.T.);
#4003=FACE_OUTER_BOUND('',#5662,.T.);
#4004=FACE_OUTER_BOUND('',#5663,.T.);
#4005=FACE_OUTER_BOUND('',#5664,.T.);
#4006=FACE_OUTER_BOUND('',#5665,.T.);
#4007=FACE_OUTER_BOUND('',#5666,.T.);
#4008=FACE_OUTER_BOUND('',#5667,.T.);
#4009=FACE_OUTER_BOUND('',#5668,.T.);
#4010=FACE_OUTER_BOUND('',#5669,.T.);
#4011=FACE_OUTER_BOUND('',#5672,.T.);
#4012=FACE_OUTER_BOUND('',#5673,.T.);
#4013=FACE_OUTER_BOUND('',#5674,.T.);
#4014=FACE_OUTER_BOUND('',#5675,.T.);
#4015=FACE_OUTER_BOUND('',#5676,.T.);
#4016=FACE_OUTER_BOUND('',#5679,.T.);
#4017=FACE_OUTER_BOUND('',#5680,.T.);
#4018=FACE_OUTER_BOUND('',#5681,.T.);
#4019=FACE_OUTER_BOUND('',#5682,.T.);
#4020=FACE_OUTER_BOUND('',#5683,.T.);
#4021=FACE_OUTER_BOUND('',#5686,.T.);
#4022=FACE_OUTER_BOUND('',#5687,.T.);
#4023=FACE_OUTER_BOUND('',#5688,.T.);
#4024=FACE_OUTER_BOUND('',#5689,.T.);
#4025=FACE_OUTER_BOUND('',#5690,.T.);
#4026=FACE_OUTER_BOUND('',#5691,.T.);
#4027=FACE_OUTER_BOUND('',#5694,.T.);
#4028=FACE_OUTER_BOUND('',#5695,.T.);
#4029=FACE_OUTER_BOUND('',#5696,.T.);
#4030=FACE_OUTER_BOUND('',#5697,.T.);
#4031=FACE_OUTER_BOUND('',#5698,.T.);
#4032=FACE_OUTER_BOUND('',#5701,.T.);
#4033=FACE_OUTER_BOUND('',#5702,.T.);
#4034=FACE_OUTER_BOUND('',#5703,.T.);
#4035=FACE_OUTER_BOUND('',#5704,.T.);
#4036=FACE_OUTER_BOUND('',#5705,.T.);
#4037=FACE_OUTER_BOUND('',#5706,.T.);
#4038=FACE_OUTER_BOUND('',#5707,.T.);
#4039=FACE_OUTER_BOUND('',#5708,.T.);
#4040=FACE_OUTER_BOUND('',#5709,.T.);
#4041=FACE_OUTER_BOUND('',#5710,.T.);
#4042=FACE_OUTER_BOUND('',#5711,.T.);
#4043=FACE_OUTER_BOUND('',#5712,.T.);
#4044=FACE_OUTER_BOUND('',#5713,.T.);
#4045=FACE_OUTER_BOUND('',#5714,.T.);
#4046=FACE_OUTER_BOUND('',#5715,.T.);
#4047=FACE_OUTER_BOUND('',#5716,.T.);
#4048=FACE_OUTER_BOUND('',#5721,.T.);
#4049=FACE_OUTER_BOUND('',#5722,.T.);
#4050=FACE_OUTER_BOUND('',#5723,.T.);
#4051=FACE_OUTER_BOUND('',#5724,.T.);
#4052=FACE_OUTER_BOUND('',#5725,.T.);
#4053=FACE_OUTER_BOUND('',#5726,.T.);
#4054=FACE_OUTER_BOUND('',#5727,.T.);
#4055=FACE_OUTER_BOUND('',#5728,.T.);
#4056=FACE_OUTER_BOUND('',#5729,.T.);
#4057=FACE_OUTER_BOUND('',#5730,.T.);
#4058=FACE_OUTER_BOUND('',#5731,.T.);
#4059=FACE_OUTER_BOUND('',#5732,.T.);
#4060=FACE_OUTER_BOUND('',#5733,.T.);
#4061=FACE_OUTER_BOUND('',#5734,.T.);
#4062=FACE_OUTER_BOUND('',#5735,.T.);
#4063=FACE_OUTER_BOUND('',#5736,.T.);
#4064=FACE_OUTER_BOUND('',#5737,.T.);
#4065=FACE_OUTER_BOUND('',#5738,.T.);
#4066=FACE_OUTER_BOUND('',#5739,.T.);
#4067=FACE_OUTER_BOUND('',#5740,.T.);
#4068=FACE_OUTER_BOUND('',#5741,.T.);
#4069=FACE_OUTER_BOUND('',#5742,.T.);
#4070=FACE_OUTER_BOUND('',#5743,.T.);
#4071=FACE_OUTER_BOUND('',#5747,.T.);
#4072=FACE_OUTER_BOUND('',#5748,.T.);
#4073=FACE_OUTER_BOUND('',#5749,.T.);
#4074=FACE_OUTER_BOUND('',#5750,.T.);
#4075=FACE_OUTER_BOUND('',#5751,.T.);
#4076=FACE_OUTER_BOUND('',#5754,.T.);
#4077=FACE_OUTER_BOUND('',#5755,.T.);
#4078=FACE_OUTER_BOUND('',#5756,.T.);
#4079=FACE_OUTER_BOUND('',#5757,.T.);
#4080=FACE_OUTER_BOUND('',#5760,.T.);
#4081=FACE_OUTER_BOUND('',#5761,.T.);
#4082=FACE_OUTER_BOUND('',#5762,.T.);
#4083=FACE_OUTER_BOUND('',#5763,.T.);
#4084=FACE_OUTER_BOUND('',#5764,.T.);
#4085=FACE_OUTER_BOUND('',#5765,.T.);
#4086=FACE_OUTER_BOUND('',#5766,.T.);
#4087=FACE_OUTER_BOUND('',#5767,.T.);
#4088=FACE_OUTER_BOUND('',#5768,.T.);
#4089=FACE_OUTER_BOUND('',#5769,.T.);
#4090=FACE_OUTER_BOUND('',#5770,.T.);
#4091=FACE_OUTER_BOUND('',#5771,.T.);
#4092=FACE_OUTER_BOUND('',#5772,.T.);
#4093=FACE_OUTER_BOUND('',#5773,.T.);
#4094=FACE_OUTER_BOUND('',#5774,.T.);
#4095=FACE_OUTER_BOUND('',#5775,.T.);
#4096=FACE_OUTER_BOUND('',#5776,.T.);
#4097=FACE_OUTER_BOUND('',#5777,.T.);
#4098=FACE_OUTER_BOUND('',#5778,.T.);
#4099=FACE_OUTER_BOUND('',#5779,.T.);
#4100=FACE_OUTER_BOUND('',#5780,.T.);
#4101=FACE_OUTER_BOUND('',#5781,.T.);
#4102=FACE_OUTER_BOUND('',#5782,.T.);
#4103=FACE_OUTER_BOUND('',#5783,.T.);
#4104=FACE_OUTER_BOUND('',#5785,.T.);
#4105=FACE_OUTER_BOUND('',#5786,.T.);
#4106=FACE_OUTER_BOUND('',#5787,.T.);
#4107=FACE_OUTER_BOUND('',#5788,.T.);
#4108=FACE_OUTER_BOUND('',#5789,.T.);
#4109=FACE_OUTER_BOUND('',#5791,.T.);
#4110=FACE_OUTER_BOUND('',#5792,.T.);
#4111=FACE_OUTER_BOUND('',#5793,.T.);
#4112=FACE_OUTER_BOUND('',#5794,.T.);
#4113=FACE_OUTER_BOUND('',#5795,.T.);
#4114=FACE_OUTER_BOUND('',#5796,.T.);
#4115=FACE_OUTER_BOUND('',#5797,.T.);
#4116=FACE_OUTER_BOUND('',#5798,.T.);
#4117=FACE_OUTER_BOUND('',#5799,.T.);
#4118=FACE_OUTER_BOUND('',#5800,.T.);
#4119=FACE_OUTER_BOUND('',#5801,.T.);
#4120=FACE_OUTER_BOUND('',#5802,.T.);
#4121=FACE_OUTER_BOUND('',#5803,.T.);
#4122=FACE_OUTER_BOUND('',#5804,.T.);
#4123=FACE_OUTER_BOUND('',#5805,.T.);
#4124=FACE_OUTER_BOUND('',#5806,.T.);
#4125=FACE_OUTER_BOUND('',#5807,.T.);
#4126=FACE_OUTER_BOUND('',#5808,.T.);
#4127=FACE_OUTER_BOUND('',#5809,.T.);
#4128=FACE_OUTER_BOUND('',#5810,.T.);
#4129=FACE_OUTER_BOUND('',#5811,.T.);
#4130=FACE_OUTER_BOUND('',#5812,.T.);
#4131=FACE_OUTER_BOUND('',#5813,.T.);
#4132=FACE_OUTER_BOUND('',#5814,.T.);
#4133=FACE_OUTER_BOUND('',#5815,.T.);
#4134=FACE_OUTER_BOUND('',#5816,.T.);
#4135=FACE_OUTER_BOUND('',#5817,.T.);
#4136=FACE_OUTER_BOUND('',#5818,.T.);
#4137=FACE_OUTER_BOUND('',#5819,.T.);
#4138=FACE_OUTER_BOUND('',#5820,.T.);
#4139=FACE_OUTER_BOUND('',#5821,.T.);
#4140=FACE_OUTER_BOUND('',#5822,.T.);
#4141=FACE_OUTER_BOUND('',#5823,.T.);
#4142=FACE_OUTER_BOUND('',#5824,.T.);
#4143=FACE_OUTER_BOUND('',#5825,.T.);
#4144=FACE_OUTER_BOUND('',#5826,.T.);
#4145=FACE_OUTER_BOUND('',#5827,.T.);
#4146=FACE_OUTER_BOUND('',#5828,.T.);
#4147=FACE_OUTER_BOUND('',#5829,.T.);
#4148=FACE_OUTER_BOUND('',#5830,.T.);
#4149=FACE_OUTER_BOUND('',#5831,.T.);
#4150=FACE_OUTER_BOUND('',#5832,.T.);
#4151=FACE_OUTER_BOUND('',#5833,.T.);
#4152=FACE_OUTER_BOUND('',#5834,.T.);
#4153=FACE_OUTER_BOUND('',#5835,.T.);
#4154=FACE_OUTER_BOUND('',#5836,.T.);
#4155=FACE_OUTER_BOUND('',#5837,.T.);
#4156=FACE_OUTER_BOUND('',#5838,.T.);
#4157=FACE_OUTER_BOUND('',#5839,.T.);
#4158=FACE_OUTER_BOUND('',#5840,.T.);
#4159=FACE_OUTER_BOUND('',#5841,.T.);
#4160=FACE_OUTER_BOUND('',#5842,.T.);
#4161=FACE_OUTER_BOUND('',#5843,.T.);
#4162=FACE_OUTER_BOUND('',#5844,.T.);
#4163=FACE_OUTER_BOUND('',#5845,.T.);
#4164=FACE_OUTER_BOUND('',#5846,.T.);
#4165=FACE_OUTER_BOUND('',#5847,.T.);
#4166=FACE_OUTER_BOUND('',#5848,.T.);
#4167=FACE_OUTER_BOUND('',#5849,.T.);
#4168=FACE_OUTER_BOUND('',#5850,.T.);
#4169=FACE_OUTER_BOUND('',#5851,.T.);
#4170=FACE_OUTER_BOUND('',#5852,.T.);
#4171=FACE_OUTER_BOUND('',#5853,.T.);
#4172=FACE_OUTER_BOUND('',#5854,.T.);
#4173=FACE_OUTER_BOUND('',#5855,.T.);
#4174=FACE_OUTER_BOUND('',#5856,.T.);
#4175=FACE_OUTER_BOUND('',#5857,.T.);
#4176=FACE_OUTER_BOUND('',#5858,.T.);
#4177=FACE_OUTER_BOUND('',#5859,.T.);
#4178=FACE_OUTER_BOUND('',#5860,.T.);
#4179=FACE_OUTER_BOUND('',#5861,.T.);
#4180=FACE_OUTER_BOUND('',#5862,.T.);
#4181=FACE_OUTER_BOUND('',#5863,.T.);
#4182=FACE_OUTER_BOUND('',#5864,.T.);
#4183=FACE_OUTER_BOUND('',#5865,.T.);
#4184=FACE_OUTER_BOUND('',#5866,.T.);
#4185=FACE_OUTER_BOUND('',#5867,.T.);
#4186=FACE_OUTER_BOUND('',#5868,.T.);
#4187=FACE_OUTER_BOUND('',#5869,.T.);
#4188=FACE_OUTER_BOUND('',#5870,.T.);
#4189=FACE_OUTER_BOUND('',#5871,.T.);
#4190=FACE_OUTER_BOUND('',#5872,.T.);
#4191=FACE_OUTER_BOUND('',#5873,.T.);
#4192=FACE_OUTER_BOUND('',#5874,.T.);
#4193=FACE_OUTER_BOUND('',#5875,.T.);
#4194=FACE_OUTER_BOUND('',#5876,.T.);
#4195=FACE_OUTER_BOUND('',#5877,.T.);
#4196=FACE_OUTER_BOUND('',#5878,.T.);
#4197=FACE_OUTER_BOUND('',#5879,.T.);
#4198=FACE_OUTER_BOUND('',#5880,.T.);
#4199=FACE_OUTER_BOUND('',#5881,.T.);
#4200=FACE_OUTER_BOUND('',#5882,.T.);
#4201=FACE_OUTER_BOUND('',#5883,.T.);
#4202=FACE_OUTER_BOUND('',#5884,.T.);
#4203=FACE_OUTER_BOUND('',#5885,.T.);
#4204=FACE_OUTER_BOUND('',#5886,.T.);
#4205=FACE_OUTER_BOUND('',#5887,.T.);
#4206=FACE_OUTER_BOUND('',#5888,.T.);
#4207=FACE_OUTER_BOUND('',#5889,.T.);
#4208=FACE_OUTER_BOUND('',#5890,.T.);
#4209=FACE_OUTER_BOUND('',#5891,.T.);
#4210=FACE_OUTER_BOUND('',#5892,.T.);
#4211=FACE_OUTER_BOUND('',#5893,.T.);
#4212=FACE_OUTER_BOUND('',#5894,.T.);
#4213=FACE_OUTER_BOUND('',#5895,.T.);
#4214=FACE_OUTER_BOUND('',#5896,.T.);
#4215=FACE_OUTER_BOUND('',#5897,.T.);
#4216=FACE_OUTER_BOUND('',#5898,.T.);
#4217=FACE_OUTER_BOUND('',#5899,.T.);
#4218=FACE_OUTER_BOUND('',#5900,.T.);
#4219=FACE_OUTER_BOUND('',#5901,.T.);
#4220=FACE_OUTER_BOUND('',#5902,.T.);
#4221=FACE_OUTER_BOUND('',#5903,.T.);
#4222=FACE_OUTER_BOUND('',#5904,.T.);
#4223=FACE_OUTER_BOUND('',#5905,.T.);
#4224=FACE_OUTER_BOUND('',#5906,.T.);
#4225=FACE_OUTER_BOUND('',#5907,.T.);
#4226=FACE_OUTER_BOUND('',#5908,.T.);
#4227=FACE_OUTER_BOUND('',#5909,.T.);
#4228=FACE_OUTER_BOUND('',#5910,.T.);
#4229=FACE_OUTER_BOUND('',#5911,.T.);
#4230=FACE_OUTER_BOUND('',#5912,.T.);
#4231=FACE_OUTER_BOUND('',#5913,.T.);
#4232=FACE_OUTER_BOUND('',#5914,.T.);
#4233=FACE_OUTER_BOUND('',#5915,.T.);
#4234=FACE_OUTER_BOUND('',#5916,.T.);
#4235=FACE_OUTER_BOUND('',#5917,.T.);
#4236=FACE_OUTER_BOUND('',#5918,.T.);
#4237=FACE_OUTER_BOUND('',#5919,.T.);
#4238=FACE_OUTER_BOUND('',#5920,.T.);
#4239=FACE_OUTER_BOUND('',#5921,.T.);
#4240=FACE_OUTER_BOUND('',#5922,.T.);
#4241=FACE_OUTER_BOUND('',#5923,.T.);
#4242=FACE_OUTER_BOUND('',#5924,.T.);
#4243=FACE_OUTER_BOUND('',#5925,.T.);
#4244=FACE_OUTER_BOUND('',#5926,.T.);
#4245=FACE_OUTER_BOUND('',#5927,.T.);
#4246=FACE_OUTER_BOUND('',#5928,.T.);
#4247=FACE_OUTER_BOUND('',#5929,.T.);
#4248=FACE_OUTER_BOUND('',#5930,.T.);
#4249=FACE_OUTER_BOUND('',#5931,.T.);
#4250=FACE_OUTER_BOUND('',#5932,.T.);
#4251=FACE_OUTER_BOUND('',#5933,.T.);
#4252=FACE_OUTER_BOUND('',#5934,.T.);
#4253=FACE_OUTER_BOUND('',#5935,.T.);
#4254=FACE_OUTER_BOUND('',#5936,.T.);
#4255=FACE_OUTER_BOUND('',#5937,.T.);
#4256=FACE_OUTER_BOUND('',#5938,.T.);
#4257=FACE_OUTER_BOUND('',#5939,.T.);
#4258=FACE_OUTER_BOUND('',#5940,.T.);
#4259=FACE_OUTER_BOUND('',#5941,.T.);
#4260=FACE_OUTER_BOUND('',#5942,.T.);
#4261=FACE_OUTER_BOUND('',#5943,.T.);
#4262=FACE_OUTER_BOUND('',#5944,.T.);
#4263=FACE_OUTER_BOUND('',#5945,.T.);
#4264=FACE_OUTER_BOUND('',#5946,.T.);
#4265=FACE_OUTER_BOUND('',#5947,.T.);
#4266=FACE_OUTER_BOUND('',#5948,.T.);
#4267=FACE_OUTER_BOUND('',#5949,.T.);
#4268=FACE_OUTER_BOUND('',#5950,.T.);
#4269=FACE_OUTER_BOUND('',#5951,.T.);
#4270=FACE_OUTER_BOUND('',#5952,.T.);
#4271=FACE_OUTER_BOUND('',#5953,.T.);
#4272=FACE_OUTER_BOUND('',#5954,.T.);
#4273=FACE_OUTER_BOUND('',#5955,.T.);
#4274=FACE_OUTER_BOUND('',#5956,.T.);
#4275=FACE_OUTER_BOUND('',#5957,.T.);
#4276=FACE_OUTER_BOUND('',#5958,.T.);
#4277=FACE_OUTER_BOUND('',#5959,.T.);
#4278=FACE_OUTER_BOUND('',#5960,.T.);
#4279=FACE_OUTER_BOUND('',#5961,.T.);
#4280=FACE_OUTER_BOUND('',#5962,.T.);
#4281=FACE_OUTER_BOUND('',#5963,.T.);
#4282=FACE_OUTER_BOUND('',#5964,.T.);
#4283=FACE_OUTER_BOUND('',#5965,.T.);
#4284=FACE_OUTER_BOUND('',#5966,.T.);
#4285=FACE_OUTER_BOUND('',#5967,.T.);
#4286=FACE_OUTER_BOUND('',#5968,.T.);
#4287=FACE_OUTER_BOUND('',#5969,.T.);
#4288=FACE_OUTER_BOUND('',#5970,.T.);
#4289=FACE_OUTER_BOUND('',#5971,.T.);
#4290=FACE_OUTER_BOUND('',#5972,.T.);
#4291=FACE_OUTER_BOUND('',#5973,.T.);
#4292=FACE_OUTER_BOUND('',#5974,.T.);
#4293=FACE_OUTER_BOUND('',#5975,.T.);
#4294=FACE_OUTER_BOUND('',#5976,.T.);
#4295=FACE_OUTER_BOUND('',#5977,.T.);
#4296=FACE_OUTER_BOUND('',#5978,.T.);
#4297=FACE_OUTER_BOUND('',#5979,.T.);
#4298=FACE_OUTER_BOUND('',#5980,.T.);
#4299=FACE_OUTER_BOUND('',#5981,.T.);
#4300=FACE_OUTER_BOUND('',#5982,.T.);
#4301=FACE_OUTER_BOUND('',#5983,.T.);
#4302=FACE_OUTER_BOUND('',#5984,.T.);
#4303=FACE_OUTER_BOUND('',#5985,.T.);
#4304=FACE_OUTER_BOUND('',#5986,.T.);
#4305=FACE_OUTER_BOUND('',#5987,.T.);
#4306=FACE_OUTER_BOUND('',#5988,.T.);
#4307=FACE_OUTER_BOUND('',#5989,.T.);
#4308=FACE_OUTER_BOUND('',#5990,.T.);
#4309=FACE_OUTER_BOUND('',#5991,.T.);
#4310=FACE_OUTER_BOUND('',#5992,.T.);
#4311=FACE_OUTER_BOUND('',#5993,.T.);
#4312=FACE_OUTER_BOUND('',#5994,.T.);
#4313=FACE_OUTER_BOUND('',#5995,.T.);
#4314=FACE_OUTER_BOUND('',#5996,.T.);
#4315=FACE_OUTER_BOUND('',#5997,.T.);
#4316=FACE_OUTER_BOUND('',#6000,.T.);
#4317=FACE_OUTER_BOUND('',#6001,.T.);
#4318=FACE_OUTER_BOUND('',#6002,.T.);
#4319=FACE_OUTER_BOUND('',#6003,.T.);
#4320=FACE_OUTER_BOUND('',#6004,.T.);
#4321=FACE_OUTER_BOUND('',#6005,.T.);
#4322=FACE_OUTER_BOUND('',#6006,.T.);
#4323=FACE_OUTER_BOUND('',#6007,.T.);
#4324=FACE_OUTER_BOUND('',#6008,.T.);
#4325=FACE_OUTER_BOUND('',#6009,.T.);
#4326=FACE_OUTER_BOUND('',#6010,.T.);
#4327=FACE_OUTER_BOUND('',#6011,.T.);
#4328=FACE_OUTER_BOUND('',#6012,.T.);
#4329=FACE_OUTER_BOUND('',#6013,.T.);
#4330=FACE_OUTER_BOUND('',#6014,.T.);
#4331=FACE_OUTER_BOUND('',#6015,.T.);
#4332=FACE_OUTER_BOUND('',#6016,.T.);
#4333=FACE_OUTER_BOUND('',#6017,.T.);
#4334=FACE_OUTER_BOUND('',#6018,.T.);
#4335=FACE_OUTER_BOUND('',#6019,.T.);
#4336=FACE_OUTER_BOUND('',#6020,.T.);
#4337=FACE_OUTER_BOUND('',#6021,.T.);
#4338=FACE_OUTER_BOUND('',#6022,.T.);
#4339=FACE_OUTER_BOUND('',#6023,.T.);
#4340=FACE_OUTER_BOUND('',#6024,.T.);
#4341=FACE_OUTER_BOUND('',#6025,.T.);
#4342=FACE_OUTER_BOUND('',#6026,.T.);
#4343=FACE_OUTER_BOUND('',#6027,.T.);
#4344=FACE_OUTER_BOUND('',#6028,.T.);
#4345=FACE_OUTER_BOUND('',#6029,.T.);
#4346=FACE_OUTER_BOUND('',#6030,.T.);
#4347=FACE_OUTER_BOUND('',#6031,.T.);
#4348=FACE_OUTER_BOUND('',#6032,.T.);
#4349=FACE_OUTER_BOUND('',#6033,.T.);
#4350=FACE_OUTER_BOUND('',#6034,.T.);
#4351=FACE_OUTER_BOUND('',#6035,.T.);
#4352=FACE_OUTER_BOUND('',#6036,.T.);
#4353=FACE_OUTER_BOUND('',#6037,.T.);
#4354=FACE_OUTER_BOUND('',#6038,.T.);
#4355=FACE_OUTER_BOUND('',#6041,.T.);
#4356=FACE_OUTER_BOUND('',#6042,.T.);
#4357=FACE_OUTER_BOUND('',#6043,.T.);
#4358=FACE_OUTER_BOUND('',#6044,.T.);
#4359=FACE_OUTER_BOUND('',#6045,.T.);
#4360=FACE_OUTER_BOUND('',#6046,.T.);
#4361=FACE_OUTER_BOUND('',#6047,.T.);
#4362=FACE_OUTER_BOUND('',#6048,.T.);
#4363=FACE_OUTER_BOUND('',#6049,.T.);
#4364=FACE_OUTER_BOUND('',#6050,.T.);
#4365=FACE_OUTER_BOUND('',#6051,.T.);
#4366=FACE_OUTER_BOUND('',#6053,.T.);
#4367=FACE_OUTER_BOUND('',#6054,.T.);
#4368=FACE_OUTER_BOUND('',#6055,.T.);
#4369=FACE_OUTER_BOUND('',#6056,.T.);
#4370=FACE_OUTER_BOUND('',#6057,.T.);
#4371=FACE_OUTER_BOUND('',#6058,.T.);
#4372=FACE_OUTER_BOUND('',#6059,.T.);
#4373=FACE_OUTER_BOUND('',#6060,.T.);
#4374=FACE_OUTER_BOUND('',#6061,.T.);
#4375=FACE_OUTER_BOUND('',#6065,.T.);
#4376=FACE_OUTER_BOUND('',#6066,.T.);
#4377=FACE_OUTER_BOUND('',#6067,.T.);
#4378=FACE_OUTER_BOUND('',#6068,.T.);
#4379=FACE_OUTER_BOUND('',#6069,.T.);
#4380=FACE_OUTER_BOUND('',#6071,.T.);
#4381=FACE_OUTER_BOUND('',#6072,.T.);
#4382=FACE_OUTER_BOUND('',#6074,.T.);
#4383=FACE_OUTER_BOUND('',#6075,.T.);
#4384=FACE_OUTER_BOUND('',#6076,.T.);
#4385=FACE_OUTER_BOUND('',#6077,.T.);
#4386=FACE_OUTER_BOUND('',#6078,.T.);
#4387=FACE_OUTER_BOUND('',#6079,.T.);
#4388=FACE_OUTER_BOUND('',#6080,.T.);
#4389=FACE_OUTER_BOUND('',#6081,.T.);
#4390=FACE_OUTER_BOUND('',#6082,.T.);
#4391=FACE_OUTER_BOUND('',#6083,.T.);
#4392=FACE_OUTER_BOUND('',#6085,.T.);
#4393=FACE_OUTER_BOUND('',#6086,.T.);
#4394=FACE_OUTER_BOUND('',#6087,.T.);
#4395=FACE_OUTER_BOUND('',#6089,.T.);
#4396=FACE_OUTER_BOUND('',#6090,.T.);
#4397=FACE_OUTER_BOUND('',#6091,.T.);
#4398=FACE_OUTER_BOUND('',#6092,.T.);
#4399=FACE_OUTER_BOUND('',#6093,.T.);
#4400=FACE_OUTER_BOUND('',#6094,.T.);
#4401=FACE_OUTER_BOUND('',#6095,.T.);
#4402=FACE_OUTER_BOUND('',#6096,.T.);
#4403=FACE_OUTER_BOUND('',#6097,.T.);
#4404=FACE_OUTER_BOUND('',#6099,.T.);
#4405=FACE_OUTER_BOUND('',#6100,.T.);
#4406=FACE_OUTER_BOUND('',#6102,.T.);
#4407=FACE_OUTER_BOUND('',#6103,.T.);
#4408=FACE_OUTER_BOUND('',#6104,.T.);
#4409=FACE_OUTER_BOUND('',#6106,.T.);
#4410=FACE_OUTER_BOUND('',#6108,.T.);
#4411=FACE_OUTER_BOUND('',#6109,.T.);
#4412=FACE_OUTER_BOUND('',#6111,.T.);
#4413=FACE_OUTER_BOUND('',#6112,.T.);
#4414=FACE_OUTER_BOUND('',#6114,.T.);
#4415=FACE_OUTER_BOUND('',#6115,.T.);
#4416=FACE_OUTER_BOUND('',#6117,.T.);
#4417=FACE_OUTER_BOUND('',#6118,.T.);
#4418=FACE_OUTER_BOUND('',#6120,.T.);
#4419=FACE_OUTER_BOUND('',#6121,.T.);
#4420=FACE_OUTER_BOUND('',#6123,.T.);
#4421=FACE_OUTER_BOUND('',#6125,.T.);
#4422=FACE_OUTER_BOUND('',#6126,.T.);
#4423=FACE_OUTER_BOUND('',#6127,.T.);
#4424=FACE_OUTER_BOUND('',#6128,.T.);
#4425=FACE_OUTER_BOUND('',#6130,.T.);
#4426=FACE_OUTER_BOUND('',#6131,.T.);
#4427=FACE_OUTER_BOUND('',#6132,.T.);
#4428=FACE_OUTER_BOUND('',#6133,.T.);
#4429=FACE_OUTER_BOUND('',#6134,.T.);
#4430=FACE_OUTER_BOUND('',#6135,.T.);
#4431=FACE_OUTER_BOUND('',#6136,.T.);
#4432=FACE_OUTER_BOUND('',#6137,.T.);
#4433=FACE_OUTER_BOUND('',#6138,.T.);
#4434=FACE_OUTER_BOUND('',#6139,.T.);
#4435=FACE_OUTER_BOUND('',#6140,.T.);
#4436=FACE_OUTER_BOUND('',#6141,.T.);
#4437=FACE_OUTER_BOUND('',#6153,.T.);
#4438=FACE_OUTER_BOUND('',#6154,.T.);
#4439=FACE_OUTER_BOUND('',#6155,.T.);
#4440=FACE_OUTER_BOUND('',#6156,.T.);
#4441=FACE_OUTER_BOUND('',#6157,.T.);
#4442=FACE_OUTER_BOUND('',#6158,.T.);
#4443=FACE_OUTER_BOUND('',#6159,.T.);
#4444=FACE_OUTER_BOUND('',#6160,.T.);
#4445=FACE_OUTER_BOUND('',#6161,.T.);
#4446=FACE_OUTER_BOUND('',#6162,.T.);
#4447=FACE_OUTER_BOUND('',#6163,.T.);
#4448=FACE_OUTER_BOUND('',#6164,.T.);
#4449=FACE_OUTER_BOUND('',#6165,.T.);
#4450=FACE_OUTER_BOUND('',#6166,.T.);
#4451=FACE_OUTER_BOUND('',#6167,.T.);
#4452=FACE_OUTER_BOUND('',#6179,.T.);
#4453=FACE_OUTER_BOUND('',#6180,.T.);
#4454=FACE_OUTER_BOUND('',#6181,.T.);
#4455=FACE_OUTER_BOUND('',#6182,.T.);
#4456=FACE_OUTER_BOUND('',#6183,.T.);
#4457=FACE_OUTER_BOUND('',#6184,.T.);
#4458=FACE_OUTER_BOUND('',#6185,.T.);
#4459=FACE_OUTER_BOUND('',#6186,.T.);
#4460=FACE_OUTER_BOUND('',#6187,.T.);
#4461=FACE_OUTER_BOUND('',#6188,.T.);
#4462=FACE_OUTER_BOUND('',#6189,.T.);
#4463=FACE_OUTER_BOUND('',#6190,.T.);
#4464=FACE_OUTER_BOUND('',#6191,.T.);
#4465=FACE_OUTER_BOUND('',#6192,.T.);
#4466=FACE_OUTER_BOUND('',#6193,.T.);
#4467=FACE_OUTER_BOUND('',#6194,.T.);
#4468=FACE_OUTER_BOUND('',#6195,.T.);
#4469=FACE_OUTER_BOUND('',#6196,.T.);
#4470=FACE_OUTER_BOUND('',#6197,.T.);
#4471=FACE_OUTER_BOUND('',#6198,.T.);
#4472=FACE_OUTER_BOUND('',#6199,.T.);
#4473=FACE_OUTER_BOUND('',#6201,.T.);
#4474=FACE_OUTER_BOUND('',#6202,.T.);
#4475=FACE_OUTER_BOUND('',#6203,.T.);
#4476=FACE_OUTER_BOUND('',#6204,.T.);
#4477=FACE_OUTER_BOUND('',#6205,.T.);
#4478=FACE_OUTER_BOUND('',#6206,.T.);
#4479=FACE_OUTER_BOUND('',#6207,.T.);
#4480=FACE_OUTER_BOUND('',#6208,.T.);
#4481=FACE_OUTER_BOUND('',#6209,.T.);
#4482=FACE_OUTER_BOUND('',#6210,.T.);
#4483=FACE_OUTER_BOUND('',#6211,.T.);
#4484=FACE_OUTER_BOUND('',#6212,.T.);
#4485=FACE_OUTER_BOUND('',#6213,.T.);
#4486=FACE_OUTER_BOUND('',#6214,.T.);
#4487=FACE_OUTER_BOUND('',#6215,.T.);
#4488=FACE_OUTER_BOUND('',#6216,.T.);
#4489=FACE_OUTER_BOUND('',#6217,.T.);
#4490=FACE_OUTER_BOUND('',#6218,.T.);
#4491=FACE_OUTER_BOUND('',#6219,.T.);
#4492=FACE_OUTER_BOUND('',#6220,.T.);
#4493=FACE_OUTER_BOUND('',#6232,.T.);
#4494=FACE_OUTER_BOUND('',#6233,.T.);
#4495=FACE_OUTER_BOUND('',#6234,.T.);
#4496=FACE_OUTER_BOUND('',#6235,.T.);
#4497=FACE_OUTER_BOUND('',#6236,.T.);
#4498=FACE_OUTER_BOUND('',#6237,.T.);
#4499=FACE_OUTER_BOUND('',#6238,.T.);
#4500=FACE_OUTER_BOUND('',#6239,.T.);
#4501=FACE_OUTER_BOUND('',#6251,.T.);
#4502=FACE_OUTER_BOUND('',#6252,.T.);
#4503=FACE_OUTER_BOUND('',#6253,.T.);
#4504=FACE_OUTER_BOUND('',#6254,.T.);
#4505=FACE_OUTER_BOUND('',#6255,.T.);
#4506=FACE_OUTER_BOUND('',#6256,.T.);
#4507=FACE_OUTER_BOUND('',#6257,.T.);
#4508=FACE_OUTER_BOUND('',#6258,.T.);
#4509=FACE_OUTER_BOUND('',#6259,.T.);
#4510=FACE_OUTER_BOUND('',#6260,.T.);
#4511=FACE_OUTER_BOUND('',#6261,.T.);
#4512=FACE_OUTER_BOUND('',#6262,.T.);
#4513=FACE_OUTER_BOUND('',#6263,.T.);
#4514=FACE_OUTER_BOUND('',#6264,.T.);
#4515=FACE_OUTER_BOUND('',#6265,.T.);
#4516=FACE_OUTER_BOUND('',#6266,.T.);
#4517=FACE_OUTER_BOUND('',#6267,.T.);
#4518=FACE_OUTER_BOUND('',#6268,.T.);
#4519=FACE_OUTER_BOUND('',#6269,.T.);
#4520=FACE_OUTER_BOUND('',#6270,.T.);
#4521=FACE_OUTER_BOUND('',#6271,.T.);
#4522=FACE_OUTER_BOUND('',#6272,.T.);
#4523=FACE_OUTER_BOUND('',#6273,.T.);
#4524=FACE_OUTER_BOUND('',#6274,.T.);
#4525=FACE_OUTER_BOUND('',#6275,.T.);
#4526=FACE_OUTER_BOUND('',#6276,.T.);
#4527=FACE_OUTER_BOUND('',#6277,.T.);
#4528=FACE_OUTER_BOUND('',#6278,.T.);
#4529=FACE_OUTER_BOUND('',#6279,.T.);
#4530=FACE_OUTER_BOUND('',#6280,.T.);
#4531=FACE_OUTER_BOUND('',#6281,.T.);
#4532=FACE_OUTER_BOUND('',#6282,.T.);
#4533=FACE_OUTER_BOUND('',#6283,.T.);
#4534=FACE_OUTER_BOUND('',#6284,.T.);
#4535=FACE_OUTER_BOUND('',#6285,.T.);
#4536=FACE_OUTER_BOUND('',#6286,.T.);
#4537=FACE_OUTER_BOUND('',#6287,.T.);
#4538=FACE_OUTER_BOUND('',#6289,.T.);
#4539=FACE_OUTER_BOUND('',#6290,.T.);
#4540=FACE_OUTER_BOUND('',#6291,.T.);
#4541=FACE_OUTER_BOUND('',#6292,.T.);
#4542=FACE_OUTER_BOUND('',#6293,.T.);
#4543=FACE_OUTER_BOUND('',#6294,.T.);
#4544=FACE_OUTER_BOUND('',#6295,.T.);
#4545=FACE_OUTER_BOUND('',#6296,.T.);
#4546=FACE_OUTER_BOUND('',#6297,.T.);
#4547=FACE_OUTER_BOUND('',#6298,.T.);
#4548=FACE_OUTER_BOUND('',#6299,.T.);
#4549=FACE_OUTER_BOUND('',#6300,.T.);
#4550=FACE_OUTER_BOUND('',#6301,.T.);
#4551=EDGE_LOOP('',(#17919,#17920,#17921,#17922,#17923));
#4552=EDGE_LOOP('',(#17924,#17925,#17926,#17927,#17928,#17929));
#4553=EDGE_LOOP('',(#17930,#17931,#17932,#17933));
#4554=EDGE_LOOP('',(#17934,#17935,#17936,#17937));
#4555=EDGE_LOOP('',(#17938,#17939,#17940,#17941,#17942));
#4556=EDGE_LOOP('',(#17943,#17944,#17945,#17946,#17947,#17948));
#4557=EDGE_LOOP('',(#17949,#17950,#17951,#17952,#17953,#17954,#17955,#17956));
#4558=EDGE_LOOP('',(#17957,#17958,#17959,#17960,#17961));
#4559=EDGE_LOOP('',(#17962,#17963,#17964,#17965));
#4560=EDGE_LOOP('',(#17966,#17967,#17968,#17969,#17970,#17971));
#4561=EDGE_LOOP('',(#17972,#17973,#17974,#17975,#17976,#17977));
#4562=EDGE_LOOP('',(#17978,#17979,#17980,#17981));
#4563=EDGE_LOOP('',(#17982,#17983,#17984,#17985));
#4564=EDGE_LOOP('',(#17986,#17987,#17988,#17989,#17990));
#4565=EDGE_LOOP('',(#17991,#17992,#17993,#17994));
#4566=EDGE_LOOP('',(#17995,#17996,#17997,#17998));
#4567=EDGE_LOOP('',(#17999));
#4568=EDGE_LOOP('',(#18000));
#4569=EDGE_LOOP('',(#18001));
#4570=EDGE_LOOP('',(#18002));
#4571=EDGE_LOOP('',(#18003,#18004,#18005,#18006));
#4572=EDGE_LOOP('',(#18007,#18008,#18009,#18010));
#4573=EDGE_LOOP('',(#18011,#18012,#18013,#18014));
#4574=EDGE_LOOP('',(#18015,#18016,#18017,#18018));
#4575=EDGE_LOOP('',(#18019,#18020,#18021,#18022));
#4576=EDGE_LOOP('',(#18023,#18024,#18025,#18026));
#4577=EDGE_LOOP('',(#18027,#18028,#18029,#18030));
#4578=EDGE_LOOP('',(#18031,#18032,#18033,#18034));
#4579=EDGE_LOOP('',(#18035,#18036,#18037,#18038));
#4580=EDGE_LOOP('',(#18039));
#4581=EDGE_LOOP('',(#18040));
#4582=EDGE_LOOP('',(#18041));
#4583=EDGE_LOOP('',(#18042));
#4584=EDGE_LOOP('',(#18043,#18044,#18045,#18046));
#4585=EDGE_LOOP('',(#18047,#18048,#18049,#18050));
#4586=EDGE_LOOP('',(#18051,#18052,#18053,#18054));
#4587=EDGE_LOOP('',(#18055,#18056,#18057,#18058));
#4588=EDGE_LOOP('',(#18059,#18060,#18061,#18062));
#4589=EDGE_LOOP('',(#18063));
#4590=EDGE_LOOP('',(#18064));
#4591=EDGE_LOOP('',(#18065));
#4592=EDGE_LOOP('',(#18066));
#4593=EDGE_LOOP('',(#18067,#18068,#18069,#18070));
#4594=EDGE_LOOP('',(#18071,#18072,#18073,#18074));
#4595=EDGE_LOOP('',(#18075,#18076,#18077,#18078));
#4596=EDGE_LOOP('',(#18079,#18080,#18081,#18082));
#4597=EDGE_LOOP('',(#18083,#18084,#18085,#18086));
#4598=EDGE_LOOP('',(#18087,#18088,#18089,#18090));
#4599=EDGE_LOOP('',(#18091,#18092,#18093,#18094));
#4600=EDGE_LOOP('',(#18095,#18096,#18097,#18098,#18099));
#4601=EDGE_LOOP('',(#18100,#18101,#18102,#18103));
#4602=EDGE_LOOP('',(#18104,#18105,#18106,#18107));
#4603=EDGE_LOOP('',(#18108,#18109,#18110,#18111));
#4604=EDGE_LOOP('',(#18112,#18113,#18114,#18115,#18116,#18117,#18118,#18119,
#18120,#18121,#18122,#18123));
#4605=EDGE_LOOP('',(#18124,#18125,#18126,#18127,#18128,#18129,#18130,#18131,
#18132,#18133,#18134,#18135));
#4606=EDGE_LOOP('',(#18136,#18137,#18138,#18139));
#4607=EDGE_LOOP('',(#18140,#18141,#18142,#18143));
#4608=EDGE_LOOP('',(#18144));
#4609=EDGE_LOOP('',(#18145));
#4610=EDGE_LOOP('',(#18146));
#4611=EDGE_LOOP('',(#18147));
#4612=EDGE_LOOP('',(#18148,#18149,#18150,#18151));
#4613=EDGE_LOOP('',(#18152,#18153,#18154,#18155));
#4614=EDGE_LOOP('',(#18156,#18157,#18158,#18159));
#4615=EDGE_LOOP('',(#18160,#18161,#18162,#18163));
#4616=EDGE_LOOP('',(#18164,#18165,#18166,#18167));
#4617=EDGE_LOOP('',(#18168,#18169,#18170,#18171));
#4618=EDGE_LOOP('',(#18172,#18173,#18174,#18175));
#4619=EDGE_LOOP('',(#18176,#18177,#18178,#18179));
#4620=EDGE_LOOP('',(#18180,#18181,#18182,#18183));
#4621=EDGE_LOOP('',(#18184,#18185,#18186,#18187));
#4622=EDGE_LOOP('',(#18188,#18189,#18190,#18191));
#4623=EDGE_LOOP('',(#18192,#18193,#18194,#18195,#18196,#18197));
#4624=EDGE_LOOP('',(#18198,#18199,#18200,#18201));
#4625=EDGE_LOOP('',(#18202,#18203,#18204,#18205,#18206,#18207,#18208,#18209,
#18210,#18211,#18212,#18213,#18214,#18215));
#4626=EDGE_LOOP('',(#18216,#18217,#18218,#18219,#18220,#18221,#18222,#18223));
#4627=EDGE_LOOP('',(#18224,#18225,#18226,#18227,#18228,#18229,#18230,#18231));
#4628=EDGE_LOOP('',(#18232,#18233,#18234,#18235));
#4629=EDGE_LOOP('',(#18236,#18237,#18238,#18239));
#4630=EDGE_LOOP('',(#18240,#18241,#18242,#18243));
#4631=EDGE_LOOP('',(#18244,#18245,#18246,#18247));
#4632=EDGE_LOOP('',(#18248,#18249,#18250,#18251));
#4633=EDGE_LOOP('',(#18252,#18253,#18254,#18255));
#4634=EDGE_LOOP('',(#18256,#18257,#18258,#18259));
#4635=EDGE_LOOP('',(#18260,#18261,#18262,#18263));
#4636=EDGE_LOOP('',(#18264,#18265,#18266,#18267));
#4637=EDGE_LOOP('',(#18268,#18269,#18270,#18271,#18272,#18273,#18274,#18275,
#18276,#18277,#18278,#18279));
#4638=EDGE_LOOP('',(#18280,#18281,#18282,#18283,#18284,#18285,#18286,#18287,
#18288,#18289));
#4639=EDGE_LOOP('',(#18290,#18291,#18292,#18293,#18294,#18295,#18296,#18297));
#4640=EDGE_LOOP('',(#18298,#18299,#18300,#18301,#18302,#18303,#18304,#18305,
#18306,#18307,#18308,#18309,#18310));
#4641=EDGE_LOOP('',(#18311,#18312,#18313,#18314,#18315,#18316,#18317,#18318,
#18319,#18320,#18321,#18322,#18323,#18324,#18325,#18326,#18327,#18328,#18329,
#18330,#18331,#18332));
#4642=EDGE_LOOP('',(#18333,#18334,#18335,#18336,#18337,#18338,#18339,#18340,
#18341,#18342));
#4643=EDGE_LOOP('',(#18343,#18344,#18345,#18346,#18347,#18348,#18349,#18350));
#4644=EDGE_LOOP('',(#18351,#18352,#18353,#18354,#18355,#18356,#18357,#18358));
#4645=EDGE_LOOP('',(#18359,#18360,#18361,#18362,#18363));
#4646=EDGE_LOOP('',(#18364,#18365,#18366,#18367));
#4647=EDGE_LOOP('',(#18368,#18369,#18370,#18371));
#4648=EDGE_LOOP('',(#18372,#18373,#18374,#18375));
#4649=EDGE_LOOP('',(#18376,#18377,#18378,#18379,#18380,#18381,#18382,#18383,
#18384,#18385,#18386,#18387));
#4650=EDGE_LOOP('',(#18388,#18389,#18390,#18391,#18392));
#4651=EDGE_LOOP('',(#18393,#18394,#18395,#18396));
#4652=EDGE_LOOP('',(#18397,#18398,#18399,#18400));
#4653=EDGE_LOOP('',(#18401,#18402,#18403,#18404));
#4654=EDGE_LOOP('',(#18405,#18406,#18407,#18408,#18409,#18410,#18411,#18412,
#18413,#18414,#18415,#18416));
#4655=EDGE_LOOP('',(#18417,#18418,#18419,#18420));
#4656=EDGE_LOOP('',(#18421,#18422,#18423,#18424));
#4657=EDGE_LOOP('',(#18425,#18426,#18427,#18428));
#4658=EDGE_LOOP('',(#18429,#18430,#18431,#18432));
#4659=EDGE_LOOP('',(#18433,#18434,#18435,#18436));
#4660=EDGE_LOOP('',(#18437,#18438,#18439,#18440));
#4661=EDGE_LOOP('',(#18441,#18442,#18443,#18444));
#4662=EDGE_LOOP('',(#18445,#18446,#18447,#18448));
#4663=EDGE_LOOP('',(#18449,#18450,#18451,#18452));
#4664=EDGE_LOOP('',(#18453,#18454,#18455,#18456));
#4665=EDGE_LOOP('',(#18457,#18458,#18459,#18460,#18461,#18462,#18463,#18464,
#18465,#18466,#18467,#18468,#18469,#18470,#18471,#18472,#18473,#18474));
#4666=EDGE_LOOP('',(#18475,#18476,#18477,#18478,#18479,#18480,#18481,#18482,
#18483,#18484,#18485,#18486));
#4667=EDGE_LOOP('',(#18487,#18488,#18489,#18490,#18491,#18492));
#4668=EDGE_LOOP('',(#18493,#18494,#18495,#18496,#18497));
#4669=EDGE_LOOP('',(#18498,#18499,#18500,#18501,#18502));
#4670=EDGE_LOOP('',(#18503,#18504,#18505,#18506));
#4671=EDGE_LOOP('',(#18507,#18508,#18509,#18510));
#4672=EDGE_LOOP('',(#18511,#18512,#18513,#18514));
#4673=EDGE_LOOP('',(#18515,#18516,#18517,#18518));
#4674=EDGE_LOOP('',(#18519,#18520,#18521,#18522));
#4675=EDGE_LOOP('',(#18523,#18524,#18525,#18526));
#4676=EDGE_LOOP('',(#18527,#18528,#18529,#18530));
#4677=EDGE_LOOP('',(#18531,#18532,#18533,#18534));
#4678=EDGE_LOOP('',(#18535,#18536,#18537,#18538));
#4679=EDGE_LOOP('',(#18539,#18540,#18541,#18542));
#4680=EDGE_LOOP('',(#18543,#18544,#18545,#18546));
#4681=EDGE_LOOP('',(#18547,#18548,#18549,#18550,#18551,#18552,#18553,#18554,
#18555,#18556,#18557,#18558,#18559,#18560,#18561,#18562,#18563,#18564));
#4682=EDGE_LOOP('',(#18565,#18566,#18567,#18568,#18569,#18570));
#4683=EDGE_LOOP('',(#18571,#18572,#18573,#18574,#18575));
#4684=EDGE_LOOP('',(#18576,#18577,#18578,#18579,#18580));
#4685=EDGE_LOOP('',(#18581,#18582,#18583,#18584));
#4686=EDGE_LOOP('',(#18585,#18586,#18587,#18588,#18589,#18590));
#4687=EDGE_LOOP('',(#18591,#18592,#18593,#18594,#18595));
#4688=EDGE_LOOP('',(#18596,#18597,#18598,#18599,#18600));
#4689=EDGE_LOOP('',(#18601,#18602,#18603,#18604));
#4690=EDGE_LOOP('',(#18605,#18606,#18607,#18608,#18609));
#4691=EDGE_LOOP('',(#18610,#18611,#18612,#18613));
#4692=EDGE_LOOP('',(#18614,#18615,#18616,#18617));
#4693=EDGE_LOOP('',(#18618,#18619,#18620,#18621));
#4694=EDGE_LOOP('',(#18622,#18623,#18624,#18625,#18626,#18627,#18628,#18629,
#18630,#18631,#18632,#18633));
#4695=EDGE_LOOP('',(#18634,#18635,#18636,#18637,#18638,#18639));
#4696=EDGE_LOOP('',(#18640,#18641,#18642,#18643,#18644));
#4697=EDGE_LOOP('',(#18645,#18646,#18647,#18648,#18649));
#4698=EDGE_LOOP('',(#18650,#18651,#18652,#18653));
#4699=EDGE_LOOP('',(#18654,#18655,#18656,#18657));
#4700=EDGE_LOOP('',(#18658,#18659,#18660,#18661));
#4701=EDGE_LOOP('',(#18662,#18663,#18664,#18665));
#4702=EDGE_LOOP('',(#18666,#18667,#18668,#18669));
#4703=EDGE_LOOP('',(#18670,#18671,#18672,#18673));
#4704=EDGE_LOOP('',(#18674,#18675,#18676,#18677));
#4705=EDGE_LOOP('',(#18678,#18679,#18680,#18681));
#4706=EDGE_LOOP('',(#18682,#18683,#18684,#18685));
#4707=EDGE_LOOP('',(#18686,#18687,#18688,#18689,#18690,#18691));
#4708=EDGE_LOOP('',(#18692,#18693,#18694,#18695));
#4709=EDGE_LOOP('',(#18696,#18697,#18698,#18699,#18700,#18701,#18702,#18703,
#18704,#18705,#18706,#18707,#18708,#18709));
#4710=EDGE_LOOP('',(#18710,#18711,#18712,#18713,#18714,#18715,#18716,#18717));
#4711=EDGE_LOOP('',(#18718,#18719,#18720,#18721,#18722,#18723,#18724,#18725));
#4712=EDGE_LOOP('',(#18726,#18727,#18728,#18729));
#4713=EDGE_LOOP('',(#18730,#18731,#18732,#18733));
#4714=EDGE_LOOP('',(#18734,#18735,#18736,#18737));
#4715=EDGE_LOOP('',(#18738,#18739,#18740,#18741));
#4716=EDGE_LOOP('',(#18742,#18743,#18744,#18745));
#4717=EDGE_LOOP('',(#18746,#18747,#18748,#18749));
#4718=EDGE_LOOP('',(#18750,#18751,#18752,#18753));
#4719=EDGE_LOOP('',(#18754,#18755,#18756,#18757));
#4720=EDGE_LOOP('',(#18758,#18759,#18760,#18761));
#4721=EDGE_LOOP('',(#18762,#18763,#18764,#18765,#18766,#18767,#18768,#18769,
#18770,#18771,#18772,#18773));
#4722=EDGE_LOOP('',(#18774,#18775,#18776,#18777,#18778,#18779,#18780,#18781,
#18782,#18783,#18784,#18785));
#4723=EDGE_LOOP('',(#18786,#18787,#18788,#18789,#18790,#18791,#18792,#18793));
#4724=EDGE_LOOP('',(#18794,#18795,#18796,#18797,#18798,#18799,#18800,#18801));
#4725=EDGE_LOOP('',(#18802,#18803,#18804,#18805));
#4726=EDGE_LOOP('',(#18806,#18807,#18808,#18809,#18810));
#4727=EDGE_LOOP('',(#18811,#18812,#18813,#18814));
#4728=EDGE_LOOP('',(#18815,#18816,#18817,#18818));
#4729=EDGE_LOOP('',(#18819,#18820,#18821,#18822,#18823,#18824,#18825,#18826,
#18827,#18828,#18829,#18830));
#4730=EDGE_LOOP('',(#18831,#18832,#18833,#18834));
#4731=EDGE_LOOP('',(#18835,#18836,#18837,#18838));
#4732=EDGE_LOOP('',(#18839,#18840,#18841,#18842));
#4733=EDGE_LOOP('',(#18843,#18844,#18845,#18846));
#4734=EDGE_LOOP('',(#18847,#18848,#18849,#18850));
#4735=EDGE_LOOP('',(#18851,#18852,#18853,#18854));
#4736=EDGE_LOOP('',(#18855,#18856,#18857,#18858));
#4737=EDGE_LOOP('',(#18859,#18860,#18861,#18862));
#4738=EDGE_LOOP('',(#18863,#18864,#18865,#18866));
#4739=EDGE_LOOP('',(#18867,#18868,#18869,#18870));
#4740=EDGE_LOOP('',(#18871,#18872,#18873,#18874,#18875,#18876,#18877,#18878,
#18879,#18880,#18881,#18882,#18883,#18884,#18885,#18886,#18887));
#4741=EDGE_LOOP('',(#18888,#18889,#18890,#18891,#18892,#18893,#18894,#18895,
#18896,#18897,#18898,#18899));
#4742=EDGE_LOOP('',(#18900,#18901,#18902,#18903));
#4743=EDGE_LOOP('',(#18904,#18905,#18906,#18907));
#4744=EDGE_LOOP('',(#18908,#18909,#18910,#18911));
#4745=EDGE_LOOP('',(#18912,#18913,#18914,#18915));
#4746=EDGE_LOOP('',(#18916,#18917,#18918,#18919));
#4747=EDGE_LOOP('',(#18920,#18921,#18922,#18923));
#4748=EDGE_LOOP('',(#18924,#18925,#18926,#18927));
#4749=EDGE_LOOP('',(#18928,#18929,#18930,#18931));
#4750=EDGE_LOOP('',(#18932,#18933,#18934,#18935));
#4751=EDGE_LOOP('',(#18936,#18937,#18938,#18939));
#4752=EDGE_LOOP('',(#18940,#18941,#18942,#18943,#18944,#18945,#18946,#18947,
#18948,#18949,#18950,#18951,#18952,#18953,#18954,#18955,#18956));
#4753=EDGE_LOOP('',(#18957,#18958,#18959,#18960,#18961,#18962));
#4754=EDGE_LOOP('',(#18963,#18964,#18965,#18966,#18967));
#4755=EDGE_LOOP('',(#18968,#18969,#18970,#18971,#18972));
#4756=EDGE_LOOP('',(#18973,#18974,#18975,#18976));
#4757=EDGE_LOOP('',(#18977,#18978,#18979,#18980,#18981));
#4758=EDGE_LOOP('',(#18982,#18983,#18984,#18985));
#4759=EDGE_LOOP('',(#18986,#18987,#18988,#18989));
#4760=EDGE_LOOP('',(#18990,#18991,#18992,#18993));
#4761=EDGE_LOOP('',(#18994,#18995,#18996,#18997,#18998,#18999,#19000,#19001,
#19002,#19003,#19004,#19005));
#4762=EDGE_LOOP('',(#19006,#19007,#19008,#19009,#19010,#19011));
#4763=EDGE_LOOP('',(#19012,#19013,#19014,#19015,#19016));
#4764=EDGE_LOOP('',(#19017,#19018,#19019,#19020,#19021));
#4765=EDGE_LOOP('',(#19022,#19023,#19024,#19025));
#4766=EDGE_LOOP('',(#19026,#19027,#19028,#19029));
#4767=EDGE_LOOP('',(#19030,#19031,#19032,#19033,#19034));
#4768=EDGE_LOOP('',(#19035,#19036,#19037,#19038));
#4769=EDGE_LOOP('',(#19039,#19040,#19041,#19042));
#4770=EDGE_LOOP('',(#19043,#19044,#19045,#19046,#19047,#19048,#19049,#19050,
#19051,#19052,#19053,#19054));
#4771=EDGE_LOOP('',(#19055,#19056,#19057,#19058,#19059,#19060));
#4772=EDGE_LOOP('',(#19061,#19062,#19063,#19064,#19065));
#4773=EDGE_LOOP('',(#19066,#19067,#19068,#19069));
#4774=EDGE_LOOP('',(#19070,#19071,#19072,#19073));
#4775=EDGE_LOOP('',(#19074,#19075,#19076,#19077,#19078));
#4776=EDGE_LOOP('',(#19079,#19080,#19081,#19082));
#4777=EDGE_LOOP('',(#19083,#19084,#19085,#19086));
#4778=EDGE_LOOP('',(#19087,#19088,#19089,#19090));
#4779=EDGE_LOOP('',(#19091,#19092,#19093,#19094,#19095,#19096,#19097,#19098,
#19099,#19100,#19101,#19102));
#4780=EDGE_LOOP('',(#19103,#19104,#19105,#19106,#19107,#19108));
#4781=EDGE_LOOP('',(#19109,#19110,#19111,#19112,#19113));
#4782=EDGE_LOOP('',(#19114,#19115,#19116,#19117));
#4783=EDGE_LOOP('',(#19118,#19119,#19120,#19121));
#4784=EDGE_LOOP('',(#19122,#19123,#19124,#19125));
#4785=EDGE_LOOP('',(#19126,#19127,#19128,#19129));
#4786=EDGE_LOOP('',(#19130,#19131,#19132,#19133));
#4787=EDGE_LOOP('',(#19134));
#4788=EDGE_LOOP('',(#19135));
#4789=EDGE_LOOP('',(#19136,#19137,#19138,#19139));
#4790=EDGE_LOOP('',(#19140,#19141,#19142,#19143));
#4791=EDGE_LOOP('',(#19144));
#4792=EDGE_LOOP('',(#19145));
#4793=EDGE_LOOP('',(#19146,#19147,#19148,#19149));
#4794=EDGE_LOOP('',(#19150,#19151,#19152,#19153));
#4795=EDGE_LOOP('',(#19154,#19155,#19156,#19157));
#4796=EDGE_LOOP('',(#19158,#19159,#19160,#19161));
#4797=EDGE_LOOP('',(#19162,#19163,#19164,#19165));
#4798=EDGE_LOOP('',(#19166,#19167,#19168,#19169));
#4799=EDGE_LOOP('',(#19170,#19171,#19172,#19173));
#4800=EDGE_LOOP('',(#19174,#19175,#19176,#19177));
#4801=EDGE_LOOP('',(#19178,#19179,#19180,#19181));
#4802=EDGE_LOOP('',(#19182,#19183,#19184,#19185));
#4803=EDGE_LOOP('',(#19186,#19187,#19188,#19189));
#4804=EDGE_LOOP('',(#19190,#19191,#19192,#19193));
#4805=EDGE_LOOP('',(#19194,#19195,#19196,#19197));
#4806=EDGE_LOOP('',(#19198,#19199,#19200,#19201));
#4807=EDGE_LOOP('',(#19202,#19203,#19204,#19205));
#4808=EDGE_LOOP('',(#19206,#19207,#19208,#19209));
#4809=EDGE_LOOP('',(#19210,#19211,#19212,#19213));
#4810=EDGE_LOOP('',(#19214,#19215,#19216,#19217));
#4811=EDGE_LOOP('',(#19218,#19219,#19220,#19221));
#4812=EDGE_LOOP('',(#19222,#19223,#19224,#19225));
#4813=EDGE_LOOP('',(#19226,#19227,#19228,#19229));
#4814=EDGE_LOOP('',(#19230,#19231,#19232,#19233,#19234,#19235,#19236,#19237,
#19238,#19239));
#4815=EDGE_LOOP('',(#19240,#19241,#19242,#19243,#19244,#19245,#19246,#19247));
#4816=EDGE_LOOP('',(#19248,#19249,#19250,#19251));
#4817=EDGE_LOOP('',(#19252,#19253,#19254,#19255));
#4818=EDGE_LOOP('',(#19256,#19257,#19258,#19259));
#4819=EDGE_LOOP('',(#19260,#19261,#19262,#19263));
#4820=EDGE_LOOP('',(#19264,#19265,#19266,#19267));
#4821=EDGE_LOOP('',(#19268,#19269,#19270,#19271));
#4822=EDGE_LOOP('',(#19272,#19273,#19274,#19275));
#4823=EDGE_LOOP('',(#19276,#19277,#19278,#19279));
#4824=EDGE_LOOP('',(#19280,#19281,#19282,#19283,#19284,#19285,#19286,#19287));
#4825=EDGE_LOOP('',(#19288,#19289,#19290,#19291));
#4826=EDGE_LOOP('',(#19292,#19293,#19294,#19295));
#4827=EDGE_LOOP('',(#19296,#19297,#19298,#19299));
#4828=EDGE_LOOP('',(#19300,#19301,#19302,#19303));
#4829=EDGE_LOOP('',(#19304,#19305,#19306,#19307));
#4830=EDGE_LOOP('',(#19308,#19309,#19310,#19311));
#4831=EDGE_LOOP('',(#19312,#19313,#19314,#19315));
#4832=EDGE_LOOP('',(#19316,#19317,#19318,#19319));
#4833=EDGE_LOOP('',(#19320,#19321,#19322,#19323));
#4834=EDGE_LOOP('',(#19324,#19325,#19326,#19327));
#4835=EDGE_LOOP('',(#19328,#19329,#19330,#19331));
#4836=EDGE_LOOP('',(#19332,#19333,#19334,#19335));
#4837=EDGE_LOOP('',(#19336,#19337,#19338,#19339));
#4838=EDGE_LOOP('',(#19340,#19341,#19342,#19343));
#4839=EDGE_LOOP('',(#19344,#19345,#19346,#19347));
#4840=EDGE_LOOP('',(#19348,#19349,#19350,#19351));
#4841=EDGE_LOOP('',(#19352,#19353,#19354,#19355));
#4842=EDGE_LOOP('',(#19356,#19357,#19358,#19359));
#4843=EDGE_LOOP('',(#19360,#19361,#19362,#19363));
#4844=EDGE_LOOP('',(#19364,#19365,#19366,#19367));
#4845=EDGE_LOOP('',(#19368,#19369,#19370,#19371));
#4846=EDGE_LOOP('',(#19372,#19373,#19374,#19375));
#4847=EDGE_LOOP('',(#19376,#19377,#19378,#19379,#19380,#19381,#19382,#19383,
#19384,#19385,#19386,#19387,#19388));
#4848=EDGE_LOOP('',(#19389,#19390,#19391,#19392,#19393,#19394,#19395,#19396,
#19397));
#4849=EDGE_LOOP('',(#19398,#19399,#19400,#19401));
#4850=EDGE_LOOP('',(#19402,#19403,#19404,#19405));
#4851=EDGE_LOOP('',(#19406,#19407,#19408,#19409));
#4852=EDGE_LOOP('',(#19410,#19411,#19412,#19413));
#4853=EDGE_LOOP('',(#19414,#19415,#19416,#19417));
#4854=EDGE_LOOP('',(#19418,#19419,#19420,#19421));
#4855=EDGE_LOOP('',(#19422,#19423,#19424,#19425));
#4856=EDGE_LOOP('',(#19426,#19427,#19428,#19429));
#4857=EDGE_LOOP('',(#19430,#19431,#19432,#19433));
#4858=EDGE_LOOP('',(#19434,#19435,#19436,#19437));
#4859=EDGE_LOOP('',(#19438,#19439,#19440,#19441));
#4860=EDGE_LOOP('',(#19442,#19443,#19444,#19445));
#4861=EDGE_LOOP('',(#19446,#19447,#19448,#19449));
#4862=EDGE_LOOP('',(#19450,#19451,#19452,#19453));
#4863=EDGE_LOOP('',(#19454,#19455,#19456,#19457));
#4864=EDGE_LOOP('',(#19458,#19459,#19460,#19461));
#4865=EDGE_LOOP('',(#19462,#19463,#19464,#19465));
#4866=EDGE_LOOP('',(#19466,#19467,#19468,#19469));
#4867=EDGE_LOOP('',(#19470,#19471,#19472,#19473));
#4868=EDGE_LOOP('',(#19474,#19475,#19476,#19477));
#4869=EDGE_LOOP('',(#19478,#19479,#19480,#19481));
#4870=EDGE_LOOP('',(#19482,#19483,#19484,#19485));
#4871=EDGE_LOOP('',(#19486,#19487,#19488,#19489,#19490,#19491,#19492,#19493,
#19494,#19495,#19496,#19497,#19498,#19499,#19500,#19501,#19502,#19503,#19504,
#19505,#19506,#19507));
#4872=EDGE_LOOP('',(#19508,#19509,#19510,#19511));
#4873=EDGE_LOOP('',(#19512,#19513,#19514,#19515));
#4874=EDGE_LOOP('',(#19516,#19517,#19518,#19519));
#4875=EDGE_LOOP('',(#19520,#19521,#19522,#19523));
#4876=EDGE_LOOP('',(#19524,#19525,#19526,#19527));
#4877=EDGE_LOOP('',(#19528,#19529,#19530,#19531));
#4878=EDGE_LOOP('',(#19532,#19533,#19534,#19535));
#4879=EDGE_LOOP('',(#19536,#19537,#19538,#19539));
#4880=EDGE_LOOP('',(#19540,#19541,#19542,#19543));
#4881=EDGE_LOOP('',(#19544,#19545,#19546,#19547));
#4882=EDGE_LOOP('',(#19548,#19549,#19550,#19551,#19552,#19553,#19554,#19555,
#19556,#19557));
#4883=EDGE_LOOP('',(#19558,#19559,#19560,#19561,#19562,#19563,#19564,#19565,
#19566));
#4884=EDGE_LOOP('',(#19567,#19568,#19569,#19570,#19571,#19572,#19573,#19574));
#4885=EDGE_LOOP('',(#19575,#19576,#19577,#19578));
#4886=EDGE_LOOP('',(#19579,#19580,#19581,#19582,#19583,#19584,#19585,#19586));
#4887=EDGE_LOOP('',(#19587,#19588,#19589,#19590));
#4888=EDGE_LOOP('',(#19591,#19592,#19593,#19594));
#4889=EDGE_LOOP('',(#19595,#19596,#19597,#19598));
#4890=EDGE_LOOP('',(#19599,#19600,#19601,#19602));
#4891=EDGE_LOOP('',(#19603,#19604,#19605,#19606));
#4892=EDGE_LOOP('',(#19607,#19608,#19609,#19610,#19611));
#4893=EDGE_LOOP('',(#19612,#19613,#19614,#19615));
#4894=EDGE_LOOP('',(#19616,#19617,#19618,#19619));
#4895=EDGE_LOOP('',(#19620,#19621,#19622,#19623,#19624,#19625));
#4896=EDGE_LOOP('',(#19626,#19627,#19628,#19629,#19630));
#4897=EDGE_LOOP('',(#19631,#19632,#19633,#19634));
#4898=EDGE_LOOP('',(#19635,#19636,#19637,#19638,#19639));
#4899=EDGE_LOOP('',(#19640,#19641,#19642,#19643,#19644,#19645));
#4900=EDGE_LOOP('',(#19646,#19647,#19648,#19649));
#4901=EDGE_LOOP('',(#19650,#19651,#19652,#19653));
#4902=EDGE_LOOP('',(#19654,#19655,#19656,#19657));
#4903=EDGE_LOOP('',(#19658,#19659,#19660,#19661,#19662,#19663));
#4904=EDGE_LOOP('',(#19664,#19665,#19666,#19667,#19668,#19669));
#4905=EDGE_LOOP('',(#19670,#19671,#19672,#19673,#19674));
#4906=EDGE_LOOP('',(#19675,#19676,#19677,#19678,#19679,#19680));
#4907=EDGE_LOOP('',(#19681,#19682,#19683,#19684,#19685,#19686,#19687,#19688));
#4908=EDGE_LOOP('',(#19689,#19690,#19691,#19692,#19693));
#4909=EDGE_LOOP('',(#19694,#19695,#19696,#19697,#19698));
#4910=EDGE_LOOP('',(#19699,#19700,#19701,#19702,#19703,#19704,#19705,#19706));
#4911=EDGE_LOOP('',(#19707,#19708,#19709,#19710,#19711,#19712));
#4912=EDGE_LOOP('',(#19713,#19714,#19715,#19716,#19717,#19718));
#4913=EDGE_LOOP('',(#19719,#19720,#19721,#19722,#19723));
#4914=EDGE_LOOP('',(#19724,#19725,#19726,#19727,#19728,#19729));
#4915=EDGE_LOOP('',(#19730,#19731,#19732,#19733,#19734,#19735));
#4916=EDGE_LOOP('',(#19736,#19737,#19738,#19739,#19740));
#4917=EDGE_LOOP('',(#19741,#19742,#19743,#19744,#19745,#19746));
#4918=EDGE_LOOP('',(#19747,#19748,#19749,#19750,#19751,#19752,#19753,#19754));
#4919=EDGE_LOOP('',(#19755,#19756,#19757,#19758,#19759));
#4920=EDGE_LOOP('',(#19760,#19761,#19762,#19763,#19764));
#4921=EDGE_LOOP('',(#19765,#19766,#19767,#19768,#19769));
#4922=EDGE_LOOP('',(#19770,#19771,#19772,#19773));
#4923=EDGE_LOOP('',(#19774,#19775,#19776,#19777,#19778,#19779,#19780,#19781,
#19782,#19783));
#4924=EDGE_LOOP('',(#19784,#19785,#19786,#19787,#19788,#19789));
#4925=EDGE_LOOP('',(#19790,#19791,#19792));
#4926=EDGE_LOOP('',(#19793,#19794,#19795,#19796,#19797));
#4927=EDGE_LOOP('',(#19798,#19799,#19800,#19801));
#4928=EDGE_LOOP('',(#19802,#19803,#19804,#19805,#19806,#19807,#19808,#19809));
#4929=EDGE_LOOP('',(#19810,#19811,#19812,#19813,#19814,#19815));
#4930=EDGE_LOOP('',(#19816,#19817,#19818,#19819,#19820));
#4931=EDGE_LOOP('',(#19821,#19822,#19823,#19824,#19825,#19826,#19827,#19828,
#19829,#19830,#19831,#19832,#19833,#19834,#19835,#19836));
#4932=EDGE_LOOP('',(#19837,#19838,#19839,#19840,#19841));
#4933=EDGE_LOOP('',(#19842,#19843,#19844,#19845,#19846,#19847));
#4934=EDGE_LOOP('',(#19848,#19849,#19850,#19851,#19852,#19853));
#4935=EDGE_LOOP('',(#19854,#19855,#19856,#19857,#19858));
#4936=EDGE_LOOP('',(#19859,#19860,#19861,#19862,#19863));
#4937=EDGE_LOOP('',(#19864,#19865,#19866,#19867,#19868,#19869));
#4938=EDGE_LOOP('',(#19870,#19871,#19872,#19873,#19874,#19875));
#4939=EDGE_LOOP('',(#19876,#19877,#19878,#19879));
#4940=EDGE_LOOP('',(#19880,#19881,#19882,#19883,#19884,#19885,#19886,#19887,
#19888,#19889));
#4941=EDGE_LOOP('',(#19890,#19891,#19892,#19893,#19894));
#4942=EDGE_LOOP('',(#19895,#19896,#19897,#19898,#19899,#19900));
#4943=EDGE_LOOP('',(#19901,#19902,#19903,#19904,#19905));
#4944=EDGE_LOOP('',(#19906,#19907,#19908,#19909));
#4945=EDGE_LOOP('',(#19910,#19911,#19912,#19913,#19914));
#4946=EDGE_LOOP('',(#19915,#19916,#19917,#19918,#19919,#19920,#19921,#19922));
#4947=EDGE_LOOP('',(#19923,#19924,#19925,#19926,#19927,#19928));
#4948=EDGE_LOOP('',(#19929,#19930,#19931,#19932));
#4949=EDGE_LOOP('',(#19933,#19934,#19935,#19936));
#4950=EDGE_LOOP('',(#19937,#19938,#19939,#19940,#19941));
#4951=EDGE_LOOP('',(#19942,#19943,#19944,#19945,#19946,#19947,#19948,#19949));
#4952=EDGE_LOOP('',(#19950,#19951,#19952,#19953,#19954));
#4953=EDGE_LOOP('',(#19955,#19956,#19957,#19958,#19959,#19960));
#4954=EDGE_LOOP('',(#19961,#19962,#19963,#19964,#19965));
#4955=EDGE_LOOP('',(#19966,#19967,#19968,#19969,#19970));
#4956=EDGE_LOOP('',(#19971,#19972,#19973,#19974));
#4957=EDGE_LOOP('',(#19975,#19976,#19977,#19978,#19979));
#4958=EDGE_LOOP('',(#19980,#19981,#19982,#19983));
#4959=EDGE_LOOP('',(#19984,#19985,#19986,#19987,#19988,#19989,#19990,#19991,
#19992,#19993));
#4960=EDGE_LOOP('',(#19994,#19995,#19996,#19997));
#4961=EDGE_LOOP('',(#19998,#19999,#20000,#20001));
#4962=EDGE_LOOP('',(#20002));
#4963=EDGE_LOOP('',(#20003));
#4964=EDGE_LOOP('',(#20004,#20005,#20006,#20007,#20008));
#4965=EDGE_LOOP('',(#20009,#20010,#20011,#20012,#20013,#20014,#20015,#20016,
#20017,#20018,#20019,#20020,#20021,#20022,#20023,#20024));
#4966=EDGE_LOOP('',(#20025,#20026,#20027,#20028,#20029));
#4967=EDGE_LOOP('',(#20030,#20031,#20032,#20033,#20034,#20035));
#4968=EDGE_LOOP('',(#20036,#20037,#20038,#20039,#20040,#20041));
#4969=EDGE_LOOP('',(#20042,#20043,#20044,#20045));
#4970=EDGE_LOOP('',(#20046,#20047,#20048,#20049,#20050,#20051));
#4971=EDGE_LOOP('',(#20052,#20053,#20054,#20055,#20056));
#4972=EDGE_LOOP('',(#20057,#20058,#20059,#20060,#20061));
#4973=EDGE_LOOP('',(#20062,#20063,#20064,#20065,#20066));
#4974=EDGE_LOOP('',(#20067,#20068,#20069,#20070));
#4975=EDGE_LOOP('',(#20071,#20072,#20073,#20074,#20075,#20076,#20077,#20078));
#4976=EDGE_LOOP('',(#20079,#20080,#20081,#20082,#20083,#20084));
#4977=EDGE_LOOP('',(#20085,#20086,#20087));
#4978=EDGE_LOOP('',(#20088,#20089,#20090,#20091));
#4979=EDGE_LOOP('',(#20092,#20093,#20094,#20095,#20096));
#4980=EDGE_LOOP('',(#20097,#20098,#20099,#20100));
#4981=EDGE_LOOP('',(#20101,#20102,#20103,#20104,#20105));
#4982=EDGE_LOOP('',(#20106,#20107,#20108,#20109,#20110,#20111));
#4983=EDGE_LOOP('',(#20112,#20113,#20114,#20115,#20116));
#4984=EDGE_LOOP('',(#20117,#20118,#20119,#20120));
#4985=EDGE_LOOP('',(#20121,#20122,#20123,#20124,#20125,#20126,#20127,#20128));
#4986=EDGE_LOOP('',(#20129,#20130,#20131,#20132,#20133));
#4987=EDGE_LOOP('',(#20134,#20135,#20136,#20137,#20138,#20139));
#4988=EDGE_LOOP('',(#20140,#20141,#20142,#20143,#20144,#20145));
#4989=EDGE_LOOP('',(#20146,#20147,#20148,#20149,#20150));
#4990=EDGE_LOOP('',(#20151,#20152,#20153,#20154,#20155,#20156));
#4991=EDGE_LOOP('',(#20157,#20158,#20159,#20160,#20161,#20162));
#4992=EDGE_LOOP('',(#20163,#20164,#20165,#20166,#20167,#20168));
#4993=EDGE_LOOP('',(#20169,#20170,#20171,#20172,#20173,#20174));
#4994=EDGE_LOOP('',(#20175,#20176,#20177,#20178,#20179));
#4995=EDGE_LOOP('',(#20180,#20181,#20182,#20183,#20184));
#4996=EDGE_LOOP('',(#20185));
#4997=EDGE_LOOP('',(#20186,#20187,#20188,#20189));
#4998=EDGE_LOOP('',(#20190,#20191,#20192,#20193));
#4999=EDGE_LOOP('',(#20194,#20195,#20196,#20197));
#5000=EDGE_LOOP('',(#20198,#20199,#20200,#20201));
#5001=EDGE_LOOP('',(#20202));
#5002=EDGE_LOOP('',(#20203));
#5003=EDGE_LOOP('',(#20204,#20205,#20206,#20207));
#5004=EDGE_LOOP('',(#20208,#20209,#20210,#20211));
#5005=EDGE_LOOP('',(#20212,#20213,#20214,#20215));
#5006=EDGE_LOOP('',(#20216,#20217,#20218,#20219));
#5007=EDGE_LOOP('',(#20220,#20221,#20222,#20223));
#5008=EDGE_LOOP('',(#20224,#20225,#20226,#20227));
#5009=EDGE_LOOP('',(#20228,#20229,#20230,#20231));
#5010=EDGE_LOOP('',(#20232));
#5011=EDGE_LOOP('',(#20233,#20234,#20235,#20236));
#5012=EDGE_LOOP('',(#20237,#20238,#20239,#20240,#20241,#20242,#20243,#20244,
#20245,#20246));
#5013=EDGE_LOOP('',(#20247,#20248,#20249,#20250));
#5014=EDGE_LOOP('',(#20251,#20252,#20253,#20254));
#5015=EDGE_LOOP('',(#20255,#20256,#20257,#20258));
#5016=EDGE_LOOP('',(#20259,#20260,#20261,#20262,#20263,#20264));
#5017=EDGE_LOOP('',(#20265,#20266,#20267,#20268));
#5018=EDGE_LOOP('',(#20269,#20270,#20271,#20272,#20273,#20274));
#5019=EDGE_LOOP('',(#20275,#20276,#20277,#20278,#20279,#20280));
#5020=EDGE_LOOP('',(#20281,#20282,#20283,#20284));
#5021=EDGE_LOOP('',(#20285,#20286,#20287,#20288));
#5022=EDGE_LOOP('',(#20289,#20290,#20291,#20292));
#5023=EDGE_LOOP('',(#20293,#20294,#20295,#20296));
#5024=EDGE_LOOP('',(#20297,#20298,#20299,#20300,#20301,#20302));
#5025=EDGE_LOOP('',(#20303,#20304,#20305,#20306,#20307,#20308));
#5026=EDGE_LOOP('',(#20309,#20310,#20311,#20312));
#5027=EDGE_LOOP('',(#20313,#20314,#20315,#20316,#20317,#20318));
#5028=EDGE_LOOP('',(#20319,#20320,#20321,#20322,#20323,#20324));
#5029=EDGE_LOOP('',(#20325,#20326,#20327,#20328,#20329));
#5030=EDGE_LOOP('',(#20330,#20331,#20332,#20333));
#5031=EDGE_LOOP('',(#20334,#20335,#20336,#20337,#20338,#20339));
#5032=EDGE_LOOP('',(#20340,#20341,#20342,#20343,#20344));
#5033=EDGE_LOOP('',(#20345,#20346,#20347,#20348));
#5034=EDGE_LOOP('',(#20349,#20350,#20351,#20352));
#5035=EDGE_LOOP('',(#20353,#20354,#20355,#20356));
#5036=EDGE_LOOP('',(#20357,#20358,#20359,#20360));
#5037=EDGE_LOOP('',(#20361,#20362,#20363,#20364));
#5038=EDGE_LOOP('',(#20365,#20366,#20367));
#5039=EDGE_LOOP('',(#20368,#20369,#20370,#20371,#20372));
#5040=EDGE_LOOP('',(#20373,#20374,#20375));
#5041=EDGE_LOOP('',(#20376,#20377,#20378,#20379,#20380));
#5042=EDGE_LOOP('',(#20381,#20382,#20383,#20384,#20385));
#5043=EDGE_LOOP('',(#20386,#20387,#20388,#20389));
#5044=EDGE_LOOP('',(#20390,#20391,#20392,#20393));
#5045=EDGE_LOOP('',(#20394,#20395,#20396,#20397));
#5046=EDGE_LOOP('',(#20398,#20399,#20400,#20401,#20402));
#5047=EDGE_LOOP('',(#20403,#20404,#20405,#20406,#20407,#20408,#20409,#20410,
#20411,#20412,#20413,#20414,#20415,#20416,#20417,#20418,#20419,#20420,#20421,
#20422));
#5048=EDGE_LOOP('',(#20423,#20424,#20425,#20426,#20427,#20428));
#5049=EDGE_LOOP('',(#20429,#20430,#20431,#20432,#20433));
#5050=EDGE_LOOP('',(#20434,#20435,#20436,#20437));
#5051=EDGE_LOOP('',(#20438,#20439,#20440,#20441,#20442));
#5052=EDGE_LOOP('',(#20443,#20444,#20445,#20446));
#5053=EDGE_LOOP('',(#20447,#20448,#20449,#20450,#20451));
#5054=EDGE_LOOP('',(#20452,#20453,#20454,#20455));
#5055=EDGE_LOOP('',(#20456,#20457,#20458));
#5056=EDGE_LOOP('',(#20459,#20460,#20461,#20462,#20463));
#5057=EDGE_LOOP('',(#20464,#20465,#20466,#20467));
#5058=EDGE_LOOP('',(#20468,#20469,#20470,#20471,#20472));
#5059=EDGE_LOOP('',(#20473,#20474,#20475,#20476));
#5060=EDGE_LOOP('',(#20477,#20478,#20479,#20480,#20481,#20482,#20483,#20484,
#20485,#20486,#20487,#20488,#20489,#20490,#20491,#20492));
#5061=EDGE_LOOP('',(#20493,#20494,#20495,#20496,#20497));
#5062=EDGE_LOOP('',(#20498,#20499,#20500,#20501,#20502,#20503));
#5063=EDGE_LOOP('',(#20504,#20505,#20506,#20507));
#5064=EDGE_LOOP('',(#20508,#20509,#20510,#20511));
#5065=EDGE_LOOP('',(#20512,#20513,#20514,#20515,#20516,#20517));
#5066=EDGE_LOOP('',(#20518,#20519,#20520,#20521,#20522,#20523));
#5067=EDGE_LOOP('',(#20524,#20525,#20526,#20527,#20528,#20529));
#5068=EDGE_LOOP('',(#20530,#20531,#20532,#20533,#20534));
#5069=EDGE_LOOP('',(#20535,#20536,#20537,#20538));
#5070=EDGE_LOOP('',(#20539,#20540,#20541,#20542));
#5071=EDGE_LOOP('',(#20543,#20544,#20545,#20546,#20547));
#5072=EDGE_LOOP('',(#20548,#20549,#20550,#20551,#20552,#20553));
#5073=EDGE_LOOP('',(#20554,#20555,#20556,#20557));
#5074=EDGE_LOOP('',(#20558,#20559,#20560,#20561,#20562));
#5075=EDGE_LOOP('',(#20563,#20564,#20565,#20566,#20567,#20568,#20569,#20570,
#20571,#20572,#20573,#20574,#20575,#20576,#20577,#20578,#20579,#20580,#20581,
#20582));
#5076=EDGE_LOOP('',(#20583,#20584,#20585,#20586));
#5077=EDGE_LOOP('',(#20587,#20588,#20589,#20590));
#5078=EDGE_LOOP('',(#20591,#20592,#20593));
#5079=EDGE_LOOP('',(#20594,#20595,#20596,#20597));
#5080=EDGE_LOOP('',(#20598,#20599,#20600,#20601,#20602));
#5081=EDGE_LOOP('',(#20603,#20604,#20605,#20606,#20607));
#5082=EDGE_LOOP('',(#20608,#20609,#20610,#20611));
#5083=EDGE_LOOP('',(#20612,#20613,#20614,#20615,#20616,#20617));
#5084=EDGE_LOOP('',(#20618,#20619,#20620,#20621));
#5085=EDGE_LOOP('',(#20622,#20623,#20624,#20625,#20626,#20627,#20628,#20629,
#20630,#20631,#20632,#20633,#20634,#20635,#20636,#20637));
#5086=EDGE_LOOP('',(#20638,#20639,#20640,#20641,#20642,#20643));
#5087=EDGE_LOOP('',(#20644,#20645,#20646,#20647));
#5088=EDGE_LOOP('',(#20648,#20649,#20650,#20651,#20652));
#5089=EDGE_LOOP('',(#20653,#20654,#20655,#20656,#20657));
#5090=EDGE_LOOP('',(#20658,#20659,#20660,#20661));
#5091=EDGE_LOOP('',(#20662,#20663,#20664,#20665));
#5092=EDGE_LOOP('',(#20666,#20667,#20668,#20669,#20670,#20671));
#5093=EDGE_LOOP('',(#20672,#20673,#20674,#20675,#20676));
#5094=EDGE_LOOP('',(#20677,#20678,#20679,#20680,#20681,#20682));
#5095=EDGE_LOOP('',(#20683,#20684,#20685,#20686,#20687,#20688));
#5096=EDGE_LOOP('',(#20689,#20690,#20691,#20692));
#5097=EDGE_LOOP('',(#20693,#20694,#20695,#20696));
#5098=EDGE_LOOP('',(#20697,#20698,#20699,#20700));
#5099=EDGE_LOOP('',(#20701,#20702,#20703,#20704));
#5100=EDGE_LOOP('',(#20705,#20706,#20707,#20708));
#5101=EDGE_LOOP('',(#20709,#20710,#20711,#20712));
#5102=EDGE_LOOP('',(#20713,#20714,#20715,#20716));
#5103=EDGE_LOOP('',(#20717,#20718,#20719,#20720));
#5104=EDGE_LOOP('',(#20721,#20722,#20723,#20724));
#5105=EDGE_LOOP('',(#20725,#20726,#20727,#20728));
#5106=EDGE_LOOP('',(#20729,#20730,#20731,#20732));
#5107=EDGE_LOOP('',(#20733,#20734,#20735,#20736));
#5108=EDGE_LOOP('',(#20737,#20738,#20739,#20740));
#5109=EDGE_LOOP('',(#20741,#20742,#20743,#20744));
#5110=EDGE_LOOP('',(#20745,#20746,#20747,#20748));
#5111=EDGE_LOOP('',(#20749,#20750,#20751,#20752));
#5112=EDGE_LOOP('',(#20753,#20754,#20755,#20756));
#5113=EDGE_LOOP('',(#20757,#20758,#20759,#20760));
#5114=EDGE_LOOP('',(#20761,#20762,#20763,#20764));
#5115=EDGE_LOOP('',(#20765,#20766,#20767,#20768));
#5116=EDGE_LOOP('',(#20769,#20770,#20771,#20772));
#5117=EDGE_LOOP('',(#20773,#20774,#20775,#20776));
#5118=EDGE_LOOP('',(#20777,#20778,#20779,#20780));
#5119=EDGE_LOOP('',(#20781,#20782,#20783,#20784));
#5120=EDGE_LOOP('',(#20785,#20786,#20787,#20788));
#5121=EDGE_LOOP('',(#20789,#20790,#20791,#20792));
#5122=EDGE_LOOP('',(#20793,#20794,#20795,#20796));
#5123=EDGE_LOOP('',(#20797,#20798,#20799,#20800,#20801,#20802));
#5124=EDGE_LOOP('',(#20803,#20804,#20805,#20806));
#5125=EDGE_LOOP('',(#20807,#20808,#20809,#20810));
#5126=EDGE_LOOP('',(#20811,#20812,#20813,#20814,#20815,#20816));
#5127=EDGE_LOOP('',(#20817,#20818,#20819,#20820,#20821,#20822));
#5128=EDGE_LOOP('',(#20823,#20824,#20825,#20826));
#5129=EDGE_LOOP('',(#20827,#20828,#20829,#20830,#20831,#20832));
#5130=EDGE_LOOP('',(#20833,#20834,#20835,#20836,#20837,#20838));
#5131=EDGE_LOOP('',(#20839,#20840,#20841,#20842,#20843,#20844));
#5132=EDGE_LOOP('',(#20845,#20846,#20847,#20848,#20849,#20850));
#5133=EDGE_LOOP('',(#20851,#20852,#20853,#20854,#20855));
#5134=EDGE_LOOP('',(#20856,#20857,#20858,#20859));
#5135=EDGE_LOOP('',(#20860));
#5136=EDGE_LOOP('',(#20861));
#5137=EDGE_LOOP('',(#20862,#20863,#20864,#20865,#20866,#20867));
#5138=EDGE_LOOP('',(#20868,#20869,#20870,#20871,#20872,#20873));
#5139=EDGE_LOOP('',(#20874,#20875,#20876,#20877));
#5140=EDGE_LOOP('',(#20878));
#5141=EDGE_LOOP('',(#20879));
#5142=EDGE_LOOP('',(#20880,#20881,#20882,#20883,#20884,#20885));
#5143=EDGE_LOOP('',(#20886,#20887,#20888,#20889,#20890,#20891));
#5144=EDGE_LOOP('',(#20892,#20893,#20894,#20895,#20896,#20897));
#5145=EDGE_LOOP('',(#20898,#20899,#20900,#20901));
#5146=EDGE_LOOP('',(#20902,#20903,#20904,#20905));
#5147=EDGE_LOOP('',(#20906,#20907,#20908,#20909));
#5148=EDGE_LOOP('',(#20910,#20911,#20912,#20913));
#5149=EDGE_LOOP('',(#20914,#20915,#20916,#20917));
#5150=EDGE_LOOP('',(#20918,#20919,#20920,#20921));
#5151=EDGE_LOOP('',(#20922,#20923,#20924,#20925,#20926));
#5152=EDGE_LOOP('',(#20927,#20928,#20929,#20930,#20931));
#5153=EDGE_LOOP('',(#20932,#20933,#20934,#20935,#20936,#20937));
#5154=EDGE_LOOP('',(#20938,#20939,#20940,#20941));
#5155=EDGE_LOOP('',(#20942,#20943,#20944,#20945,#20946,#20947));
#5156=EDGE_LOOP('',(#20948,#20949,#20950,#20951,#20952,#20953));
#5157=EDGE_LOOP('',(#20954,#20955,#20956,#20957,#20958));
#5158=EDGE_LOOP('',(#20959,#20960,#20961,#20962));
#5159=EDGE_LOOP('',(#20963,#20964,#20965,#20966,#20967,#20968));
#5160=EDGE_LOOP('',(#20969,#20970,#20971,#20972));
#5161=EDGE_LOOP('',(#20973,#20974,#20975,#20976));
#5162=EDGE_LOOP('',(#20977,#20978,#20979,#20980));
#5163=EDGE_LOOP('',(#20981,#20982,#20983,#20984));
#5164=EDGE_LOOP('',(#20985,#20986,#20987,#20988));
#5165=EDGE_LOOP('',(#20989,#20990,#20991,#20992));
#5166=EDGE_LOOP('',(#20993,#20994,#20995,#20996));
#5167=EDGE_LOOP('',(#20997,#20998,#20999,#21000));
#5168=EDGE_LOOP('',(#21001,#21002,#21003,#21004));
#5169=EDGE_LOOP('',(#21005,#21006,#21007,#21008));
#5170=EDGE_LOOP('',(#21009,#21010,#21011,#21012));
#5171=EDGE_LOOP('',(#21013,#21014,#21015,#21016));
#5172=EDGE_LOOP('',(#21017,#21018,#21019,#21020));
#5173=EDGE_LOOP('',(#21021,#21022,#21023,#21024,#21025,#21026,#21027,#21028));
#5174=EDGE_LOOP('',(#21029));
#5175=EDGE_LOOP('',(#21030));
#5176=EDGE_LOOP('',(#21031));
#5177=EDGE_LOOP('',(#21032,#21033,#21034,#21035));
#5178=EDGE_LOOP('',(#21036,#21037,#21038,#21039));
#5179=EDGE_LOOP('',(#21040,#21041,#21042,#21043));
#5180=EDGE_LOOP('',(#21044,#21045,#21046,#21047));
#5181=EDGE_LOOP('',(#21048,#21049,#21050,#21051));
#5182=EDGE_LOOP('',(#21052,#21053,#21054,#21055));
#5183=EDGE_LOOP('',(#21056,#21057,#21058,#21059));
#5184=EDGE_LOOP('',(#21060,#21061,#21062,#21063));
#5185=EDGE_LOOP('',(#21064,#21065,#21066,#21067));
#5186=EDGE_LOOP('',(#21068,#21069,#21070,#21071));
#5187=EDGE_LOOP('',(#21072,#21073,#21074,#21075));
#5188=EDGE_LOOP('',(#21076,#21077,#21078,#21079));
#5189=EDGE_LOOP('',(#21080,#21081,#21082,#21083));
#5190=EDGE_LOOP('',(#21084,#21085,#21086,#21087));
#5191=EDGE_LOOP('',(#21088,#21089,#21090,#21091));
#5192=EDGE_LOOP('',(#21092));
#5193=EDGE_LOOP('',(#21093,#21094,#21095,#21096));
#5194=EDGE_LOOP('',(#21097,#21098,#21099,#21100));
#5195=EDGE_LOOP('',(#21101,#21102,#21103,#21104));
#5196=EDGE_LOOP('',(#21105,#21106,#21107,#21108));
#5197=EDGE_LOOP('',(#21109,#21110,#21111,#21112));
#5198=EDGE_LOOP('',(#21113,#21114,#21115,#21116));
#5199=EDGE_LOOP('',(#21117,#21118,#21119,#21120));
#5200=EDGE_LOOP('',(#21121,#21122,#21123,#21124));
#5201=EDGE_LOOP('',(#21125,#21126,#21127,#21128,#21129,#21130,#21131,#21132));
#5202=EDGE_LOOP('',(#21133,#21134,#21135,#21136));
#5203=EDGE_LOOP('',(#21137,#21138,#21139,#21140));
#5204=EDGE_LOOP('',(#21141,#21142,#21143,#21144));
#5205=EDGE_LOOP('',(#21145,#21146,#21147,#21148));
#5206=EDGE_LOOP('',(#21149,#21150,#21151,#21152));
#5207=EDGE_LOOP('',(#21153,#21154,#21155,#21156,#21157,#21158));
#5208=EDGE_LOOP('',(#21159));
#5209=EDGE_LOOP('',(#21160,#21161,#21162,#21163));
#5210=EDGE_LOOP('',(#21164,#21165,#21166,#21167));
#5211=EDGE_LOOP('',(#21168,#21169,#21170,#21171));
#5212=EDGE_LOOP('',(#21172,#21173,#21174,#21175));
#5213=EDGE_LOOP('',(#21176,#21177,#21178,#21179));
#5214=EDGE_LOOP('',(#21180,#21181,#21182,#21183,#21184,#21185));
#5215=EDGE_LOOP('',(#21186));
#5216=EDGE_LOOP('',(#21187,#21188,#21189,#21190));
#5217=EDGE_LOOP('',(#21191,#21192,#21193,#21194));
#5218=EDGE_LOOP('',(#21195,#21196,#21197,#21198));
#5219=EDGE_LOOP('',(#21199,#21200,#21201,#21202));
#5220=EDGE_LOOP('',(#21203,#21204,#21205,#21206));
#5221=EDGE_LOOP('',(#21207,#21208,#21209,#21210,#21211));
#5222=EDGE_LOOP('',(#21212,#21213,#21214,#21215));
#5223=EDGE_LOOP('',(#21216,#21217,#21218,#21219));
#5224=EDGE_LOOP('',(#21220,#21221,#21222,#21223));
#5225=EDGE_LOOP('',(#21224,#21225,#21226,#21227,#21228));
#5226=EDGE_LOOP('',(#21229,#21230,#21231,#21232));
#5227=EDGE_LOOP('',(#21233,#21234,#21235,#21236));
#5228=EDGE_LOOP('',(#21237));
#5229=EDGE_LOOP('',(#21238));
#5230=EDGE_LOOP('',(#21239,#21240,#21241,#21242));
#5231=EDGE_LOOP('',(#21243,#21244,#21245,#21246));
#5232=EDGE_LOOP('',(#21247,#21248,#21249,#21250));
#5233=EDGE_LOOP('',(#21251,#21252,#21253,#21254));
#5234=EDGE_LOOP('',(#21255,#21256,#21257,#21258));
#5235=EDGE_LOOP('',(#21259,#21260,#21261));
#5236=EDGE_LOOP('',(#21262,#21263,#21264));
#5237=EDGE_LOOP('',(#21265,#21266,#21267,#21268));
#5238=EDGE_LOOP('',(#21269,#21270,#21271,#21272));
#5239=EDGE_LOOP('',(#21273,#21274,#21275,#21276));
#5240=EDGE_LOOP('',(#21277,#21278,#21279,#21280));
#5241=EDGE_LOOP('',(#21281,#21282,#21283,#21284));
#5242=EDGE_LOOP('',(#21285,#21286,#21287,#21288,#21289));
#5243=EDGE_LOOP('',(#21290,#21291,#21292,#21293,#21294));
#5244=EDGE_LOOP('',(#21295,#21296));
#5245=EDGE_LOOP('',(#21297,#21298,#21299,#21300));
#5246=EDGE_LOOP('',(#21301,#21302,#21303,#21304,#21305,#21306,#21307,#21308));
#5247=EDGE_LOOP('',(#21309,#21310));
#5248=EDGE_LOOP('',(#21311,#21312,#21313,#21314,#21315,#21316,#21317,#21318,
#21319,#21320,#21321,#21322,#21323));
#5249=EDGE_LOOP('',(#21324,#21325,#21326,#21327,#21328,#21329,#21330,#21331,
#21332,#21333,#21334,#21335));
#5250=EDGE_LOOP('',(#21336,#21337,#21338,#21339));
#5251=EDGE_LOOP('',(#21340,#21341,#21342,#21343));
#5252=EDGE_LOOP('',(#21344,#21345,#21346,#21347));
#5253=EDGE_LOOP('',(#21348));
#5254=EDGE_LOOP('',(#21349));
#5255=EDGE_LOOP('',(#21350,#21351,#21352,#21353));
#5256=EDGE_LOOP('',(#21354,#21355,#21356,#21357));
#5257=EDGE_LOOP('',(#21358));
#5258=EDGE_LOOP('',(#21359,#21360,#21361,#21362,#21363));
#5259=EDGE_LOOP('',(#21364,#21365,#21366,#21367,#21368));
#5260=EDGE_LOOP('',(#21369,#21370,#21371,#21372));
#5261=EDGE_LOOP('',(#21373));
#5262=EDGE_LOOP('',(#21374));
#5263=EDGE_LOOP('',(#21375,#21376,#21377,#21378));
#5264=EDGE_LOOP('',(#21379,#21380,#21381,#21382));
#5265=EDGE_LOOP('',(#21383,#21384,#21385,#21386));
#5266=EDGE_LOOP('',(#21387,#21388,#21389,#21390));
#5267=EDGE_LOOP('',(#21391,#21392,#21393,#21394));
#5268=EDGE_LOOP('',(#21395,#21396,#21397,#21398));
#5269=EDGE_LOOP('',(#21399,#21400,#21401,#21402));
#5270=EDGE_LOOP('',(#21403,#21404,#21405,#21406));
#5271=EDGE_LOOP('',(#21407,#21408,#21409,#21410));
#5272=EDGE_LOOP('',(#21411,#21412,#21413,#21414));
#5273=EDGE_LOOP('',(#21415,#21416,#21417,#21418));
#5274=EDGE_LOOP('',(#21419,#21420,#21421,#21422));
#5275=EDGE_LOOP('',(#21423,#21424,#21425,#21426,#21427,#21428,#21429,#21430));
#5276=EDGE_LOOP('',(#21431,#21432,#21433,#21434));
#5277=EDGE_LOOP('',(#21435,#21436,#21437,#21438));
#5278=EDGE_LOOP('',(#21439,#21440,#21441,#21442));
#5279=EDGE_LOOP('',(#21443,#21444,#21445,#21446));
#5280=EDGE_LOOP('',(#21447,#21448,#21449,#21450));
#5281=EDGE_LOOP('',(#21451,#21452,#21453,#21454));
#5282=EDGE_LOOP('',(#21455,#21456,#21457,#21458));
#5283=EDGE_LOOP('',(#21459,#21460,#21461,#21462));
#5284=EDGE_LOOP('',(#21463,#21464,#21465,#21466));
#5285=EDGE_LOOP('',(#21467,#21468,#21469,#21470,#21471));
#5286=EDGE_LOOP('',(#21472,#21473,#21474,#21475));
#5287=EDGE_LOOP('',(#21476,#21477,#21478,#21479));
#5288=EDGE_LOOP('',(#21480,#21481,#21482,#21483));
#5289=EDGE_LOOP('',(#21484,#21485,#21486,#21487));
#5290=EDGE_LOOP('',(#21488,#21489,#21490,#21491));
#5291=EDGE_LOOP('',(#21492,#21493,#21494,#21495));
#5292=EDGE_LOOP('',(#21496,#21497,#21498));
#5293=EDGE_LOOP('',(#21499,#21500,#21501,#21502));
#5294=EDGE_LOOP('',(#21503,#21504,#21505,#21506));
#5295=EDGE_LOOP('',(#21507,#21508,#21509));
#5296=EDGE_LOOP('',(#21510,#21511,#21512,#21513));
#5297=EDGE_LOOP('',(#21514,#21515,#21516,#21517));
#5298=EDGE_LOOP('',(#21518,#21519,#21520));
#5299=EDGE_LOOP('',(#21521,#21522,#21523,#21524));
#5300=EDGE_LOOP('',(#21525,#21526,#21527,#21528));
#5301=EDGE_LOOP('',(#21529,#21530,#21531));
#5302=EDGE_LOOP('',(#21532,#21533,#21534,#21535));
#5303=EDGE_LOOP('',(#21536,#21537,#21538,#21539));
#5304=EDGE_LOOP('',(#21540,#21541,#21542));
#5305=EDGE_LOOP('',(#21543,#21544,#21545,#21546));
#5306=EDGE_LOOP('',(#21547,#21548,#21549,#21550));
#5307=EDGE_LOOP('',(#21551,#21552,#21553,#21554));
#5308=EDGE_LOOP('',(#21555,#21556,#21557,#21558));
#5309=EDGE_LOOP('',(#21559,#21560,#21561,#21562));
#5310=EDGE_LOOP('',(#21563,#21564,#21565));
#5311=EDGE_LOOP('',(#21566,#21567,#21568,#21569));
#5312=EDGE_LOOP('',(#21570,#21571,#21572,#21573));
#5313=EDGE_LOOP('',(#21574,#21575,#21576));
#5314=EDGE_LOOP('',(#21577,#21578,#21579,#21580));
#5315=EDGE_LOOP('',(#21581,#21582,#21583,#21584));
#5316=EDGE_LOOP('',(#21585,#21586,#21587));
#5317=EDGE_LOOP('',(#21588,#21589,#21590,#21591));
#5318=EDGE_LOOP('',(#21592,#21593,#21594,#21595));
#5319=EDGE_LOOP('',(#21596,#21597,#21598));
#5320=EDGE_LOOP('',(#21599,#21600,#21601,#21602));
#5321=EDGE_LOOP('',(#21603,#21604,#21605,#21606));
#5322=EDGE_LOOP('',(#21607,#21608,#21609));
#5323=EDGE_LOOP('',(#21610,#21611,#21612,#21613));
#5324=EDGE_LOOP('',(#21614,#21615,#21616,#21617));
#5325=EDGE_LOOP('',(#21618,#21619,#21620));
#5326=EDGE_LOOP('',(#21621,#21622,#21623,#21624));
#5327=EDGE_LOOP('',(#21625,#21626,#21627,#21628));
#5328=EDGE_LOOP('',(#21629,#21630,#21631));
#5329=EDGE_LOOP('',(#21632,#21633,#21634,#21635));
#5330=EDGE_LOOP('',(#21636,#21637,#21638,#21639));
#5331=EDGE_LOOP('',(#21640,#21641,#21642));
#5332=EDGE_LOOP('',(#21643,#21644,#21645,#21646));
#5333=EDGE_LOOP('',(#21647,#21648,#21649,#21650));
#5334=EDGE_LOOP('',(#21651,#21652,#21653));
#5335=EDGE_LOOP('',(#21654,#21655,#21656,#21657));
#5336=EDGE_LOOP('',(#21658,#21659,#21660,#21661));
#5337=EDGE_LOOP('',(#21662,#21663,#21664));
#5338=EDGE_LOOP('',(#21665,#21666,#21667,#21668));
#5339=EDGE_LOOP('',(#21669,#21670,#21671,#21672));
#5340=EDGE_LOOP('',(#21673,#21674,#21675));
#5341=EDGE_LOOP('',(#21676,#21677,#21678,#21679));
#5342=EDGE_LOOP('',(#21680,#21681,#21682,#21683));
#5343=EDGE_LOOP('',(#21684,#21685,#21686));
#5344=EDGE_LOOP('',(#21687,#21688,#21689,#21690));
#5345=EDGE_LOOP('',(#21691,#21692,#21693,#21694));
#5346=EDGE_LOOP('',(#21695,#21696,#21697));
#5347=EDGE_LOOP('',(#21698,#21699,#21700,#21701));
#5348=EDGE_LOOP('',(#21702,#21703,#21704,#21705));
#5349=EDGE_LOOP('',(#21706,#21707,#21708));
#5350=EDGE_LOOP('',(#21709,#21710,#21711,#21712));
#5351=EDGE_LOOP('',(#21713,#21714,#21715,#21716));
#5352=EDGE_LOOP('',(#21717,#21718,#21719));
#5353=EDGE_LOOP('',(#21720,#21721,#21722,#21723));
#5354=EDGE_LOOP('',(#21724,#21725,#21726,#21727));
#5355=EDGE_LOOP('',(#21728,#21729,#21730));
#5356=EDGE_LOOP('',(#21731,#21732,#21733,#21734));
#5357=EDGE_LOOP('',(#21735,#21736,#21737,#21738));
#5358=EDGE_LOOP('',(#21739,#21740,#21741));
#5359=EDGE_LOOP('',(#21742,#21743,#21744,#21745));
#5360=EDGE_LOOP('',(#21746,#21747,#21748,#21749));
#5361=EDGE_LOOP('',(#21750,#21751,#21752));
#5362=EDGE_LOOP('',(#21753,#21754,#21755,#21756,#21757,#21758,#21759,#21760,
#21761,#21762,#21763,#21764,#21765,#21766,#21767,#21768,#21769,#21770,#21771,
#21772,#21773,#21774,#21775,#21776,#21777,#21778,#21779,#21780,#21781,#21782,
#21783,#21784,#21785,#21786,#21787,#21788,#21789,#21790,#21791,#21792,#21793,
#21794,#21795,#21796,#21797,#21798,#21799,#21800,#21801,#21802,#21803,#21804,
#21805,#21806,#21807,#21808,#21809,#21810,#21811,#21812,#21813,#21814,#21815,
#21816,#21817,#21818,#21819,#21820,#21821,#21822,#21823,#21824,#21825,#21826,
#21827));
#5363=EDGE_LOOP('',(#21828,#21829,#21830,#21831));
#5364=EDGE_LOOP('',(#21832,#21833,#21834,#21835));
#5365=EDGE_LOOP('',(#21836,#21837,#21838,#21839));
#5366=EDGE_LOOP('',(#21840,#21841,#21842,#21843));
#5367=EDGE_LOOP('',(#21844,#21845,#21846,#21847));
#5368=EDGE_LOOP('',(#21848,#21849,#21850,#21851));
#5369=EDGE_LOOP('',(#21852,#21853,#21854,#21855));
#5370=EDGE_LOOP('',(#21856,#21857,#21858,#21859));
#5371=EDGE_LOOP('',(#21860,#21861,#21862,#21863));
#5372=EDGE_LOOP('',(#21864,#21865,#21866,#21867));
#5373=EDGE_LOOP('',(#21868,#21869,#21870,#21871));
#5374=EDGE_LOOP('',(#21872,#21873,#21874,#21875));
#5375=EDGE_LOOP('',(#21876,#21877,#21878,#21879));
#5376=EDGE_LOOP('',(#21880,#21881,#21882,#21883));
#5377=EDGE_LOOP('',(#21884,#21885,#21886,#21887));
#5378=EDGE_LOOP('',(#21888,#21889,#21890,#21891));
#5379=EDGE_LOOP('',(#21892,#21893,#21894,#21895));
#5380=EDGE_LOOP('',(#21896,#21897,#21898,#21899));
#5381=EDGE_LOOP('',(#21900,#21901,#21902,#21903));
#5382=EDGE_LOOP('',(#21904,#21905,#21906,#21907));
#5383=EDGE_LOOP('',(#21908,#21909,#21910,#21911));
#5384=EDGE_LOOP('',(#21912,#21913,#21914,#21915));
#5385=EDGE_LOOP('',(#21916,#21917,#21918,#21919));
#5386=EDGE_LOOP('',(#21920,#21921,#21922,#21923,#21924,#21925,#21926,#21927,
#21928,#21929,#21930,#21931,#21932));
#5387=EDGE_LOOP('',(#21933,#21934,#21935,#21936));
#5388=EDGE_LOOP('',(#21937,#21938,#21939,#21940,#21941,#21942,#21943,#21944,
#21945,#21946,#21947,#21948));
#5389=EDGE_LOOP('',(#21949,#21950,#21951));
#5390=EDGE_LOOP('',(#21952));
#5391=EDGE_LOOP('',(#21953,#21954,#21955,#21956));
#5392=EDGE_LOOP('',(#21957,#21958,#21959,#21960));
#5393=EDGE_LOOP('',(#21961,#21962,#21963,#21964));
#5394=EDGE_LOOP('',(#21965));
#5395=EDGE_LOOP('',(#21966,#21967,#21968,#21969));
#5396=EDGE_LOOP('',(#21970));
#5397=EDGE_LOOP('',(#21971,#21972,#21973,#21974,#21975));
#5398=EDGE_LOOP('',(#21976,#21977,#21978,#21979,#21980,#21981,#21982,#21983,
#21984,#21985,#21986,#21987,#21988,#21989,#21990,#21991,#21992,#21993,#21994,
#21995,#21996,#21997,#21998,#21999,#22000,#22001,#22002,#22003,#22004,#22005,
#22006,#22007,#22008,#22009,#22010,#22011,#22012,#22013,#22014,#22015,#22016,
#22017,#22018,#22019,#22020,#22021,#22022,#22023,#22024,#22025,#22026,#22027));
#5399=EDGE_LOOP('',(#22028,#22029,#22030,#22031));
#5400=EDGE_LOOP('',(#22032));
#5401=EDGE_LOOP('',(#22033,#22034,#22035,#22036));
#5402=EDGE_LOOP('',(#22037,#22038,#22039,#22040));
#5403=EDGE_LOOP('',(#22041,#22042,#22043,#22044));
#5404=EDGE_LOOP('',(#22045,#22046,#22047,#22048));
#5405=EDGE_LOOP('',(#22049,#22050,#22051,#22052));
#5406=EDGE_LOOP('',(#22053,#22054,#22055,#22056));
#5407=EDGE_LOOP('',(#22057,#22058,#22059,#22060));
#5408=EDGE_LOOP('',(#22061,#22062,#22063,#22064));
#5409=EDGE_LOOP('',(#22065,#22066,#22067,#22068));
#5410=EDGE_LOOP('',(#22069,#22070,#22071,#22072));
#5411=EDGE_LOOP('',(#22073,#22074,#22075,#22076));
#5412=EDGE_LOOP('',(#22077,#22078,#22079,#22080));
#5413=EDGE_LOOP('',(#22081,#22082,#22083,#22084));
#5414=EDGE_LOOP('',(#22085,#22086,#22087,#22088));
#5415=EDGE_LOOP('',(#22089,#22090,#22091,#22092));
#5416=EDGE_LOOP('',(#22093,#22094,#22095,#22096));
#5417=EDGE_LOOP('',(#22097,#22098,#22099,#22100));
#5418=EDGE_LOOP('',(#22101,#22102,#22103,#22104));
#5419=EDGE_LOOP('',(#22105,#22106,#22107,#22108));
#5420=EDGE_LOOP('',(#22109,#22110,#22111,#22112));
#5421=EDGE_LOOP('',(#22113,#22114,#22115,#22116));
#5422=EDGE_LOOP('',(#22117,#22118,#22119,#22120));
#5423=EDGE_LOOP('',(#22121,#22122,#22123,#22124));
#5424=EDGE_LOOP('',(#22125,#22126,#22127,#22128));
#5425=EDGE_LOOP('',(#22129,#22130,#22131,#22132));
#5426=EDGE_LOOP('',(#22133,#22134,#22135,#22136));
#5427=EDGE_LOOP('',(#22137,#22138,#22139,#22140));
#5428=EDGE_LOOP('',(#22141,#22142,#22143,#22144));
#5429=EDGE_LOOP('',(#22145,#22146,#22147,#22148));
#5430=EDGE_LOOP('',(#22149,#22150,#22151,#22152));
#5431=EDGE_LOOP('',(#22153,#22154,#22155,#22156));
#5432=EDGE_LOOP('',(#22157,#22158,#22159));
#5433=EDGE_LOOP('',(#22160,#22161,#22162,#22163));
#5434=EDGE_LOOP('',(#22164,#22165,#22166,#22167));
#5435=EDGE_LOOP('',(#22168,#22169,#22170));
#5436=EDGE_LOOP('',(#22171,#22172,#22173,#22174));
#5437=EDGE_LOOP('',(#22175,#22176,#22177,#22178));
#5438=EDGE_LOOP('',(#22179,#22180,#22181));
#5439=EDGE_LOOP('',(#22182,#22183,#22184,#22185));
#5440=EDGE_LOOP('',(#22186,#22187,#22188,#22189));
#5441=EDGE_LOOP('',(#22190,#22191,#22192));
#5442=EDGE_LOOP('',(#22193,#22194,#22195,#22196));
#5443=EDGE_LOOP('',(#22197,#22198,#22199,#22200));
#5444=EDGE_LOOP('',(#22201,#22202,#22203));
#5445=EDGE_LOOP('',(#22204,#22205,#22206,#22207));
#5446=EDGE_LOOP('',(#22208,#22209,#22210,#22211));
#5447=EDGE_LOOP('',(#22212,#22213,#22214));
#5448=EDGE_LOOP('',(#22215,#22216,#22217,#22218));
#5449=EDGE_LOOP('',(#22219,#22220,#22221,#22222));
#5450=EDGE_LOOP('',(#22223,#22224,#22225));
#5451=EDGE_LOOP('',(#22226,#22227,#22228,#22229));
#5452=EDGE_LOOP('',(#22230,#22231,#22232,#22233));
#5453=EDGE_LOOP('',(#22234,#22235,#22236));
#5454=EDGE_LOOP('',(#22237,#22238,#22239,#22240));
#5455=EDGE_LOOP('',(#22241,#22242,#22243,#22244));
#5456=EDGE_LOOP('',(#22245,#22246,#22247));
#5457=EDGE_LOOP('',(#22248,#22249,#22250,#22251));
#5458=EDGE_LOOP('',(#22252,#22253,#22254,#22255));
#5459=EDGE_LOOP('',(#22256,#22257,#22258));
#5460=EDGE_LOOP('',(#22259,#22260,#22261,#22262));
#5461=EDGE_LOOP('',(#22263,#22264,#22265,#22266));
#5462=EDGE_LOOP('',(#22267,#22268,#22269));
#5463=EDGE_LOOP('',(#22270,#22271,#22272,#22273));
#5464=EDGE_LOOP('',(#22274,#22275,#22276,#22277));
#5465=EDGE_LOOP('',(#22278,#22279,#22280));
#5466=EDGE_LOOP('',(#22281,#22282,#22283,#22284));
#5467=EDGE_LOOP('',(#22285,#22286,#22287,#22288));
#5468=EDGE_LOOP('',(#22289,#22290,#22291));
#5469=EDGE_LOOP('',(#22292,#22293,#22294,#22295));
#5470=EDGE_LOOP('',(#22296,#22297,#22298,#22299));
#5471=EDGE_LOOP('',(#22300,#22301,#22302,#22303));
#5472=EDGE_LOOP('',(#22304,#22305,#22306,#22307));
#5473=EDGE_LOOP('',(#22308,#22309,#22310,#22311));
#5474=EDGE_LOOP('',(#22312,#22313,#22314));
#5475=EDGE_LOOP('',(#22315,#22316,#22317,#22318));
#5476=EDGE_LOOP('',(#22319,#22320,#22321,#22322));
#5477=EDGE_LOOP('',(#22323,#22324,#22325));
#5478=EDGE_LOOP('',(#22326,#22327,#22328,#22329));
#5479=EDGE_LOOP('',(#22330,#22331,#22332,#22333));
#5480=EDGE_LOOP('',(#22334,#22335,#22336));
#5481=EDGE_LOOP('',(#22337,#22338,#22339,#22340));
#5482=EDGE_LOOP('',(#22341,#22342,#22343,#22344));
#5483=EDGE_LOOP('',(#22345,#22346,#22347));
#5484=EDGE_LOOP('',(#22348,#22349,#22350,#22351));
#5485=EDGE_LOOP('',(#22352,#22353,#22354,#22355,#22356,#22357,#22358,#22359,
#22360,#22361,#22362,#22363,#22364,#22365,#22366,#22367,#22368,#22369,#22370,
#22371,#22372,#22373,#22374,#22375,#22376,#22377,#22378,#22379,#22380,#22381,
#22382,#22383,#22384,#22385,#22386,#22387,#22388,#22389,#22390,#22391,#22392,
#22393,#22394,#22395,#22396,#22397,#22398,#22399,#22400,#22401,#22402,#22403,
#22404,#22405,#22406,#22407,#22408,#22409,#22410,#22411,#22412,#22413,#22414,
#22415,#22416,#22417,#22418,#22419,#22420,#22421,#22422,#22423,#22424,#22425,
#22426,#22427));
#5486=EDGE_LOOP('',(#22428,#22429,#22430,#22431,#22432,#22433,#22434,#22435,
#22436,#22437,#22438,#22439,#22440,#22441,#22442,#22443,#22444,#22445,#22446,
#22447,#22448,#22449,#22450,#22451,#22452,#22453,#22454,#22455,#22456,#22457,
#22458,#22459,#22460,#22461));
#5487=EDGE_LOOP('',(#22462,#22463,#22464,#22465,#22466));
#5488=EDGE_LOOP('',(#22467,#22468,#22469,#22470));
#5489=EDGE_LOOP('',(#22471,#22472,#22473,#22474,#22475,#22476,#22477,#22478,
#22479,#22480,#22481,#22482,#22483,#22484,#22485,#22486,#22487,#22488,#22489,
#22490,#22491,#22492,#22493,#22494,#22495,#22496,#22497,#22498,#22499,#22500,
#22501,#22502,#22503,#22504));
#5490=EDGE_LOOP('',(#22505));
#5491=EDGE_LOOP('',(#22506,#22507,#22508,#22509,#22510,#22511));
#5492=EDGE_LOOP('',(#22512,#22513,#22514,#22515));
#5493=EDGE_LOOP('',(#22516));
#5494=EDGE_LOOP('',(#22517,#22518,#22519,#22520));
#5495=EDGE_LOOP('',(#22521,#22522,#22523,#22524));
#5496=EDGE_LOOP('',(#22525,#22526,#22527,#22528,#22529,#22530,#22531,#22532,
#22533,#22534,#22535,#22536,#22537,#22538,#22539,#22540,#22541,#22542,#22543,
#22544,#22545,#22546,#22547,#22548,#22549,#22550,#22551,#22552,#22553,#22554,
#22555,#22556,#22557,#22558,#22559,#22560,#22561,#22562,#22563,#22564,#22565,
#22566,#22567,#22568,#22569,#22570,#22571,#22572,#22573,#22574,#22575,#22576,
#22577,#22578,#22579,#22580,#22581));
#5497=EDGE_LOOP('',(#22582));
#5498=EDGE_LOOP('',(#22583,#22584,#22585,#22586));
#5499=EDGE_LOOP('',(#22587));
#5500=EDGE_LOOP('',(#22588,#22589,#22590,#22591,#22592,#22593));
#5501=EDGE_LOOP('',(#22594));
#5502=EDGE_LOOP('',(#22595,#22596,#22597,#22598));
#5503=EDGE_LOOP('',(#22599,#22600,#22601,#22602));
#5504=EDGE_LOOP('',(#22603,#22604,#22605,#22606));
#5505=EDGE_LOOP('',(#22607,#22608,#22609,#22610));
#5506=EDGE_LOOP('',(#22611,#22612,#22613,#22614));
#5507=EDGE_LOOP('',(#22615,#22616,#22617,#22618));
#5508=EDGE_LOOP('',(#22619,#22620,#22621,#22622,#22623,#22624));
#5509=EDGE_LOOP('',(#22625));
#5510=EDGE_LOOP('',(#22626,#22627));
#5511=EDGE_LOOP('',(#22628,#22629,#22630));
#5512=EDGE_LOOP('',(#22631,#22632,#22633,#22634,#22635,#22636,#22637,#22638));
#5513=EDGE_LOOP('',(#22639,#22640,#22641,#22642));
#5514=EDGE_LOOP('',(#22643,#22644,#22645,#22646));
#5515=EDGE_LOOP('',(#22647,#22648,#22649,#22650));
#5516=EDGE_LOOP('',(#22651,#22652,#22653,#22654));
#5517=EDGE_LOOP('',(#22655,#22656,#22657,#22658));
#5518=EDGE_LOOP('',(#22659,#22660,#22661,#22662));
#5519=EDGE_LOOP('',(#22663,#22664,#22665,#22666));
#5520=EDGE_LOOP('',(#22667,#22668,#22669,#22670,#22671,#22672,#22673));
#5521=EDGE_LOOP('',(#22674,#22675,#22676,#22677));
#5522=EDGE_LOOP('',(#22678,#22679,#22680,#22681));
#5523=EDGE_LOOP('',(#22682,#22683,#22684,#22685));
#5524=EDGE_LOOP('',(#22686,#22687,#22688,#22689));
#5525=EDGE_LOOP('',(#22690,#22691,#22692,#22693));
#5526=EDGE_LOOP('',(#22694,#22695,#22696,#22697));
#5527=EDGE_LOOP('',(#22698,#22699,#22700,#22701));
#5528=EDGE_LOOP('',(#22702,#22703,#22704,#22705));
#5529=EDGE_LOOP('',(#22706,#22707,#22708,#22709));
#5530=EDGE_LOOP('',(#22710,#22711,#22712,#22713));
#5531=EDGE_LOOP('',(#22714,#22715,#22716,#22717));
#5532=EDGE_LOOP('',(#22718,#22719,#22720,#22721));
#5533=EDGE_LOOP('',(#22722,#22723,#22724,#22725));
#5534=EDGE_LOOP('',(#22726,#22727,#22728,#22729));
#5535=EDGE_LOOP('',(#22730,#22731,#22732,#22733));
#5536=EDGE_LOOP('',(#22734,#22735,#22736,#22737));
#5537=EDGE_LOOP('',(#22738,#22739,#22740,#22741));
#5538=EDGE_LOOP('',(#22742,#22743,#22744,#22745));
#5539=EDGE_LOOP('',(#22746,#22747,#22748,#22749));
#5540=EDGE_LOOP('',(#22750,#22751,#22752,#22753));
#5541=EDGE_LOOP('',(#22754,#22755,#22756,#22757));
#5542=EDGE_LOOP('',(#22758,#22759,#22760,#22761));
#5543=EDGE_LOOP('',(#22762,#22763,#22764,#22765));
#5544=EDGE_LOOP('',(#22766,#22767,#22768,#22769));
#5545=EDGE_LOOP('',(#22770,#22771,#22772,#22773));
#5546=EDGE_LOOP('',(#22774,#22775,#22776,#22777));
#5547=EDGE_LOOP('',(#22778,#22779,#22780,#22781));
#5548=EDGE_LOOP('',(#22782,#22783,#22784,#22785));
#5549=EDGE_LOOP('',(#22786,#22787,#22788,#22789));
#5550=EDGE_LOOP('',(#22790,#22791,#22792,#22793));
#5551=EDGE_LOOP('',(#22794,#22795,#22796,#22797));
#5552=EDGE_LOOP('',(#22798,#22799,#22800,#22801));
#5553=EDGE_LOOP('',(#22802,#22803,#22804,#22805));
#5554=EDGE_LOOP('',(#22806,#22807,#22808,#22809));
#5555=EDGE_LOOP('',(#22810,#22811,#22812,#22813));
#5556=EDGE_LOOP('',(#22814,#22815,#22816,#22817));
#5557=EDGE_LOOP('',(#22818,#22819,#22820,#22821));
#5558=EDGE_LOOP('',(#22822,#22823,#22824,#22825));
#5559=EDGE_LOOP('',(#22826,#22827,#22828,#22829));
#5560=EDGE_LOOP('',(#22830,#22831,#22832,#22833));
#5561=EDGE_LOOP('',(#22834,#22835,#22836,#22837));
#5562=EDGE_LOOP('',(#22838,#22839,#22840,#22841));
#5563=EDGE_LOOP('',(#22842,#22843,#22844,#22845));
#5564=EDGE_LOOP('',(#22846,#22847,#22848,#22849));
#5565=EDGE_LOOP('',(#22850,#22851,#22852,#22853));
#5566=EDGE_LOOP('',(#22854,#22855,#22856,#22857));
#5567=EDGE_LOOP('',(#22858,#22859,#22860,#22861));
#5568=EDGE_LOOP('',(#22862,#22863,#22864,#22865));
#5569=EDGE_LOOP('',(#22866,#22867,#22868,#22869));
#5570=EDGE_LOOP('',(#22870,#22871,#22872,#22873));
#5571=EDGE_LOOP('',(#22874,#22875,#22876,#22877));
#5572=EDGE_LOOP('',(#22878,#22879,#22880,#22881));
#5573=EDGE_LOOP('',(#22882,#22883,#22884,#22885));
#5574=EDGE_LOOP('',(#22886,#22887,#22888,#22889));
#5575=EDGE_LOOP('',(#22890,#22891,#22892,#22893));
#5576=EDGE_LOOP('',(#22894));
#5577=EDGE_LOOP('',(#22895,#22896,#22897,#22898));
#5578=EDGE_LOOP('',(#22899,#22900,#22901,#22902));
#5579=EDGE_LOOP('',(#22903,#22904,#22905,#22906));
#5580=EDGE_LOOP('',(#22907,#22908,#22909,#22910));
#5581=EDGE_LOOP('',(#22911,#22912,#22913,#22914));
#5582=EDGE_LOOP('',(#22915,#22916,#22917,#22918));
#5583=EDGE_LOOP('',(#22919,#22920,#22921,#22922));
#5584=EDGE_LOOP('',(#22923,#22924,#22925,#22926));
#5585=EDGE_LOOP('',(#22927,#22928,#22929,#22930));
#5586=EDGE_LOOP('',(#22931,#22932,#22933,#22934));
#5587=EDGE_LOOP('',(#22935,#22936,#22937,#22938));
#5588=EDGE_LOOP('',(#22939,#22940,#22941,#22942,#22943,#22944,#22945));
#5589=EDGE_LOOP('',(#22946,#22947,#22948,#22949));
#5590=EDGE_LOOP('',(#22950));
#5591=EDGE_LOOP('',(#22951,#22952,#22953,#22954));
#5592=EDGE_LOOP('',(#22955,#22956,#22957,#22958));
#5593=EDGE_LOOP('',(#22959,#22960,#22961,#22962));
#5594=EDGE_LOOP('',(#22963));
#5595=EDGE_LOOP('',(#22964));
#5596=EDGE_LOOP('',(#22965,#22966,#22967,#22968));
#5597=EDGE_LOOP('',(#22969,#22970,#22971,#22972));
#5598=EDGE_LOOP('',(#22973));
#5599=EDGE_LOOP('',(#22974));
#5600=EDGE_LOOP('',(#22975,#22976,#22977,#22978,#22979));
#5601=EDGE_LOOP('',(#22980,#22981,#22982,#22983,#22984,#22985));
#5602=EDGE_LOOP('',(#22986,#22987,#22988,#22989));
#5603=EDGE_LOOP('',(#22990));
#5604=EDGE_LOOP('',(#22991));
#5605=EDGE_LOOP('',(#22992,#22993,#22994,#22995,#22996));
#5606=EDGE_LOOP('',(#22997,#22998,#22999,#23000));
#5607=EDGE_LOOP('',(#23001,#23002,#23003));
#5608=EDGE_LOOP('',(#23004,#23005,#23006,#23007,#23008,#23009,#23010,#23011,
#23012));
#5609=EDGE_LOOP('',(#23013));
#5610=EDGE_LOOP('',(#23014,#23015,#23016,#23017));
#5611=EDGE_LOOP('',(#23018));
#5612=EDGE_LOOP('',(#23019));
#5613=EDGE_LOOP('',(#23020,#23021,#23022,#23023));
#5614=EDGE_LOOP('',(#23024,#23025,#23026,#23027));
#5615=EDGE_LOOP('',(#23028,#23029,#23030,#23031));
#5616=EDGE_LOOP('',(#23032));
#5617=EDGE_LOOP('',(#23033));
#5618=EDGE_LOOP('',(#23034,#23035,#23036,#23037));
#5619=EDGE_LOOP('',(#23038));
#5620=EDGE_LOOP('',(#23039,#23040,#23041,#23042));
#5621=EDGE_LOOP('',(#23043));
#5622=EDGE_LOOP('',(#23044));
#5623=EDGE_LOOP('',(#23045,#23046,#23047,#23048));
#5624=EDGE_LOOP('',(#23049,#23050,#23051,#23052));
#5625=EDGE_LOOP('',(#23053,#23054,#23055,#23056));
#5626=EDGE_LOOP('',(#23057,#23058,#23059,#23060));
#5627=EDGE_LOOP('',(#23061,#23062,#23063,#23064));
#5628=EDGE_LOOP('',(#23065,#23066,#23067,#23068));
#5629=EDGE_LOOP('',(#23069,#23070,#23071,#23072,#23073));
#5630=EDGE_LOOP('',(#23074,#23075,#23076,#23077,#23078,#23079,#23080,#23081));
#5631=EDGE_LOOP('',(#23082,#23083,#23084));
#5632=EDGE_LOOP('',(#23085,#23086,#23087,#23088,#23089));
#5633=EDGE_LOOP('',(#23090,#23091,#23092));
#5634=EDGE_LOOP('',(#23093,#23094,#23095,#23096,#23097,#23098,#23099));
#5635=EDGE_LOOP('',(#23100,#23101,#23102,#23103,#23104,#23105));
#5636=EDGE_LOOP('',(#23106,#23107,#23108,#23109,#23110,#23111));
#5637=EDGE_LOOP('',(#23112,#23113,#23114,#23115,#23116,#23117));
#5638=EDGE_LOOP('',(#23118,#23119,#23120,#23121,#23122));
#5639=EDGE_LOOP('',(#23123,#23124,#23125,#23126,#23127,#23128));
#5640=EDGE_LOOP('',(#23129,#23130,#23131,#23132,#23133));
#5641=EDGE_LOOP('',(#23134,#23135,#23136,#23137,#23138));
#5642=EDGE_LOOP('',(#23139,#23140,#23141,#23142,#23143));
#5643=EDGE_LOOP('',(#23144,#23145,#23146,#23147,#23148,#23149,#23150,#23151));
#5644=EDGE_LOOP('',(#23152,#23153,#23154,#23155));
#5645=EDGE_LOOP('',(#23156,#23157,#23158,#23159,#23160,#23161,#23162));
#5646=EDGE_LOOP('',(#23163,#23164,#23165,#23166,#23167,#23168));
#5647=EDGE_LOOP('',(#23169,#23170,#23171,#23172,#23173));
#5648=EDGE_LOOP('',(#23174,#23175,#23176,#23177,#23178,#23179,#23180));
#5649=EDGE_LOOP('',(#23181,#23182,#23183));
#5650=EDGE_LOOP('',(#23184,#23185,#23186));
#5651=EDGE_LOOP('',(#23187,#23188,#23189,#23190,#23191,#23192));
#5652=EDGE_LOOP('',(#23193,#23194,#23195,#23196,#23197,#23198));
#5653=EDGE_LOOP('',(#23199,#23200,#23201,#23202,#23203));
#5654=EDGE_LOOP('',(#23204,#23205,#23206,#23207,#23208,#23209));
#5655=EDGE_LOOP('',(#23210,#23211,#23212,#23213,#23214,#23215));
#5656=EDGE_LOOP('',(#23216,#23217,#23218,#23219,#23220));
#5657=EDGE_LOOP('',(#23221,#23222,#23223,#23224));
#5658=EDGE_LOOP('',(#23225,#23226,#23227,#23228));
#5659=EDGE_LOOP('',(#23229,#23230,#23231,#23232));
#5660=EDGE_LOOP('',(#23233,#23234,#23235,#23236));
#5661=EDGE_LOOP('',(#23237,#23238,#23239,#23240));
#5662=EDGE_LOOP('',(#23241,#23242,#23243,#23244));
#5663=EDGE_LOOP('',(#23245,#23246,#23247,#23248));
#5664=EDGE_LOOP('',(#23249,#23250,#23251,#23252));
#5665=EDGE_LOOP('',(#23253,#23254,#23255,#23256));
#5666=EDGE_LOOP('',(#23257,#23258,#23259,#23260));
#5667=EDGE_LOOP('',(#23261,#23262,#23263,#23264));
#5668=EDGE_LOOP('',(#23265,#23266,#23267,#23268));
#5669=EDGE_LOOP('',(#23269,#23270,#23271,#23272,#23273,#23274,#23275,#23276));
#5670=EDGE_LOOP('',(#23277));
#5671=EDGE_LOOP('',(#23278));
#5672=EDGE_LOOP('',(#23279,#23280,#23281,#23282));
#5673=EDGE_LOOP('',(#23283,#23284,#23285,#23286));
#5674=EDGE_LOOP('',(#23287,#23288,#23289,#23290,#23291));
#5675=EDGE_LOOP('',(#23292,#23293,#23294,#23295,#23296));
#5676=EDGE_LOOP('',(#23297,#23298,#23299,#23300,#23301,#23302,#23303,#23304,
#23305,#23306,#23307,#23308,#23309,#23310,#23311,#23312));
#5677=EDGE_LOOP('',(#23313));
#5678=EDGE_LOOP('',(#23314));
#5679=EDGE_LOOP('',(#23315,#23316,#23317,#23318,#23319));
#5680=EDGE_LOOP('',(#23320,#23321,#23322,#23323,#23324));
#5681=EDGE_LOOP('',(#23325,#23326,#23327,#23328,#23329));
#5682=EDGE_LOOP('',(#23330,#23331,#23332,#23333,#23334));
#5683=EDGE_LOOP('',(#23335,#23336,#23337,#23338,#23339,#23340,#23341,#23342,
#23343,#23344,#23345,#23346,#23347,#23348,#23349,#23350));
#5684=EDGE_LOOP('',(#23351));
#5685=EDGE_LOOP('',(#23352));
#5686=EDGE_LOOP('',(#23353,#23354,#23355,#23356));
#5687=EDGE_LOOP('',(#23357,#23358,#23359,#23360,#23361));
#5688=EDGE_LOOP('',(#23362,#23363,#23364,#23365));
#5689=EDGE_LOOP('',(#23366,#23367,#23368,#23369));
#5690=EDGE_LOOP('',(#23370,#23371,#23372,#23373));
#5691=EDGE_LOOP('',(#23374,#23375,#23376,#23377));
#5692=EDGE_LOOP('',(#23378));
#5693=EDGE_LOOP('',(#23379));
#5694=EDGE_LOOP('',(#23380,#23381,#23382,#23383));
#5695=EDGE_LOOP('',(#23384,#23385,#23386,#23387));
#5696=EDGE_LOOP('',(#23388,#23389,#23390,#23391));
#5697=EDGE_LOOP('',(#23392,#23393,#23394,#23395));
#5698=EDGE_LOOP('',(#23396,#23397,#23398,#23399));
#5699=EDGE_LOOP('',(#23400));
#5700=EDGE_LOOP('',(#23401));
#5701=EDGE_LOOP('',(#23402,#23403,#23404,#23405));
#5702=EDGE_LOOP('',(#23406,#23407,#23408,#23409));
#5703=EDGE_LOOP('',(#23410,#23411,#23412,#23413));
#5704=EDGE_LOOP('',(#23414,#23415,#23416,#23417));
#5705=EDGE_LOOP('',(#23418,#23419,#23420,#23421));
#5706=EDGE_LOOP('',(#23422,#23423,#23424,#23425));
#5707=EDGE_LOOP('',(#23426,#23427,#23428,#23429));
#5708=EDGE_LOOP('',(#23430,#23431,#23432,#23433));
#5709=EDGE_LOOP('',(#23434,#23435,#23436,#23437));
#5710=EDGE_LOOP('',(#23438,#23439,#23440,#23441));
#5711=EDGE_LOOP('',(#23442,#23443,#23444,#23445));
#5712=EDGE_LOOP('',(#23446,#23447,#23448,#23449));
#5713=EDGE_LOOP('',(#23450,#23451,#23452,#23453));
#5714=EDGE_LOOP('',(#23454,#23455,#23456,#23457));
#5715=EDGE_LOOP('',(#23458,#23459,#23460,#23461));
#5716=EDGE_LOOP('',(#23462,#23463,#23464,#23465,#23466,#23467,#23468,#23469,
#23470,#23471,#23472,#23473,#23474,#23475,#23476,#23477,#23478,#23479,#23480,
#23481));
#5717=EDGE_LOOP('',(#23482));
#5718=EDGE_LOOP('',(#23483,#23484,#23485,#23486,#23487,#23488,#23489,#23490));
#5719=EDGE_LOOP('',(#23491,#23492,#23493,#23494,#23495,#23496,#23497,#23498));
#5720=EDGE_LOOP('',(#23499));
#5721=EDGE_LOOP('',(#23500,#23501,#23502,#23503));
#5722=EDGE_LOOP('',(#23504,#23505,#23506,#23507));
#5723=EDGE_LOOP('',(#23508,#23509,#23510,#23511));
#5724=EDGE_LOOP('',(#23512,#23513,#23514,#23515));
#5725=EDGE_LOOP('',(#23516,#23517,#23518,#23519));
#5726=EDGE_LOOP('',(#23520,#23521,#23522,#23523));
#5727=EDGE_LOOP('',(#23524,#23525,#23526,#23527));
#5728=EDGE_LOOP('',(#23528,#23529,#23530,#23531));
#5729=EDGE_LOOP('',(#23532,#23533,#23534,#23535,#23536,#23537));
#5730=EDGE_LOOP('',(#23538,#23539,#23540,#23541,#23542,#23543,#23544));
#5731=EDGE_LOOP('',(#23545,#23546,#23547,#23548));
#5732=EDGE_LOOP('',(#23549,#23550,#23551,#23552));
#5733=EDGE_LOOP('',(#23553,#23554,#23555,#23556));
#5734=EDGE_LOOP('',(#23557,#23558,#23559,#23560,#23561,#23562,#23563,#23564));
#5735=EDGE_LOOP('',(#23565,#23566,#23567,#23568));
#5736=EDGE_LOOP('',(#23569,#23570,#23571,#23572));
#5737=EDGE_LOOP('',(#23573,#23574,#23575,#23576));
#5738=EDGE_LOOP('',(#23577,#23578,#23579,#23580,#23581,#23582,#23583,#23584));
#5739=EDGE_LOOP('',(#23585,#23586,#23587,#23588));
#5740=EDGE_LOOP('',(#23589,#23590,#23591,#23592));
#5741=EDGE_LOOP('',(#23593,#23594,#23595,#23596));
#5742=EDGE_LOOP('',(#23597,#23598,#23599,#23600));
#5743=EDGE_LOOP('',(#23601,#23602,#23603,#23604));
#5744=EDGE_LOOP('',(#23605,#23606,#23607));
#5745=EDGE_LOOP('',(#23608));
#5746=EDGE_LOOP('',(#23609,#23610,#23611,#23612,#23613,#23614));
#5747=EDGE_LOOP('',(#23615,#23616));
#5748=EDGE_LOOP('',(#23617,#23618,#23619,#23620,#23621,#23622));
#5749=EDGE_LOOP('',(#23623,#23624));
#5750=EDGE_LOOP('',(#23625,#23626));
#5751=EDGE_LOOP('',(#23627,#23628,#23629,#23630));
#5752=EDGE_LOOP('',(#23631,#23632,#23633,#23634,#23635,#23636,#23637));
#5753=EDGE_LOOP('',(#23638));
#5754=EDGE_LOOP('',(#23639,#23640,#23641));
#5755=EDGE_LOOP('',(#23642,#23643,#23644));
#5756=EDGE_LOOP('',(#23645,#23646,#23647,#23648,#23649));
#5757=EDGE_LOOP('',(#23650,#23651,#23652,#23653,#23654,#23655,#23656,#23657,
#23658));
#5758=EDGE_LOOP('',(#23659));
#5759=EDGE_LOOP('',(#23660));
#5760=EDGE_LOOP('',(#23661,#23662,#23663,#23664));
#5761=EDGE_LOOP('',(#23665,#23666,#23667,#23668));
#5762=EDGE_LOOP('',(#23669,#23670,#23671,#23672));
#5763=EDGE_LOOP('',(#23673,#23674,#23675,#23676));
#5764=EDGE_LOOP('',(#23677,#23678,#23679,#23680));
#5765=EDGE_LOOP('',(#23681,#23682,#23683,#23684));
#5766=EDGE_LOOP('',(#23685,#23686,#23687,#23688));
#5767=EDGE_LOOP('',(#23689,#23690,#23691,#23692));
#5768=EDGE_LOOP('',(#23693,#23694,#23695,#23696));
#5769=EDGE_LOOP('',(#23697,#23698,#23699,#23700));
#5770=EDGE_LOOP('',(#23701,#23702,#23703,#23704));
#5771=EDGE_LOOP('',(#23705,#23706,#23707,#23708));
#5772=EDGE_LOOP('',(#23709,#23710,#23711,#23712));
#5773=EDGE_LOOP('',(#23713,#23714,#23715,#23716));
#5774=EDGE_LOOP('',(#23717,#23718,#23719,#23720));
#5775=EDGE_LOOP('',(#23721,#23722,#23723,#23724));
#5776=EDGE_LOOP('',(#23725,#23726,#23727,#23728));
#5777=EDGE_LOOP('',(#23729,#23730,#23731,#23732));
#5778=EDGE_LOOP('',(#23733,#23734,#23735,#23736));
#5779=EDGE_LOOP('',(#23737,#23738,#23739,#23740));
#5780=EDGE_LOOP('',(#23741,#23742,#23743,#23744));
#5781=EDGE_LOOP('',(#23745,#23746,#23747,#23748));
#5782=EDGE_LOOP('',(#23749,#23750,#23751,#23752,#23753,#23754,#23755,#23756,
#23757,#23758,#23759,#23760,#23761,#23762,#23763,#23764));
#5783=EDGE_LOOP('',(#23765));
#5784=EDGE_LOOP('',(#23766,#23767,#23768,#23769));
#5785=EDGE_LOOP('',(#23770,#23771,#23772));
#5786=EDGE_LOOP('',(#23773,#23774,#23775,#23776));
#5787=EDGE_LOOP('',(#23777,#23778,#23779,#23780));
#5788=EDGE_LOOP('',(#23781,#23782,#23783));
#5789=EDGE_LOOP('',(#23784));
#5790=EDGE_LOOP('',(#23785,#23786,#23787,#23788));
#5791=EDGE_LOOP('',(#23789,#23790,#23791,#23792));
#5792=EDGE_LOOP('',(#23793,#23794,#23795,#23796));
#5793=EDGE_LOOP('',(#23797,#23798,#23799,#23800,#23801,#23802,#23803,#23804,
#23805,#23806,#23807,#23808,#23809,#23810,#23811,#23812,#23813,#23814,#23815,
#23816,#23817,#23818,#23819,#23820,#23821,#23822));
#5794=EDGE_LOOP('',(#23823,#23824,#23825,#23826));
#5795=EDGE_LOOP('',(#23827,#23828,#23829,#23830,#23831,#23832,#23833,#23834,
#23835,#23836,#23837,#23838,#23839,#23840,#23841,#23842,#23843,#23844,#23845,
#23846,#23847,#23848,#23849,#23850,#23851,#23852));
#5796=EDGE_LOOP('',(#23853,#23854,#23855,#23856,#23857));
#5797=EDGE_LOOP('',(#23858));
#5798=EDGE_LOOP('',(#23859,#23860,#23861,#23862,#23863,#23864));
#5799=EDGE_LOOP('',(#23865,#23866,#23867,#23868));
#5800=EDGE_LOOP('',(#23869,#23870,#23871,#23872,#23873,#23874));
#5801=EDGE_LOOP('',(#23875,#23876,#23877,#23878));
#5802=EDGE_LOOP('',(#23879,#23880,#23881,#23882,#23883,#23884));
#5803=EDGE_LOOP('',(#23885,#23886,#23887,#23888,#23889,#23890));
#5804=EDGE_LOOP('',(#23891,#23892,#23893,#23894,#23895,#23896,#23897,#23898,
#23899,#23900));
#5805=EDGE_LOOP('',(#23901,#23902,#23903,#23904));
#5806=EDGE_LOOP('',(#23905,#23906,#23907,#23908,#23909));
#5807=EDGE_LOOP('',(#23910,#23911,#23912,#23913,#23914,#23915));
#5808=EDGE_LOOP('',(#23916,#23917,#23918,#23919,#23920));
#5809=EDGE_LOOP('',(#23921,#23922,#23923,#23924,#23925,#23926));
#5810=EDGE_LOOP('',(#23927,#23928,#23929,#23930));
#5811=EDGE_LOOP('',(#23931,#23932,#23933,#23934,#23935,#23936));
#5812=EDGE_LOOP('',(#23937,#23938,#23939,#23940,#23941));
#5813=EDGE_LOOP('',(#23942,#23943,#23944,#23945));
#5814=EDGE_LOOP('',(#23946,#23947,#23948,#23949,#23950,#23951));
#5815=EDGE_LOOP('',(#23952,#23953,#23954,#23955,#23956,#23957));
#5816=EDGE_LOOP('',(#23958,#23959,#23960,#23961,#23962));
#5817=EDGE_LOOP('',(#23963,#23964,#23965));
#5818=EDGE_LOOP('',(#23966,#23967,#23968,#23969));
#5819=EDGE_LOOP('',(#23970,#23971,#23972,#23973,#23974));
#5820=EDGE_LOOP('',(#23975,#23976,#23977,#23978,#23979));
#5821=EDGE_LOOP('',(#23980,#23981,#23982,#23983));
#5822=EDGE_LOOP('',(#23984,#23985,#23986,#23987,#23988,#23989));
#5823=EDGE_LOOP('',(#23990,#23991,#23992,#23993,#23994,#23995));
#5824=EDGE_LOOP('',(#23996,#23997,#23998,#23999,#24000,#24001));
#5825=EDGE_LOOP('',(#24002,#24003,#24004,#24005,#24006));
#5826=EDGE_LOOP('',(#24007,#24008,#24009));
#5827=EDGE_LOOP('',(#24010,#24011,#24012,#24013,#24014));
#5828=EDGE_LOOP('',(#24015,#24016,#24017));
#5829=EDGE_LOOP('',(#24018,#24019,#24020,#24021));
#5830=EDGE_LOOP('',(#24022,#24023,#24024));
#5831=EDGE_LOOP('',(#24025,#24026,#24027,#24028));
#5832=EDGE_LOOP('',(#24029,#24030,#24031,#24032,#24033));
#5833=EDGE_LOOP('',(#24034,#24035,#24036));
#5834=EDGE_LOOP('',(#24037,#24038,#24039,#24040));
#5835=EDGE_LOOP('',(#24041,#24042,#24043,#24044));
#5836=EDGE_LOOP('',(#24045,#24046,#24047,#24048));
#5837=EDGE_LOOP('',(#24049,#24050,#24051,#24052));
#5838=EDGE_LOOP('',(#24053,#24054,#24055,#24056));
#5839=EDGE_LOOP('',(#24057,#24058,#24059,#24060,#24061,#24062,#24063,#24064,
#24065,#24066));
#5840=EDGE_LOOP('',(#24067,#24068,#24069,#24070));
#5841=EDGE_LOOP('',(#24071,#24072,#24073,#24074));
#5842=EDGE_LOOP('',(#24075,#24076,#24077,#24078));
#5843=EDGE_LOOP('',(#24079,#24080,#24081,#24082,#24083,#24084));
#5844=EDGE_LOOP('',(#24085,#24086,#24087,#24088));
#5845=EDGE_LOOP('',(#24089,#24090,#24091,#24092));
#5846=EDGE_LOOP('',(#24093,#24094,#24095,#24096));
#5847=EDGE_LOOP('',(#24097,#24098,#24099,#24100));
#5848=EDGE_LOOP('',(#24101,#24102,#24103,#24104));
#5849=EDGE_LOOP('',(#24105,#24106,#24107,#24108));
#5850=EDGE_LOOP('',(#24109,#24110,#24111,#24112));
#5851=EDGE_LOOP('',(#24113,#24114,#24115,#24116));
#5852=EDGE_LOOP('',(#24117,#24118,#24119,#24120));
#5853=EDGE_LOOP('',(#24121,#24122,#24123,#24124));
#5854=EDGE_LOOP('',(#24125,#24126,#24127,#24128));
#5855=EDGE_LOOP('',(#24129,#24130,#24131,#24132));
#5856=EDGE_LOOP('',(#24133,#24134,#24135,#24136));
#5857=EDGE_LOOP('',(#24137,#24138,#24139,#24140));
#5858=EDGE_LOOP('',(#24141,#24142,#24143,#24144));
#5859=EDGE_LOOP('',(#24145,#24146,#24147,#24148));
#5860=EDGE_LOOP('',(#24149,#24150,#24151,#24152));
#5861=EDGE_LOOP('',(#24153,#24154,#24155,#24156));
#5862=EDGE_LOOP('',(#24157,#24158,#24159,#24160));
#5863=EDGE_LOOP('',(#24161,#24162,#24163,#24164));
#5864=EDGE_LOOP('',(#24165,#24166,#24167,#24168));
#5865=EDGE_LOOP('',(#24169,#24170,#24171,#24172));
#5866=EDGE_LOOP('',(#24173,#24174,#24175,#24176));
#5867=EDGE_LOOP('',(#24177,#24178,#24179,#24180));
#5868=EDGE_LOOP('',(#24181,#24182,#24183,#24184));
#5869=EDGE_LOOP('',(#24185,#24186,#24187,#24188));
#5870=EDGE_LOOP('',(#24189,#24190,#24191,#24192));
#5871=EDGE_LOOP('',(#24193,#24194,#24195,#24196));
#5872=EDGE_LOOP('',(#24197,#24198,#24199,#24200));
#5873=EDGE_LOOP('',(#24201,#24202,#24203,#24204));
#5874=EDGE_LOOP('',(#24205,#24206,#24207,#24208));
#5875=EDGE_LOOP('',(#24209,#24210,#24211,#24212));
#5876=EDGE_LOOP('',(#24213,#24214,#24215,#24216));
#5877=EDGE_LOOP('',(#24217,#24218,#24219,#24220));
#5878=EDGE_LOOP('',(#24221,#24222,#24223,#24224));
#5879=EDGE_LOOP('',(#24225,#24226,#24227,#24228));
#5880=EDGE_LOOP('',(#24229,#24230,#24231,#24232));
#5881=EDGE_LOOP('',(#24233,#24234,#24235,#24236));
#5882=EDGE_LOOP('',(#24237,#24238,#24239,#24240));
#5883=EDGE_LOOP('',(#24241,#24242,#24243,#24244));
#5884=EDGE_LOOP('',(#24245,#24246,#24247,#24248));
#5885=EDGE_LOOP('',(#24249,#24250,#24251,#24252));
#5886=EDGE_LOOP('',(#24253,#24254,#24255,#24256));
#5887=EDGE_LOOP('',(#24257,#24258,#24259,#24260));
#5888=EDGE_LOOP('',(#24261,#24262,#24263,#24264));
#5889=EDGE_LOOP('',(#24265,#24266,#24267,#24268));
#5890=EDGE_LOOP('',(#24269,#24270,#24271,#24272));
#5891=EDGE_LOOP('',(#24273,#24274,#24275,#24276));
#5892=EDGE_LOOP('',(#24277,#24278,#24279,#24280));
#5893=EDGE_LOOP('',(#24281,#24282,#24283,#24284));
#5894=EDGE_LOOP('',(#24285,#24286,#24287,#24288));
#5895=EDGE_LOOP('',(#24289,#24290,#24291,#24292));
#5896=EDGE_LOOP('',(#24293,#24294,#24295,#24296));
#5897=EDGE_LOOP('',(#24297,#24298,#24299,#24300));
#5898=EDGE_LOOP('',(#24301,#24302,#24303,#24304));
#5899=EDGE_LOOP('',(#24305,#24306,#24307,#24308));
#5900=EDGE_LOOP('',(#24309,#24310,#24311,#24312));
#5901=EDGE_LOOP('',(#24313,#24314,#24315,#24316));
#5902=EDGE_LOOP('',(#24317,#24318,#24319,#24320));
#5903=EDGE_LOOP('',(#24321,#24322,#24323,#24324));
#5904=EDGE_LOOP('',(#24325,#24326,#24327,#24328,#24329));
#5905=EDGE_LOOP('',(#24330,#24331,#24332,#24333));
#5906=EDGE_LOOP('',(#24334,#24335,#24336,#24337));
#5907=EDGE_LOOP('',(#24338,#24339,#24340,#24341));
#5908=EDGE_LOOP('',(#24342,#24343,#24344,#24345));
#5909=EDGE_LOOP('',(#24346,#24347,#24348,#24349));
#5910=EDGE_LOOP('',(#24350,#24351,#24352,#24353));
#5911=EDGE_LOOP('',(#24354,#24355,#24356,#24357));
#5912=EDGE_LOOP('',(#24358,#24359,#24360,#24361));
#5913=EDGE_LOOP('',(#24362,#24363,#24364,#24365));
#5914=EDGE_LOOP('',(#24366,#24367,#24368,#24369));
#5915=EDGE_LOOP('',(#24370,#24371,#24372,#24373));
#5916=EDGE_LOOP('',(#24374,#24375,#24376,#24377));
#5917=EDGE_LOOP('',(#24378,#24379,#24380,#24381));
#5918=EDGE_LOOP('',(#24382,#24383,#24384,#24385));
#5919=EDGE_LOOP('',(#24386,#24387,#24388,#24389));
#5920=EDGE_LOOP('',(#24390,#24391,#24392,#24393));
#5921=EDGE_LOOP('',(#24394,#24395,#24396,#24397));
#5922=EDGE_LOOP('',(#24398,#24399,#24400,#24401));
#5923=EDGE_LOOP('',(#24402,#24403,#24404,#24405));
#5924=EDGE_LOOP('',(#24406,#24407,#24408,#24409));
#5925=EDGE_LOOP('',(#24410,#24411,#24412,#24413));
#5926=EDGE_LOOP('',(#24414,#24415,#24416,#24417));
#5927=EDGE_LOOP('',(#24418,#24419,#24420,#24421));
#5928=EDGE_LOOP('',(#24422,#24423,#24424,#24425));
#5929=EDGE_LOOP('',(#24426,#24427,#24428,#24429));
#5930=EDGE_LOOP('',(#24430,#24431,#24432,#24433));
#5931=EDGE_LOOP('',(#24434,#24435,#24436,#24437));
#5932=EDGE_LOOP('',(#24438,#24439,#24440,#24441));
#5933=EDGE_LOOP('',(#24442,#24443,#24444,#24445));
#5934=EDGE_LOOP('',(#24446,#24447,#24448,#24449));
#5935=EDGE_LOOP('',(#24450,#24451,#24452,#24453));
#5936=EDGE_LOOP('',(#24454,#24455,#24456,#24457));
#5937=EDGE_LOOP('',(#24458,#24459,#24460,#24461));
#5938=EDGE_LOOP('',(#24462,#24463,#24464,#24465));
#5939=EDGE_LOOP('',(#24466,#24467,#24468,#24469));
#5940=EDGE_LOOP('',(#24470,#24471,#24472,#24473));
#5941=EDGE_LOOP('',(#24474,#24475,#24476,#24477));
#5942=EDGE_LOOP('',(#24478,#24479,#24480,#24481));
#5943=EDGE_LOOP('',(#24482,#24483,#24484,#24485));
#5944=EDGE_LOOP('',(#24486,#24487,#24488,#24489));
#5945=EDGE_LOOP('',(#24490,#24491,#24492,#24493));
#5946=EDGE_LOOP('',(#24494,#24495,#24496,#24497));
#5947=EDGE_LOOP('',(#24498,#24499,#24500,#24501));
#5948=EDGE_LOOP('',(#24502,#24503,#24504,#24505));
#5949=EDGE_LOOP('',(#24506,#24507,#24508,#24509));
#5950=EDGE_LOOP('',(#24510,#24511,#24512,#24513));
#5951=EDGE_LOOP('',(#24514,#24515,#24516,#24517));
#5952=EDGE_LOOP('',(#24518,#24519,#24520,#24521));
#5953=EDGE_LOOP('',(#24522,#24523,#24524,#24525));
#5954=EDGE_LOOP('',(#24526,#24527,#24528,#24529));
#5955=EDGE_LOOP('',(#24530,#24531,#24532,#24533));
#5956=EDGE_LOOP('',(#24534,#24535,#24536,#24537));
#5957=EDGE_LOOP('',(#24538,#24539,#24540,#24541));
#5958=EDGE_LOOP('',(#24542,#24543,#24544,#24545));
#5959=EDGE_LOOP('',(#24546,#24547,#24548,#24549));
#5960=EDGE_LOOP('',(#24550,#24551,#24552,#24553));
#5961=EDGE_LOOP('',(#24554,#24555,#24556,#24557));
#5962=EDGE_LOOP('',(#24558,#24559,#24560,#24561));
#5963=EDGE_LOOP('',(#24562,#24563,#24564,#24565));
#5964=EDGE_LOOP('',(#24566,#24567,#24568,#24569));
#5965=EDGE_LOOP('',(#24570,#24571,#24572,#24573));
#5966=EDGE_LOOP('',(#24574,#24575,#24576,#24577));
#5967=EDGE_LOOP('',(#24578,#24579,#24580,#24581));
#5968=EDGE_LOOP('',(#24582,#24583,#24584,#24585));
#5969=EDGE_LOOP('',(#24586,#24587,#24588,#24589));
#5970=EDGE_LOOP('',(#24590,#24591,#24592,#24593));
#5971=EDGE_LOOP('',(#24594,#24595,#24596,#24597));
#5972=EDGE_LOOP('',(#24598,#24599,#24600,#24601));
#5973=EDGE_LOOP('',(#24602,#24603,#24604,#24605));
#5974=EDGE_LOOP('',(#24606,#24607,#24608,#24609));
#5975=EDGE_LOOP('',(#24610,#24611,#24612,#24613));
#5976=EDGE_LOOP('',(#24614,#24615,#24616,#24617));
#5977=EDGE_LOOP('',(#24618,#24619,#24620,#24621));
#5978=EDGE_LOOP('',(#24622,#24623,#24624,#24625));
#5979=EDGE_LOOP('',(#24626,#24627,#24628,#24629));
#5980=EDGE_LOOP('',(#24630,#24631,#24632,#24633));
#5981=EDGE_LOOP('',(#24634,#24635,#24636,#24637));
#5982=EDGE_LOOP('',(#24638,#24639,#24640,#24641));
#5983=EDGE_LOOP('',(#24642,#24643,#24644,#24645));
#5984=EDGE_LOOP('',(#24646,#24647,#24648,#24649));
#5985=EDGE_LOOP('',(#24650,#24651,#24652,#24653));
#5986=EDGE_LOOP('',(#24654,#24655,#24656,#24657));
#5987=EDGE_LOOP('',(#24658,#24659,#24660,#24661));
#5988=EDGE_LOOP('',(#24662,#24663,#24664,#24665));
#5989=EDGE_LOOP('',(#24666,#24667,#24668,#24669));
#5990=EDGE_LOOP('',(#24670,#24671,#24672,#24673));
#5991=EDGE_LOOP('',(#24674,#24675,#24676,#24677));
#5992=EDGE_LOOP('',(#24678,#24679,#24680,#24681));
#5993=EDGE_LOOP('',(#24682,#24683,#24684,#24685));
#5994=EDGE_LOOP('',(#24686,#24687,#24688,#24689));
#5995=EDGE_LOOP('',(#24690,#24691,#24692,#24693));
#5996=EDGE_LOOP('',(#24694,#24695,#24696,#24697));
#5997=EDGE_LOOP('',(#24698,#24699,#24700,#24701,#24702,#24703,#24704,#24705,
#24706,#24707,#24708,#24709,#24710,#24711,#24712,#24713));
#5998=EDGE_LOOP('',(#24714,#24715,#24716,#24717,#24718,#24719,#24720,#24721));
#5999=EDGE_LOOP('',(#24722,#24723,#24724,#24725,#24726,#24727,#24728,#24729,
#24730));
#6000=EDGE_LOOP('',(#24731,#24732,#24733,#24734));
#6001=EDGE_LOOP('',(#24735,#24736,#24737,#24738));
#6002=EDGE_LOOP('',(#24739,#24740,#24741,#24742));
#6003=EDGE_LOOP('',(#24743,#24744,#24745,#24746));
#6004=EDGE_LOOP('',(#24747,#24748,#24749,#24750));
#6005=EDGE_LOOP('',(#24751,#24752,#24753,#24754));
#6006=EDGE_LOOP('',(#24755,#24756,#24757,#24758));
#6007=EDGE_LOOP('',(#24759,#24760,#24761,#24762));
#6008=EDGE_LOOP('',(#24763,#24764,#24765,#24766));
#6009=EDGE_LOOP('',(#24767,#24768,#24769,#24770));
#6010=EDGE_LOOP('',(#24771,#24772,#24773,#24774));
#6011=EDGE_LOOP('',(#24775,#24776,#24777,#24778));
#6012=EDGE_LOOP('',(#24779,#24780,#24781,#24782));
#6013=EDGE_LOOP('',(#24783,#24784,#24785,#24786));
#6014=EDGE_LOOP('',(#24787,#24788,#24789,#24790));
#6015=EDGE_LOOP('',(#24791,#24792,#24793,#24794));
#6016=EDGE_LOOP('',(#24795,#24796,#24797,#24798));
#6017=EDGE_LOOP('',(#24799,#24800,#24801,#24802));
#6018=EDGE_LOOP('',(#24803,#24804,#24805,#24806));
#6019=EDGE_LOOP('',(#24807,#24808,#24809,#24810));
#6020=EDGE_LOOP('',(#24811,#24812,#24813,#24814));
#6021=EDGE_LOOP('',(#24815,#24816,#24817,#24818));
#6022=EDGE_LOOP('',(#24819,#24820,#24821,#24822));
#6023=EDGE_LOOP('',(#24823,#24824,#24825,#24826));
#6024=EDGE_LOOP('',(#24827,#24828,#24829,#24830));
#6025=EDGE_LOOP('',(#24831,#24832,#24833,#24834));
#6026=EDGE_LOOP('',(#24835,#24836,#24837,#24838));
#6027=EDGE_LOOP('',(#24839,#24840,#24841,#24842));
#6028=EDGE_LOOP('',(#24843,#24844,#24845,#24846));
#6029=EDGE_LOOP('',(#24847,#24848,#24849,#24850));
#6030=EDGE_LOOP('',(#24851,#24852,#24853,#24854));
#6031=EDGE_LOOP('',(#24855,#24856,#24857,#24858));
#6032=EDGE_LOOP('',(#24859,#24860,#24861,#24862));
#6033=EDGE_LOOP('',(#24863,#24864,#24865,#24866));
#6034=EDGE_LOOP('',(#24867,#24868,#24869,#24870));
#6035=EDGE_LOOP('',(#24871,#24872,#24873,#24874));
#6036=EDGE_LOOP('',(#24875,#24876,#24877,#24878));
#6037=EDGE_LOOP('',(#24879,#24880,#24881,#24882));
#6038=EDGE_LOOP('',(#24883,#24884,#24885,#24886,#24887,#24888,#24889,#24890,
#24891,#24892,#24893,#24894,#24895,#24896,#24897,#24898));
#6039=EDGE_LOOP('',(#24899,#24900,#24901,#24902,#24903,#24904,#24905,#24906));
#6040=EDGE_LOOP('',(#24907,#24908,#24909,#24910,#24911,#24912,#24913,#24914,
#24915));
#6041=EDGE_LOOP('',(#24916,#24917,#24918,#24919,#24920,#24921,#24922,#24923));
#6042=EDGE_LOOP('',(#24924,#24925,#24926,#24927,#24928,#24929,#24930,#24931,
#24932));
#6043=EDGE_LOOP('',(#24933,#24934,#24935,#24936,#24937,#24938,#24939,#24940));
#6044=EDGE_LOOP('',(#24941,#24942,#24943,#24944,#24945,#24946,#24947,#24948,
#24949));
#6045=EDGE_LOOP('',(#24950,#24951,#24952,#24953,#24954));
#6046=EDGE_LOOP('',(#24955,#24956,#24957,#24958,#24959,#24960,#24961,#24962,
#24963,#24964,#24965,#24966,#24967,#24968,#24969,#24970,#24971,#24972,#24973,
#24974,#24975,#24976,#24977,#24978,#24979,#24980,#24981,#24982,#24983,#24984,
#24985,#24986,#24987,#24988,#24989,#24990,#24991,#24992,#24993,#24994,#24995,
#24996,#24997,#24998,#24999,#25000,#25001,#25002,#25003,#25004,#25005,#25006,
#25007,#25008,#25009,#25010,#25011,#25012,#25013,#25014,#25015,#25016,#25017,
#25018,#25019,#25020,#25021,#25022,#25023,#25024,#25025,#25026,#25027,#25028,
#25029,#25030,#25031,#25032,#25033,#25034,#25035,#25036,#25037,#25038,#25039,
#25040,#25041,#25042,#25043,#25044,#25045,#25046,#25047,#25048,#25049,#25050,
#25051,#25052,#25053,#25054,#25055,#25056,#25057,#25058,#25059,#25060,#25061,
#25062,#25063,#25064,#25065,#25066,#25067,#25068,#25069,#25070,#25071,#25072,
#25073,#25074,#25075,#25076,#25077));
#6047=EDGE_LOOP('',(#25078,#25079,#25080,#25081,#25082));
#6048=EDGE_LOOP('',(#25083,#25084,#25085,#25086));
#6049=EDGE_LOOP('',(#25087,#25088,#25089,#25090,#25091,#25092,#25093,#25094,
#25095,#25096,#25097,#25098,#25099,#25100,#25101,#25102,#25103,#25104,#25105,
#25106,#25107,#25108,#25109,#25110,#25111,#25112,#25113,#25114,#25115,#25116,
#25117,#25118,#25119,#25120,#25121,#25122,#25123,#25124,#25125,#25126,#25127,
#25128,#25129,#25130,#25131,#25132,#25133,#25134,#25135,#25136,#25137,#25138,
#25139,#25140,#25141,#25142,#25143,#25144,#25145,#25146,#25147,#25148,#25149,
#25150,#25151,#25152,#25153,#25154,#25155,#25156,#25157,#25158,#25159,#25160,
#25161,#25162,#25163,#25164,#25165,#25166,#25167,#25168,#25169,#25170,#25171,
#25172,#25173,#25174,#25175,#25176,#25177,#25178,#25179,#25180,#25181,#25182,
#25183,#25184,#25185,#25186,#25187,#25188,#25189,#25190,#25191,#25192,#25193,
#25194,#25195,#25196,#25197,#25198,#25199,#25200,#25201,#25202,#25203,#25204,
#25205,#25206,#25207,#25208));
#6050=EDGE_LOOP('',(#25209,#25210,#25211,#25212,#25213,#25214,#25215));
#6051=EDGE_LOOP('',(#25216,#25217,#25218,#25219,#25220,#25221));
#6052=EDGE_LOOP('',(#25222));
#6053=EDGE_LOOP('',(#25223,#25224,#25225));
#6054=EDGE_LOOP('',(#25226,#25227,#25228,#25229,#25230,#25231,#25232,#25233,
#25234,#25235));
#6055=EDGE_LOOP('',(#25236,#25237,#25238,#25239));
#6056=EDGE_LOOP('',(#25240,#25241,#25242,#25243));
#6057=EDGE_LOOP('',(#25244,#25245,#25246,#25247));
#6058=EDGE_LOOP('',(#25248,#25249,#25250,#25251));
#6059=EDGE_LOOP('',(#25252,#25253,#25254,#25255));
#6060=EDGE_LOOP('',(#25256,#25257,#25258,#25259,#25260));
#6061=EDGE_LOOP('',(#25261));
#6062=EDGE_LOOP('',(#25262,#25263,#25264,#25265,#25266,#25267,#25268,#25269,
#25270,#25271,#25272,#25273,#25274,#25275,#25276,#25277));
#6063=EDGE_LOOP('',(#25278,#25279,#25280,#25281));
#6064=EDGE_LOOP('',(#25282,#25283,#25284,#25285,#25286,#25287,#25288,#25289,
#25290,#25291,#25292,#25293,#25294,#25295,#25296,#25297));
#6065=EDGE_LOOP('',(#25298));
#6066=EDGE_LOOP('',(#25299,#25300,#25301,#25302,#25303,#25304));
#6067=EDGE_LOOP('',(#25305,#25306,#25307,#25308));
#6068=EDGE_LOOP('',(#25309,#25310,#25311,#25312));
#6069=EDGE_LOOP('',(#25313));
#6070=EDGE_LOOP('',(#25314));
#6071=EDGE_LOOP('',(#25315,#25316,#25317,#25318));
#6072=EDGE_LOOP('',(#25319));
#6073=EDGE_LOOP('',(#25320));
#6074=EDGE_LOOP('',(#25321,#25322,#25323,#25324,#25325,#25326,#25327,#25328,
#25329,#25330));
#6075=EDGE_LOOP('',(#25331,#25332,#25333,#25334));
#6076=EDGE_LOOP('',(#25335,#25336,#25337,#25338));
#6077=EDGE_LOOP('',(#25339,#25340,#25341,#25342));
#6078=EDGE_LOOP('',(#25343,#25344,#25345,#25346,#25347,#25348,#25349,#25350,
#25351,#25352));
#6079=EDGE_LOOP('',(#25353,#25354,#25355,#25356));
#6080=EDGE_LOOP('',(#25357,#25358,#25359,#25360));
#6081=EDGE_LOOP('',(#25361,#25362,#25363,#25364,#25365,#25366));
#6082=EDGE_LOOP('',(#25367,#25368,#25369,#25370));
#6083=EDGE_LOOP('',(#25371));
#6084=EDGE_LOOP('',(#25372));
#6085=EDGE_LOOP('',(#25373,#25374,#25375,#25376));
#6086=EDGE_LOOP('',(#25377,#25378,#25379,#25380));
#6087=EDGE_LOOP('',(#25381));
#6088=EDGE_LOOP('',(#25382));
#6089=EDGE_LOOP('',(#25383,#25384,#25385,#25386));
#6090=EDGE_LOOP('',(#25387,#25388,#25389,#25390,#25391));
#6091=EDGE_LOOP('',(#25392,#25393,#25394,#25395,#25396,#25397));
#6092=EDGE_LOOP('',(#25398));
#6093=EDGE_LOOP('',(#25399,#25400,#25401,#25402,#25403,#25404));
#6094=EDGE_LOOP('',(#25405,#25406,#25407,#25408,#25409));
#6095=EDGE_LOOP('',(#25410,#25411,#25412,#25413));
#6096=EDGE_LOOP('',(#25414,#25415,#25416,#25417));
#6097=EDGE_LOOP('',(#25418,#25419,#25420,#25421));
#6098=EDGE_LOOP('',(#25422));
#6099=EDGE_LOOP('',(#25423,#25424,#25425,#25426));
#6100=EDGE_LOOP('',(#25427,#25428,#25429,#25430));
#6101=EDGE_LOOP('',(#25431));
#6102=EDGE_LOOP('',(#25432,#25433,#25434,#25435,#25436));
#6103=EDGE_LOOP('',(#25437,#25438,#25439,#25440,#25441));
#6104=EDGE_LOOP('',(#25442));
#6105=EDGE_LOOP('',(#25443));
#6106=EDGE_LOOP('',(#25444));
#6107=EDGE_LOOP('',(#25445));
#6108=EDGE_LOOP('',(#25446,#25447,#25448,#25449));
#6109=EDGE_LOOP('',(#25450));
#6110=EDGE_LOOP('',(#25451));
#6111=EDGE_LOOP('',(#25452,#25453,#25454,#25455));
#6112=EDGE_LOOP('',(#25456));
#6113=EDGE_LOOP('',(#25457));
#6114=EDGE_LOOP('',(#25458,#25459,#25460,#25461));
#6115=EDGE_LOOP('',(#25462));
#6116=EDGE_LOOP('',(#25463));
#6117=EDGE_LOOP('',(#25464,#25465,#25466,#25467));
#6118=EDGE_LOOP('',(#25468));
#6119=EDGE_LOOP('',(#25469));
#6120=EDGE_LOOP('',(#25470,#25471,#25472,#25473));
#6121=EDGE_LOOP('',(#25474));
#6122=EDGE_LOOP('',(#25475));
#6123=EDGE_LOOP('',(#25476));
#6124=EDGE_LOOP('',(#25477,#25478,#25479,#25480,#25481,#25482,#25483,#25484));
#6125=EDGE_LOOP('',(#25485,#25486,#25487,#25488));
#6126=EDGE_LOOP('',(#25489,#25490,#25491,#25492));
#6127=EDGE_LOOP('',(#25493,#25494,#25495,#25496));
#6128=EDGE_LOOP('',(#25497));
#6129=EDGE_LOOP('',(#25498));
#6130=EDGE_LOOP('',(#25499,#25500,#25501,#25502));
#6131=EDGE_LOOP('',(#25503,#25504,#25505,#25506));
#6132=EDGE_LOOP('',(#25507,#25508,#25509,#25510));
#6133=EDGE_LOOP('',(#25511,#25512,#25513,#25514));
#6134=EDGE_LOOP('',(#25515,#25516,#25517,#25518));
#6135=EDGE_LOOP('',(#25519,#25520,#25521,#25522));
#6136=EDGE_LOOP('',(#25523,#25524,#25525,#25526));
#6137=EDGE_LOOP('',(#25527,#25528,#25529,#25530));
#6138=EDGE_LOOP('',(#25531,#25532,#25533,#25534));
#6139=EDGE_LOOP('',(#25535,#25536,#25537,#25538));
#6140=EDGE_LOOP('',(#25539,#25540,#25541,#25542));
#6141=EDGE_LOOP('',(#25543,#25544,#25545,#25546));
#6142=EDGE_LOOP('',(#25547));
#6143=EDGE_LOOP('',(#25548));
#6144=EDGE_LOOP('',(#25549));
#6145=EDGE_LOOP('',(#25550));
#6146=EDGE_LOOP('',(#25551));
#6147=EDGE_LOOP('',(#25552));
#6148=EDGE_LOOP('',(#25553));
#6149=EDGE_LOOP('',(#25554));
#6150=EDGE_LOOP('',(#25555));
#6151=EDGE_LOOP('',(#25556));
#6152=EDGE_LOOP('',(#25557));
#6153=EDGE_LOOP('',(#25558,#25559,#25560,#25561));
#6154=EDGE_LOOP('',(#25562,#25563,#25564,#25565));
#6155=EDGE_LOOP('',(#25566,#25567,#25568,#25569));
#6156=EDGE_LOOP('',(#25570,#25571,#25572,#25573));
#6157=EDGE_LOOP('',(#25574,#25575,#25576,#25577));
#6158=EDGE_LOOP('',(#25578,#25579,#25580,#25581));
#6159=EDGE_LOOP('',(#25582,#25583,#25584,#25585));
#6160=EDGE_LOOP('',(#25586,#25587,#25588,#25589));
#6161=EDGE_LOOP('',(#25590,#25591,#25592,#25593));
#6162=EDGE_LOOP('',(#25594,#25595,#25596,#25597));
#6163=EDGE_LOOP('',(#25598,#25599,#25600,#25601));
#6164=EDGE_LOOP('',(#25602,#25603,#25604,#25605));
#6165=EDGE_LOOP('',(#25606,#25607,#25608,#25609));
#6166=EDGE_LOOP('',(#25610,#25611,#25612,#25613));
#6167=EDGE_LOOP('',(#25614,#25615,#25616,#25617));
#6168=EDGE_LOOP('',(#25618));
#6169=EDGE_LOOP('',(#25619));
#6170=EDGE_LOOP('',(#25620));
#6171=EDGE_LOOP('',(#25621));
#6172=EDGE_LOOP('',(#25622));
#6173=EDGE_LOOP('',(#25623));
#6174=EDGE_LOOP('',(#25624));
#6175=EDGE_LOOP('',(#25625));
#6176=EDGE_LOOP('',(#25626));
#6177=EDGE_LOOP('',(#25627));
#6178=EDGE_LOOP('',(#25628));
#6179=EDGE_LOOP('',(#25629,#25630,#25631,#25632));
#6180=EDGE_LOOP('',(#25633,#25634,#25635,#25636));
#6181=EDGE_LOOP('',(#25637,#25638,#25639,#25640));
#6182=EDGE_LOOP('',(#25641,#25642,#25643,#25644));
#6183=EDGE_LOOP('',(#25645,#25646,#25647,#25648));
#6184=EDGE_LOOP('',(#25649,#25650,#25651,#25652));
#6185=EDGE_LOOP('',(#25653,#25654,#25655,#25656));
#6186=EDGE_LOOP('',(#25657,#25658,#25659,#25660));
#6187=EDGE_LOOP('',(#25661,#25662,#25663,#25664));
#6188=EDGE_LOOP('',(#25665,#25666,#25667,#25668));
#6189=EDGE_LOOP('',(#25669,#25670,#25671,#25672));
#6190=EDGE_LOOP('',(#25673,#25674,#25675,#25676));
#6191=EDGE_LOOP('',(#25677,#25678,#25679,#25680));
#6192=EDGE_LOOP('',(#25681,#25682,#25683,#25684));
#6193=EDGE_LOOP('',(#25685,#25686,#25687,#25688));
#6194=EDGE_LOOP('',(#25689,#25690,#25691,#25692));
#6195=EDGE_LOOP('',(#25693,#25694,#25695,#25696));
#6196=EDGE_LOOP('',(#25697,#25698,#25699,#25700));
#6197=EDGE_LOOP('',(#25701,#25702,#25703,#25704));
#6198=EDGE_LOOP('',(#25705,#25706,#25707,#25708));
#6199=EDGE_LOOP('',(#25709,#25710,#25711,#25712,#25713,#25714,#25715,#25716));
#6200=EDGE_LOOP('',(#25717,#25718,#25719,#25720,#25721,#25722,#25723,#25724));
#6201=EDGE_LOOP('',(#25725,#25726,#25727,#25728));
#6202=EDGE_LOOP('',(#25729,#25730,#25731,#25732));
#6203=EDGE_LOOP('',(#25733,#25734,#25735,#25736));
#6204=EDGE_LOOP('',(#25737,#25738,#25739,#25740));
#6205=EDGE_LOOP('',(#25741,#25742,#25743,#25744));
#6206=EDGE_LOOP('',(#25745,#25746,#25747,#25748));
#6207=EDGE_LOOP('',(#25749,#25750,#25751,#25752));
#6208=EDGE_LOOP('',(#25753,#25754,#25755,#25756));
#6209=EDGE_LOOP('',(#25757,#25758,#25759,#25760));
#6210=EDGE_LOOP('',(#25761,#25762,#25763,#25764));
#6211=EDGE_LOOP('',(#25765,#25766,#25767,#25768));
#6212=EDGE_LOOP('',(#25769,#25770,#25771,#25772));
#6213=EDGE_LOOP('',(#25773,#25774,#25775,#25776));
#6214=EDGE_LOOP('',(#25777,#25778,#25779,#25780));
#6215=EDGE_LOOP('',(#25781,#25782,#25783,#25784));
#6216=EDGE_LOOP('',(#25785,#25786,#25787,#25788));
#6217=EDGE_LOOP('',(#25789,#25790,#25791,#25792));
#6218=EDGE_LOOP('',(#25793,#25794,#25795,#25796));
#6219=EDGE_LOOP('',(#25797,#25798,#25799,#25800));
#6220=EDGE_LOOP('',(#25801,#25802,#25803,#25804));
#6221=EDGE_LOOP('',(#25805));
#6222=EDGE_LOOP('',(#25806));
#6223=EDGE_LOOP('',(#25807));
#6224=EDGE_LOOP('',(#25808));
#6225=EDGE_LOOP('',(#25809));
#6226=EDGE_LOOP('',(#25810));
#6227=EDGE_LOOP('',(#25811));
#6228=EDGE_LOOP('',(#25812));
#6229=EDGE_LOOP('',(#25813));
#6230=EDGE_LOOP('',(#25814));
#6231=EDGE_LOOP('',(#25815));
#6232=EDGE_LOOP('',(#25816,#25817,#25818,#25819));
#6233=EDGE_LOOP('',(#25820,#25821,#25822,#25823));
#6234=EDGE_LOOP('',(#25824,#25825,#25826,#25827));
#6235=EDGE_LOOP('',(#25828,#25829,#25830,#25831));
#6236=EDGE_LOOP('',(#25832,#25833,#25834,#25835));
#6237=EDGE_LOOP('',(#25836,#25837,#25838,#25839));
#6238=EDGE_LOOP('',(#25840,#25841,#25842,#25843));
#6239=EDGE_LOOP('',(#25844,#25845,#25846,#25847));
#6240=EDGE_LOOP('',(#25848));
#6241=EDGE_LOOP('',(#25849));
#6242=EDGE_LOOP('',(#25850));
#6243=EDGE_LOOP('',(#25851));
#6244=EDGE_LOOP('',(#25852));
#6245=EDGE_LOOP('',(#25853));
#6246=EDGE_LOOP('',(#25854));
#6247=EDGE_LOOP('',(#25855));
#6248=EDGE_LOOP('',(#25856));
#6249=EDGE_LOOP('',(#25857));
#6250=EDGE_LOOP('',(#25858));
#6251=EDGE_LOOP('',(#25859,#25860,#25861,#25862));
#6252=EDGE_LOOP('',(#25863,#25864,#25865,#25866));
#6253=EDGE_LOOP('',(#25867,#25868,#25869,#25870));
#6254=EDGE_LOOP('',(#25871,#25872,#25873,#25874));
#6255=EDGE_LOOP('',(#25875,#25876,#25877,#25878));
#6256=EDGE_LOOP('',(#25879,#25880,#25881,#25882));
#6257=EDGE_LOOP('',(#25883,#25884,#25885,#25886));
#6258=EDGE_LOOP('',(#25887,#25888,#25889,#25890));
#6259=EDGE_LOOP('',(#25891,#25892,#25893,#25894));
#6260=EDGE_LOOP('',(#25895,#25896,#25897,#25898));
#6261=EDGE_LOOP('',(#25899,#25900,#25901,#25902));
#6262=EDGE_LOOP('',(#25903,#25904,#25905,#25906));
#6263=EDGE_LOOP('',(#25907,#25908,#25909,#25910));
#6264=EDGE_LOOP('',(#25911,#25912,#25913,#25914));
#6265=EDGE_LOOP('',(#25915,#25916,#25917,#25918));
#6266=EDGE_LOOP('',(#25919,#25920,#25921,#25922));
#6267=EDGE_LOOP('',(#25923,#25924,#25925,#25926));
#6268=EDGE_LOOP('',(#25927,#25928,#25929,#25930));
#6269=EDGE_LOOP('',(#25931,#25932,#25933,#25934));
#6270=EDGE_LOOP('',(#25935,#25936,#25937,#25938));
#6271=EDGE_LOOP('',(#25939,#25940,#25941,#25942));
#6272=EDGE_LOOP('',(#25943,#25944,#25945,#25946));
#6273=EDGE_LOOP('',(#25947,#25948,#25949,#25950));
#6274=EDGE_LOOP('',(#25951,#25952,#25953,#25954));
#6275=EDGE_LOOP('',(#25955,#25956,#25957,#25958));
#6276=EDGE_LOOP('',(#25959,#25960,#25961,#25962));
#6277=EDGE_LOOP('',(#25963,#25964,#25965,#25966));
#6278=EDGE_LOOP('',(#25967,#25968,#25969,#25970));
#6279=EDGE_LOOP('',(#25971,#25972,#25973,#25974));
#6280=EDGE_LOOP('',(#25975,#25976,#25977,#25978));
#6281=EDGE_LOOP('',(#25979,#25980,#25981,#25982));
#6282=EDGE_LOOP('',(#25983,#25984,#25985,#25986));
#6283=EDGE_LOOP('',(#25987,#25988,#25989,#25990));
#6284=EDGE_LOOP('',(#25991,#25992,#25993,#25994));
#6285=EDGE_LOOP('',(#25995,#25996,#25997,#25998));
#6286=EDGE_LOOP('',(#25999,#26000,#26001,#26002));
#6287=EDGE_LOOP('',(#26003,#26004,#26005,#26006,#26007,#26008,#26009,#26010));
#6288=EDGE_LOOP('',(#26011,#26012,#26013,#26014,#26015,#26016,#26017,#26018));
#6289=EDGE_LOOP('',(#26019,#26020,#26021,#26022));
#6290=EDGE_LOOP('',(#26023,#26024,#26025,#26026));
#6291=EDGE_LOOP('',(#26027,#26028,#26029,#26030));
#6292=EDGE_LOOP('',(#26031,#26032,#26033,#26034));
#6293=EDGE_LOOP('',(#26035,#26036,#26037,#26038));
#6294=EDGE_LOOP('',(#26039,#26040,#26041,#26042));
#6295=EDGE_LOOP('',(#26043,#26044,#26045,#26046));
#6296=EDGE_LOOP('',(#26047,#26048,#26049,#26050));
#6297=EDGE_LOOP('',(#26051,#26052,#26053,#26054));
#6298=EDGE_LOOP('',(#26055,#26056,#26057,#26058));
#6299=EDGE_LOOP('',(#26059,#26060,#26061,#26062));
#6300=EDGE_LOOP('',(#26063,#26064,#26065,#26066));
#6301=EDGE_LOOP('',(#26067,#26068,#26069,#26070));
#6302=LINE('',#37682,#8790);
#6303=LINE('',#37684,#8791);
#6304=LINE('',#37686,#8792);
#6305=LINE('',#37688,#8793);
#6306=LINE('',#37689,#8794);
#6307=LINE('',#37692,#8795);
#6308=LINE('',#37694,#8796);
#6309=LINE('',#37696,#8797);
#6310=LINE('',#37698,#8798);
#6311=LINE('',#37699,#8799);
#6312=LINE('',#37702,#8800);
#6313=LINE('',#37703,#8801);
#6314=LINE('',#37706,#8802);
#6315=LINE('',#37707,#8803);
#6316=LINE('',#37710,#8804);
#6317=LINE('',#37711,#8805);
#6318=LINE('',#37714,#8806);
#6319=LINE('',#37716,#8807);
#6320=LINE('',#37718,#8808);
#6321=LINE('',#37719,#8809);
#6322=LINE('',#37722,#8810);
#6323=LINE('',#37724,#8811);
#6324=LINE('',#37726,#8812);
#6325=LINE('',#37728,#8813);
#6326=LINE('',#37730,#8814);
#6327=LINE('',#37731,#8815);
#6328=LINE('',#37735,#8816);
#6329=LINE('',#37737,#8817);
#6330=LINE('',#37739,#8818);
#6331=LINE('',#37741,#8819);
#6332=LINE('',#37742,#8820);
#6333=LINE('',#37745,#8821);
#6334=LINE('',#37747,#8822);
#6335=LINE('',#37748,#8823);
#6336=LINE('',#37751,#8824);
#6337=LINE('',#37752,#8825);
#6338=LINE('',#37753,#8826);
#6339=LINE('',#37755,#8827);
#6340=LINE('',#37756,#8828);
#6341=LINE('',#37758,#8829);
#6342=LINE('',#37759,#8830);
#6343=LINE('',#37762,#8831);
#6344=LINE('',#37763,#8832);
#6345=LINE('',#37769,#8833);
#6346=LINE('',#37774,#8834);
#6347=LINE('',#37776,#8835);
#6348=LINE('',#37778,#8836);
#6349=LINE('',#37779,#8837);
#6350=LINE('',#37788,#8838);
#6351=LINE('',#37792,#8839);
#6352=LINE('',#37796,#8840);
#6353=LINE('',#37800,#8841);
#6354=LINE('',#37804,#8842);
#6355=LINE('',#37808,#8843);
#6356=LINE('',#37812,#8844);
#6357=LINE('',#37817,#8845);
#6358=LINE('',#37821,#8846);
#6359=LINE('',#37823,#8847);
#6360=LINE('',#37825,#8848);
#6361=LINE('',#37826,#8849);
#6362=LINE('',#37834,#8850);
#6363=LINE('',#37836,#8851);
#6364=LINE('',#37838,#8852);
#6365=LINE('',#37843,#8853);
#6366=LINE('',#37848,#8854);
#6367=LINE('',#37850,#8855);
#6368=LINE('',#37852,#8856);
#6369=LINE('',#37853,#8857);
#6370=LINE('',#37863,#8858);
#6371=LINE('',#37866,#8859);
#6372=LINE('',#37871,#8860);
#6373=LINE('',#37874,#8861);
#6374=LINE('',#37879,#8862);
#6375=LINE('',#37882,#8863);
#6376=LINE('',#37887,#8864);
#6377=LINE('',#37891,#8865);
#6378=LINE('',#37897,#8866);
#6379=LINE('',#37937,#8867);
#6380=LINE('',#37949,#8868);
#6381=LINE('',#38009,#8869);
#6382=LINE('',#38013,#8870);
#6383=LINE('',#38017,#8871);
#6384=LINE('',#38039,#8872);
#6385=LINE('',#38042,#8873);
#6386=LINE('',#38097,#8874);
#6387=LINE('',#38101,#8875);
#6388=LINE('',#38103,#8876);
#6389=LINE('',#38105,#8877);
#6390=LINE('',#38106,#8878);
#6391=LINE('',#38114,#8879);
#6392=LINE('',#38116,#8880);
#6393=LINE('',#38118,#8881);
#6394=LINE('',#38122,#8882);
#6395=LINE('',#38126,#8883);
#6396=LINE('',#38130,#8884);
#6397=LINE('',#38131,#8885);
#6398=LINE('',#38132,#8886);
#6399=LINE('',#38135,#8887);
#6400=LINE('',#38139,#8888);
#6401=LINE('',#38141,#8889);
#6402=LINE('',#38142,#8890);
#6403=LINE('',#38145,#8891);
#6404=LINE('',#38150,#8892);
#6405=LINE('',#38151,#8893);
#6406=LINE('',#38155,#8894);
#6407=LINE('',#38159,#8895);
#6408=LINE('',#38160,#8896);
#6409=LINE('',#38162,#8897);
#6410=LINE('',#38164,#8898);
#6411=LINE('',#38166,#8899);
#6412=LINE('',#38169,#8900);
#6413=LINE('',#38172,#8901);
#6414=LINE('',#38195,#8902);
#6415=LINE('',#38219,#8903);
#6416=LINE('',#38222,#8904);
#6417=LINE('',#38226,#8905);
#6418=LINE('',#38230,#8906);
#6419=LINE('',#38234,#8907);
#6420=LINE('',#38238,#8908);
#6421=LINE('',#38242,#8909);
#6422=LINE('',#38244,#8910);
#6423=LINE('',#38248,#8911);
#6424=LINE('',#38249,#8912);
#6425=LINE('',#38250,#8913);
#6426=LINE('',#38253,#8914);
#6427=LINE('',#38257,#8915);
#6428=LINE('',#38258,#8916);
#6429=LINE('',#38262,#8917);
#6430=LINE('',#38267,#8918);
#6431=LINE('',#38268,#8919);
#6432=LINE('',#38269,#8920);
#6433=LINE('',#38272,#8921);
#6434=LINE('',#38275,#8922);
#6435=LINE('',#38276,#8923);
#6436=LINE('',#38278,#8924);
#6437=LINE('',#38325,#8925);
#6438=LINE('',#38327,#8926);
#6439=LINE('',#38329,#8927);
#6440=LINE('',#38331,#8928);
#6441=LINE('',#38333,#8929);
#6442=LINE('',#38335,#8930);
#6443=LINE('',#38337,#8931);
#6444=LINE('',#38338,#8932);
#6445=LINE('',#38393,#8933);
#6446=LINE('',#38395,#8934);
#6447=LINE('',#38397,#8935);
#6448=LINE('',#38431,#8936);
#6449=LINE('',#38473,#8937);
#6450=LINE('',#38475,#8938);
#6451=LINE('',#38477,#8939);
#6452=LINE('',#38479,#8940);
#6453=LINE('',#38481,#8941);
#6454=LINE('',#38483,#8942);
#6455=LINE('',#38485,#8943);
#6456=LINE('',#38487,#8944);
#6457=LINE('',#38489,#8945);
#6458=LINE('',#38490,#8946);
#6459=LINE('',#38494,#8947);
#6460=LINE('',#38498,#8948);
#6461=LINE('',#38502,#8949);
#6462=LINE('',#38506,#8950);
#6463=LINE('',#38510,#8951);
#6464=LINE('',#38515,#8952);
#6465=LINE('',#38561,#8953);
#6466=LINE('',#38563,#8954);
#6467=LINE('',#38617,#8955);
#6468=LINE('',#38665,#8956);
#6469=LINE('',#38670,#8957);
#6470=LINE('',#38712,#8958);
#6471=LINE('',#38714,#8959);
#6472=LINE('',#38767,#8960);
#6473=LINE('',#38821,#8961);
#6474=LINE('',#38823,#8962);
#6475=LINE('',#38824,#8963);
#6476=LINE('',#38827,#8964);
#6477=LINE('',#38831,#8965);
#6478=LINE('',#38832,#8966);
#6479=LINE('',#38834,#8967);
#6480=LINE('',#38837,#8968);
#6481=LINE('',#38840,#8969);
#6482=LINE('',#38844,#8970);
#6483=LINE('',#38845,#8971);
#6484=LINE('',#38850,#8972);
#6485=LINE('',#38854,#8973);
#6486=LINE('',#38855,#8974);
#6487=LINE('',#38858,#8975);
#6488=LINE('',#38908,#8976);
#6489=LINE('',#38956,#8977);
#6490=LINE('',#38960,#8978);
#6491=LINE('',#38964,#8979);
#6492=LINE('',#38968,#8980);
#6493=LINE('',#38969,#8981);
#6494=LINE('',#39052,#8982);
#6495=LINE('',#39053,#8983);
#6496=LINE('',#39055,#8984);
#6497=LINE('',#39056,#8985);
#6498=LINE('',#39090,#8986);
#6499=LINE('',#39091,#8987);
#6500=LINE('',#39095,#8988);
#6501=LINE('',#39098,#8989);
#6502=LINE('',#39099,#8990);
#6503=LINE('',#39102,#8991);
#6504=LINE('',#39104,#8992);
#6505=LINE('',#39106,#8993);
#6506=LINE('',#39108,#8994);
#6507=LINE('',#39111,#8995);
#6508=LINE('',#39113,#8996);
#6509=LINE('',#39298,#8997);
#6510=LINE('',#39299,#8998);
#6511=LINE('',#39301,#8999);
#6512=LINE('',#39302,#9000);
#6513=LINE('',#39431,#9001);
#6514=LINE('',#39432,#9002);
#6515=LINE('',#39434,#9003);
#6516=LINE('',#39435,#9004);
#6517=LINE('',#39470,#9005);
#6518=LINE('',#39475,#9006);
#6519=LINE('',#39517,#9007);
#6520=LINE('',#39519,#9008);
#6521=LINE('',#39572,#9009);
#6522=LINE('',#39690,#9010);
#6523=LINE('',#39691,#9011);
#6524=LINE('',#39693,#9012);
#6525=LINE('',#39694,#9013);
#6526=LINE('',#39730,#9014);
#6527=LINE('',#39734,#9015);
#6528=LINE('',#39739,#9016);
#6529=LINE('',#39740,#9017);
#6530=LINE('',#39741,#9018);
#6531=LINE('',#39745,#9019);
#6532=LINE('',#39751,#9020);
#6533=LINE('',#39752,#9021);
#6534=LINE('',#39753,#9022);
#6535=LINE('',#39756,#9023);
#6536=LINE('',#39761,#9024);
#6537=LINE('',#39762,#9025);
#6538=LINE('',#39766,#9026);
#6539=LINE('',#39770,#9027);
#6540=LINE('',#39771,#9028);
#6541=LINE('',#39774,#9029);
#6542=LINE('',#39775,#9030);
#6543=LINE('',#39777,#9031);
#6544=LINE('',#39781,#9032);
#6545=LINE('',#39782,#9033);
#6546=LINE('',#39785,#9034);
#6547=LINE('',#39808,#9035);
#6548=LINE('',#39831,#9036);
#6549=LINE('',#39834,#9037);
#6550=LINE('',#39835,#9038);
#6551=LINE('',#39839,#9039);
#6552=LINE('',#39843,#9040);
#6553=LINE('',#39847,#9041);
#6554=LINE('',#39851,#9042);
#6555=LINE('',#39855,#9043);
#6556=LINE('',#39857,#9044);
#6557=LINE('',#39861,#9045);
#6558=LINE('',#39862,#9046);
#6559=LINE('',#39863,#9047);
#6560=LINE('',#39866,#9048);
#6561=LINE('',#39870,#9049);
#6562=LINE('',#39871,#9050);
#6563=LINE('',#39875,#9051);
#6564=LINE('',#39880,#9052);
#6565=LINE('',#39882,#9053);
#6566=LINE('',#39883,#9054);
#6567=LINE('',#39887,#9055);
#6568=LINE('',#39891,#9056);
#6569=LINE('',#39892,#9057);
#6570=LINE('',#39894,#9058);
#6571=LINE('',#39895,#9059);
#6572=LINE('',#39898,#9060);
#6573=LINE('',#39921,#9061);
#6574=LINE('',#39944,#9062);
#6575=LINE('',#39953,#9063);
#6576=LINE('',#39957,#9064);
#6577=LINE('',#39961,#9065);
#6578=LINE('',#39965,#9066);
#6579=LINE('',#40008,#9067);
#6580=LINE('',#40010,#9068);
#6581=LINE('',#40023,#9069);
#6582=LINE('',#40028,#9070);
#6583=LINE('',#40071,#9071);
#6584=LINE('',#40122,#9072);
#6585=LINE('',#40124,#9073);
#6586=LINE('',#40125,#9074);
#6587=LINE('',#40129,#9075);
#6588=LINE('',#40132,#9076);
#6589=LINE('',#40133,#9077);
#6590=LINE('',#40136,#9078);
#6591=LINE('',#40138,#9079);
#6592=LINE('',#40142,#9080);
#6593=LINE('',#40145,#9081);
#6594=LINE('',#40146,#9082);
#6595=LINE('',#40151,#9083);
#6596=LINE('',#40155,#9084);
#6597=LINE('',#40156,#9085);
#6598=LINE('',#40159,#9086);
#6599=LINE('',#40204,#9087);
#6600=LINE('',#40254,#9088);
#6601=LINE('',#40258,#9089);
#6602=LINE('',#40262,#9090);
#6603=LINE('',#40266,#9091);
#6604=LINE('',#40267,#9092);
#6605=LINE('',#40271,#9093);
#6606=LINE('',#40272,#9094);
#6607=LINE('',#40274,#9095);
#6608=LINE('',#40276,#9096);
#6609=LINE('',#40278,#9097);
#6610=LINE('',#40280,#9098);
#6611=LINE('',#40283,#9099);
#6612=LINE('',#40287,#9100);
#6613=LINE('',#40288,#9101);
#6614=LINE('',#40292,#9102);
#6615=LINE('',#40294,#9103);
#6616=LINE('',#40466,#9104);
#6617=LINE('',#40467,#9105);
#6618=LINE('',#40469,#9106);
#6619=LINE('',#40470,#9107);
#6620=LINE('',#40505,#9108);
#6621=LINE('',#40510,#9109);
#6622=LINE('',#40552,#9110);
#6623=LINE('',#40554,#9111);
#6624=LINE('',#40607,#9112);
#6625=LINE('',#40733,#9113);
#6626=LINE('',#40734,#9114);
#6627=LINE('',#40736,#9115);
#6628=LINE('',#40737,#9116);
#6629=LINE('',#40815,#9117);
#6630=LINE('',#40817,#9118);
#6631=LINE('',#40831,#9119);
#6632=LINE('',#40836,#9120);
#6633=LINE('',#40879,#9121);
#6634=LINE('',#41009,#9122);
#6635=LINE('',#41010,#9123);
#6636=LINE('',#41012,#9124);
#6637=LINE('',#41013,#9125);
#6638=LINE('',#41048,#9126);
#6639=LINE('',#41053,#9127);
#6640=LINE('',#41095,#9128);
#6641=LINE('',#41097,#9129);
#6642=LINE('',#41150,#9130);
#6643=LINE('',#41276,#9131);
#6644=LINE('',#41277,#9132);
#6645=LINE('',#41279,#9133);
#6646=LINE('',#41280,#9134);
#6647=LINE('',#41317,#9135);
#6648=LINE('',#41321,#9136);
#6649=LINE('',#41329,#9137);
#6650=LINE('',#41331,#9138);
#6651=LINE('',#41336,#9139);
#6652=LINE('',#41340,#9140);
#6653=LINE('',#41343,#9141);
#6654=LINE('',#41356,#9142);
#6655=LINE('',#41361,#9143);
#6656=LINE('',#41373,#9144);
#6657=LINE('',#41388,#9145);
#6658=LINE('',#41403,#9146);
#6659=LINE('',#41418,#9147);
#6660=LINE('',#41433,#9148);
#6661=LINE('',#41448,#9149);
#6662=LINE('',#41471,#9150);
#6663=LINE('',#41476,#9151);
#6664=LINE('',#41484,#9152);
#6665=LINE('',#41495,#9153);
#6666=LINE('',#41506,#9154);
#6667=LINE('',#41517,#9155);
#6668=LINE('',#41528,#9156);
#6669=LINE('',#41539,#9157);
#6670=LINE('',#41550,#9158);
#6671=LINE('',#41561,#9159);
#6672=LINE('',#41577,#9160);
#6673=LINE('',#41579,#9161);
#6674=LINE('',#41580,#9162);
#6675=LINE('',#41583,#9163);
#6676=LINE('',#41584,#9164);
#6677=LINE('',#41587,#9165);
#6678=LINE('',#41588,#9166);
#6679=LINE('',#41591,#9167);
#6680=LINE('',#41592,#9168);
#6681=LINE('',#41595,#9169);
#6682=LINE('',#41596,#9170);
#6683=LINE('',#41599,#9171);
#6684=LINE('',#41600,#9172);
#6685=LINE('',#41603,#9173);
#6686=LINE('',#41604,#9174);
#6687=LINE('',#41606,#9175);
#6688=LINE('',#41620,#9176);
#6689=LINE('',#41625,#9177);
#6690=LINE('',#41637,#9178);
#6691=LINE('',#41652,#9179);
#6692=LINE('',#41667,#9180);
#6693=LINE('',#41682,#9181);
#6694=LINE('',#41697,#9182);
#6695=LINE('',#41712,#9183);
#6696=LINE('',#41727,#9184);
#6697=LINE('',#41750,#9185);
#6698=LINE('',#41755,#9186);
#6699=LINE('',#41763,#9187);
#6700=LINE('',#41774,#9188);
#6701=LINE('',#41785,#9189);
#6702=LINE('',#41796,#9190);
#6703=LINE('',#41807,#9191);
#6704=LINE('',#41818,#9192);
#6705=LINE('',#41829,#9193);
#6706=LINE('',#41840,#9194);
#6707=LINE('',#41851,#9195);
#6708=LINE('',#41862,#9196);
#6709=LINE('',#41873,#9197);
#6710=LINE('',#41889,#9198);
#6711=LINE('',#41891,#9199);
#6712=LINE('',#41892,#9200);
#6713=LINE('',#41900,#9201);
#6714=LINE('',#41911,#9202);
#6715=LINE('',#41922,#9203);
#6716=LINE('',#41933,#9204);
#6717=LINE('',#41944,#9205);
#6718=LINE('',#41955,#9206);
#6719=LINE('',#41966,#9207);
#6720=LINE('',#41977,#9208);
#6721=LINE('',#41988,#9209);
#6722=LINE('',#41999,#9210);
#6723=LINE('',#42005,#9211);
#6724=LINE('',#42006,#9212);
#6725=LINE('',#42014,#9213);
#6726=LINE('',#42025,#9214);
#6727=LINE('',#42036,#9215);
#6728=LINE('',#42047,#9216);
#6729=LINE('',#42058,#9217);
#6730=LINE('',#42069,#9218);
#6731=LINE('',#42080,#9219);
#6732=LINE('',#42091,#9220);
#6733=LINE('',#42097,#9221);
#6734=LINE('',#42098,#9222);
#6735=LINE('',#42100,#9223);
#6736=LINE('',#42104,#9224);
#6737=LINE('',#42106,#9225);
#6738=LINE('',#42107,#9226);
#6739=LINE('',#42110,#9227);
#6740=LINE('',#42111,#9228);
#6741=LINE('',#42114,#9229);
#6742=LINE('',#42115,#9230);
#6743=LINE('',#42118,#9231);
#6744=LINE('',#42119,#9232);
#6745=LINE('',#42122,#9233);
#6746=LINE('',#42123,#9234);
#6747=LINE('',#42126,#9235);
#6748=LINE('',#42127,#9236);
#6749=LINE('',#42130,#9237);
#6750=LINE('',#42131,#9238);
#6751=LINE('',#42134,#9239);
#6752=LINE('',#42135,#9240);
#6753=LINE('',#42138,#9241);
#6754=LINE('',#42139,#9242);
#6755=LINE('',#42141,#9243);
#6756=LINE('',#42146,#9244);
#6757=LINE('',#42148,#9245);
#6758=LINE('',#42157,#9246);
#6759=LINE('',#42159,#9247);
#6760=LINE('',#42161,#9248);
#6761=LINE('',#42162,#9249);
#6762=LINE('',#42165,#9250);
#6763=LINE('',#42167,#9251);
#6764=LINE('',#42169,#9252);
#6765=LINE('',#42170,#9253);
#6766=LINE('',#42173,#9254);
#6767=LINE('',#42175,#9255);
#6768=LINE('',#42176,#9256);
#6769=LINE('',#42179,#9257);
#6770=LINE('',#42180,#9258);
#6771=LINE('',#42183,#9259);
#6772=LINE('',#42185,#9260);
#6773=LINE('',#42187,#9261);
#6774=LINE('',#42188,#9262);
#6775=LINE('',#42192,#9263);
#6776=LINE('',#42194,#9264);
#6777=LINE('',#42196,#9265);
#6778=LINE('',#42198,#9266);
#6779=LINE('',#42199,#9267);
#6780=LINE('',#42202,#9268);
#6781=LINE('',#42204,#9269);
#6782=LINE('',#42205,#9270);
#6783=LINE('',#42208,#9271);
#6784=LINE('',#42210,#9272);
#6785=LINE('',#42212,#9273);
#6786=LINE('',#42213,#9274);
#6787=LINE('',#42216,#9275);
#6788=LINE('',#42218,#9276);
#6789=LINE('',#42220,#9277);
#6790=LINE('',#42222,#9278);
#6791=LINE('',#42223,#9279);
#6792=LINE('',#42226,#9280);
#6793=LINE('',#42227,#9281);
#6794=LINE('',#42230,#9282);
#6795=LINE('',#42231,#9283);
#6796=LINE('',#42234,#9284);
#6797=LINE('',#42235,#9285);
#6798=LINE('',#42238,#9286);
#6799=LINE('',#42240,#9287);
#6800=LINE('',#42242,#9288);
#6801=LINE('',#42243,#9289);
#6802=LINE('',#42247,#9290);
#6803=LINE('',#42249,#9291);
#6804=LINE('',#42251,#9292);
#6805=LINE('',#42253,#9293);
#6806=LINE('',#42255,#9294);
#6807=LINE('',#42256,#9295);
#6808=LINE('',#42259,#9296);
#6809=LINE('',#42261,#9297);
#6810=LINE('',#42263,#9298);
#6811=LINE('',#42264,#9299);
#6812=LINE('',#42267,#9300);
#6813=LINE('',#42269,#9301);
#6814=LINE('',#42271,#9302);
#6815=LINE('',#42272,#9303);
#6816=LINE('',#42274,#9304);
#6817=LINE('',#42276,#9305);
#6818=LINE('',#42278,#9306);
#6819=LINE('',#42279,#9307);
#6820=LINE('',#42283,#9308);
#6821=LINE('',#42285,#9309);
#6822=LINE('',#42287,#9310);
#6823=LINE('',#42289,#9311);
#6824=LINE('',#42290,#9312);
#6825=LINE('',#42293,#9313);
#6826=LINE('',#42295,#9314);
#6827=LINE('',#42297,#9315);
#6828=LINE('',#42298,#9316);
#6829=LINE('',#42301,#9317);
#6830=LINE('',#42302,#9318);
#6831=LINE('',#42304,#9319);
#6832=LINE('',#42305,#9320);
#6833=LINE('',#42308,#9321);
#6834=LINE('',#42310,#9322);
#6835=LINE('',#42312,#9323);
#6836=LINE('',#42313,#9324);
#6837=LINE('',#42316,#9325);
#6838=LINE('',#42318,#9326);
#6839=LINE('',#42320,#9327);
#6840=LINE('',#42321,#9328);
#6841=LINE('',#42324,#9329);
#6842=LINE('',#42325,#9330);
#6843=LINE('',#42328,#9331);
#6844=LINE('',#42330,#9332);
#6845=LINE('',#42331,#9333);
#6846=LINE('',#42334,#9334);
#6847=LINE('',#42336,#9335);
#6848=LINE('',#42337,#9336);
#6849=LINE('',#42339,#9337);
#6850=LINE('',#42341,#9338);
#6851=LINE('',#42342,#9339);
#6852=LINE('',#42345,#9340);
#6853=LINE('',#42347,#9341);
#6854=LINE('',#42349,#9342);
#6855=LINE('',#42350,#9343);
#6856=LINE('',#42353,#9344);
#6857=LINE('',#42355,#9345);
#6858=LINE('',#42357,#9346);
#6859=LINE('',#42359,#9347);
#6860=LINE('',#42361,#9348);
#6861=LINE('',#42362,#9349);
#6862=LINE('',#42365,#9350);
#6863=LINE('',#42367,#9351);
#6864=LINE('',#42368,#9352);
#6865=LINE('',#42371,#9353);
#6866=LINE('',#42373,#9354);
#6867=LINE('',#42374,#9355);
#6868=LINE('',#42377,#9356);
#6869=LINE('',#42378,#9357);
#6870=LINE('',#42381,#9358);
#6871=LINE('',#42382,#9359);
#6872=LINE('',#42385,#9360);
#6873=LINE('',#42387,#9361);
#6874=LINE('',#42389,#9362);
#6875=LINE('',#42391,#9363);
#6876=LINE('',#42393,#9364);
#6877=LINE('',#42395,#9365);
#6878=LINE('',#42397,#9366);
#6879=LINE('',#42398,#9367);
#6880=LINE('',#42401,#9368);
#6881=LINE('',#42403,#9369);
#6882=LINE('',#42404,#9370);
#6883=LINE('',#42407,#9371);
#6884=LINE('',#42408,#9372);
#6885=LINE('',#42412,#9373);
#6886=LINE('',#42413,#9374);
#6887=LINE('',#42415,#9375);
#6888=LINE('',#42416,#9376);
#6889=LINE('',#42420,#9377);
#6890=LINE('',#42421,#9378);
#6891=LINE('',#42422,#9379);
#6892=LINE('',#42425,#9380);
#6893=LINE('',#42426,#9381);
#6894=LINE('',#42429,#9382);
#6895=LINE('',#42431,#9383);
#6896=LINE('',#42433,#9384);
#6897=LINE('',#42434,#9385);
#6898=LINE('',#42436,#9386);
#6899=LINE('',#42437,#9387);
#6900=LINE('',#42440,#9388);
#6901=LINE('',#42442,#9389);
#6902=LINE('',#42444,#9390);
#6903=LINE('',#42446,#9391);
#6904=LINE('',#42448,#9392);
#6905=LINE('',#42450,#9393);
#6906=LINE('',#42452,#9394);
#6907=LINE('',#42454,#9395);
#6908=LINE('',#42456,#9396);
#6909=LINE('',#42458,#9397);
#6910=LINE('',#42460,#9398);
#6911=LINE('',#42461,#9399);
#6912=LINE('',#42465,#9400);
#6913=LINE('',#42467,#9401);
#6914=LINE('',#42468,#9402);
#6915=LINE('',#42469,#9403);
#6916=LINE('',#42472,#9404);
#6917=LINE('',#42474,#9405);
#6918=LINE('',#42476,#9406);
#6919=LINE('',#42478,#9407);
#6920=LINE('',#42479,#9408);
#6921=LINE('',#42482,#9409);
#6922=LINE('',#42484,#9410);
#6923=LINE('',#42485,#9411);
#6924=LINE('',#42488,#9412);
#6925=LINE('',#42490,#9413);
#6926=LINE('',#42492,#9414);
#6927=LINE('',#42493,#9415);
#6928=LINE('',#42496,#9416);
#6929=LINE('',#42498,#9417);
#6930=LINE('',#42499,#9418);
#6931=LINE('',#42502,#9419);
#6932=LINE('',#42504,#9420);
#6933=LINE('',#42505,#9421);
#6934=LINE('',#42508,#9422);
#6935=LINE('',#42510,#9423);
#6936=LINE('',#42512,#9424);
#6937=LINE('',#42513,#9425);
#6938=LINE('',#42517,#9426);
#6939=LINE('',#42518,#9427);
#6940=LINE('',#42519,#9428);
#6941=LINE('',#42522,#9429);
#6942=LINE('',#42523,#9430);
#6943=LINE('',#42525,#9431);
#6944=LINE('',#42527,#9432);
#6945=LINE('',#42529,#9433);
#6946=LINE('',#42531,#9434);
#6947=LINE('',#42532,#9435);
#6948=LINE('',#42535,#9436);
#6949=LINE('',#42536,#9437);
#6950=LINE('',#42538,#9438);
#6951=LINE('',#42539,#9439);
#6952=LINE('',#42542,#9440);
#6953=LINE('',#42544,#9441);
#6954=LINE('',#42545,#9442);
#6955=LINE('',#42548,#9443);
#6956=LINE('',#42549,#9444);
#6957=LINE('',#42551,#9445);
#6958=LINE('',#42553,#9446);
#6959=LINE('',#42556,#9447);
#6960=LINE('',#42557,#9448);
#6961=LINE('',#42561,#9449);
#6962=LINE('',#42562,#9450);
#6963=LINE('',#42565,#9451);
#6964=LINE('',#42566,#9452);
#6965=LINE('',#42569,#9453);
#6966=LINE('',#42571,#9454);
#6967=LINE('',#42573,#9455);
#6968=LINE('',#42575,#9456);
#6969=LINE('',#42576,#9457);
#6970=LINE('',#42578,#9458);
#6971=LINE('',#42579,#9459);
#6972=LINE('',#42581,#9460);
#6973=LINE('',#42582,#9461);
#6974=LINE('',#42584,#9462);
#6975=LINE('',#42586,#9463);
#6976=LINE('',#42587,#9464);
#6977=LINE('',#42591,#9465);
#6978=LINE('',#42592,#9466);
#6979=LINE('',#42595,#9467);
#6980=LINE('',#42597,#9468);
#6981=LINE('',#42598,#9469);
#6982=LINE('',#42601,#9470);
#6983=LINE('',#42603,#9471);
#6984=LINE('',#42605,#9472);
#6985=LINE('',#42607,#9473);
#6986=LINE('',#42608,#9474);
#6987=LINE('',#42609,#9475);
#6988=LINE('',#42612,#9476);
#6989=LINE('',#42614,#9477);
#6990=LINE('',#42615,#9478);
#6991=LINE('',#42618,#9479);
#6992=LINE('',#42619,#9480);
#6993=LINE('',#42627,#9481);
#6994=LINE('',#42629,#9482);
#6995=LINE('',#42631,#9483);
#6996=LINE('',#42633,#9484);
#6997=LINE('',#42634,#9485);
#6998=LINE('',#42636,#9486);
#6999=LINE('',#42638,#9487);
#7000=LINE('',#42639,#9488);
#7001=LINE('',#42640,#9489);
#7002=LINE('',#42642,#9490);
#7003=LINE('',#42644,#9491);
#7004=LINE('',#42645,#9492);
#7005=LINE('',#42646,#9493);
#7006=LINE('',#42649,#9494);
#7007=LINE('',#42651,#9495);
#7008=LINE('',#42652,#9496);
#7009=LINE('',#42654,#9497);
#7010=LINE('',#42655,#9498);
#7011=LINE('',#42659,#9499);
#7012=LINE('',#42661,#9500);
#7013=LINE('',#42662,#9501);
#7014=LINE('',#42666,#9502);
#7015=LINE('',#42667,#9503);
#7016=LINE('',#42670,#9504);
#7017=LINE('',#42672,#9505);
#7018=LINE('',#42673,#9506);
#7019=LINE('',#42675,#9507);
#7020=LINE('',#42678,#9508);
#7021=LINE('',#42679,#9509);
#7022=LINE('',#42682,#9510);
#7023=LINE('',#42684,#9511);
#7024=LINE('',#42685,#9512);
#7025=LINE('',#42688,#9513);
#7026=LINE('',#42689,#9514);
#7027=LINE('',#42691,#9515);
#7028=LINE('',#42694,#9516);
#7029=LINE('',#42695,#9517);
#7030=LINE('',#42697,#9518);
#7031=LINE('',#42700,#9519);
#7032=LINE('',#42701,#9520);
#7033=LINE('',#42704,#9521);
#7034=LINE('',#42706,#9522);
#7035=LINE('',#42707,#9523);
#7036=LINE('',#42709,#9524);
#7037=LINE('',#42711,#9525);
#7038=LINE('',#42713,#9526);
#7039=LINE('',#42714,#9527);
#7040=LINE('',#42717,#9528);
#7041=LINE('',#42719,#9529);
#7042=LINE('',#42721,#9530);
#7043=LINE('',#42722,#9531);
#7044=LINE('',#42725,#9532);
#7045=LINE('',#42726,#9533);
#7046=LINE('',#42729,#9534);
#7047=LINE('',#42730,#9535);
#7048=LINE('',#42733,#9536);
#7049=LINE('',#42735,#9537);
#7050=LINE('',#42736,#9538);
#7051=LINE('',#42738,#9539);
#7052=LINE('',#42740,#9540);
#7053=LINE('',#42748,#9541);
#7054=LINE('',#42754,#9542);
#7055=LINE('',#42761,#9543);
#7056=LINE('',#42764,#9544);
#7057=LINE('',#42769,#9545);
#7058=LINE('',#42773,#9546);
#7059=LINE('',#42778,#9547);
#7060=LINE('',#42784,#9548);
#7061=LINE('',#42788,#9549);
#7062=LINE('',#42791,#9550);
#7063=LINE('',#42795,#9551);
#7064=LINE('',#42801,#9552);
#7065=LINE('',#42807,#9553);
#7066=LINE('',#42809,#9554);
#7067=LINE('',#42811,#9555);
#7068=LINE('',#42812,#9556);
#7069=LINE('',#42815,#9557);
#7070=LINE('',#42817,#9558);
#7071=LINE('',#42818,#9559);
#7072=LINE('',#42822,#9560);
#7073=LINE('',#42824,#9561);
#7074=LINE('',#42826,#9562);
#7075=LINE('',#42828,#9563);
#7076=LINE('',#42830,#9564);
#7077=LINE('',#42831,#9565);
#7078=LINE('',#42834,#9566);
#7079=LINE('',#42836,#9567);
#7080=LINE('',#42837,#9568);
#7081=LINE('',#42840,#9569);
#7082=LINE('',#42842,#9570);
#7083=LINE('',#42844,#9571);
#7084=LINE('',#42845,#9572);
#7085=LINE('',#42848,#9573);
#7086=LINE('',#42850,#9574);
#7087=LINE('',#42852,#9575);
#7088=LINE('',#42853,#9576);
#7089=LINE('',#42857,#9577);
#7090=LINE('',#42859,#9578);
#7091=LINE('',#42861,#9579);
#7092=LINE('',#42862,#9580);
#7093=LINE('',#42864,#9581);
#7094=LINE('',#42865,#9582);
#7095=LINE('',#42869,#9583);
#7096=LINE('',#42871,#9584);
#7097=LINE('',#42873,#9585);
#7098=LINE('',#42874,#9586);
#7099=LINE('',#42877,#9587);
#7100=LINE('',#42879,#9588);
#7101=LINE('',#42880,#9589);
#7102=LINE('',#42884,#9590);
#7103=LINE('',#42886,#9591);
#7104=LINE('',#42888,#9592);
#7105=LINE('',#42890,#9593);
#7106=LINE('',#42892,#9594);
#7107=LINE('',#42893,#9595);
#7108=LINE('',#42896,#9596);
#7109=LINE('',#42898,#9597);
#7110=LINE('',#42900,#9598);
#7111=LINE('',#42902,#9599);
#7112=LINE('',#42903,#9600);
#7113=LINE('',#42906,#9601);
#7114=LINE('',#42907,#9602);
#7115=LINE('',#42910,#9603);
#7116=LINE('',#42912,#9604);
#7117=LINE('',#42914,#9605);
#7118=LINE('',#42915,#9606);
#7119=LINE('',#42918,#9607);
#7120=LINE('',#42920,#9608);
#7121=LINE('',#42921,#9609);
#7122=LINE('',#42924,#9610);
#7123=LINE('',#42926,#9611);
#7124=LINE('',#42927,#9612);
#7125=LINE('',#42930,#9613);
#7126=LINE('',#42931,#9614);
#7127=LINE('',#42934,#9615);
#7128=LINE('',#42936,#9616);
#7129=LINE('',#42937,#9617);
#7130=LINE('',#42940,#9618);
#7131=LINE('',#42942,#9619);
#7132=LINE('',#42943,#9620);
#7133=LINE('',#42946,#9621);
#7134=LINE('',#42948,#9622);
#7135=LINE('',#42949,#9623);
#7136=LINE('',#42952,#9624);
#7137=LINE('',#42953,#9625);
#7138=LINE('',#42956,#9626);
#7139=LINE('',#42957,#9627);
#7140=LINE('',#42961,#9628);
#7141=LINE('',#42963,#9629);
#7142=LINE('',#42965,#9630);
#7143=LINE('',#42966,#9631);
#7144=LINE('',#42968,#9632);
#7145=LINE('',#42969,#9633);
#7146=LINE('',#42972,#9634);
#7147=LINE('',#42973,#9635);
#7148=LINE('',#42976,#9636);
#7149=LINE('',#42977,#9637);
#7150=LINE('',#42981,#9638);
#7151=LINE('',#42983,#9639);
#7152=LINE('',#42984,#9640);
#7153=LINE('',#42986,#9641);
#7154=LINE('',#42988,#9642);
#7155=LINE('',#42989,#9643);
#7156=LINE('',#42992,#9644);
#7157=LINE('',#42993,#9645);
#7158=LINE('',#42994,#9646);
#7159=LINE('',#42996,#9647);
#7160=LINE('',#42998,#9648);
#7161=LINE('',#42999,#9649);
#7162=LINE('',#43002,#9650);
#7163=LINE('',#43003,#9651);
#7164=LINE('',#43005,#9652);
#7165=LINE('',#43006,#9653);
#7166=LINE('',#43009,#9654);
#7167=LINE('',#43010,#9655);
#7168=LINE('',#43011,#9656);
#7169=LINE('',#43014,#9657);
#7170=LINE('',#43016,#9658);
#7171=LINE('',#43018,#9659);
#7172=LINE('',#43020,#9660);
#7173=LINE('',#43022,#9661);
#7174=LINE('',#43024,#9662);
#7175=LINE('',#43026,#9663);
#7176=LINE('',#43028,#9664);
#7177=LINE('',#43030,#9665);
#7178=LINE('',#43032,#9666);
#7179=LINE('',#43034,#9667);
#7180=LINE('',#43035,#9668);
#7181=LINE('',#43038,#9669);
#7182=LINE('',#43040,#9670);
#7183=LINE('',#43042,#9671);
#7184=LINE('',#43043,#9672);
#7185=LINE('',#43046,#9673);
#7186=LINE('',#43047,#9674);
#7187=LINE('',#43048,#9675);
#7188=LINE('',#43051,#9676);
#7189=LINE('',#43052,#9677);
#7190=LINE('',#43055,#9678);
#7191=LINE('',#43056,#9679);
#7192=LINE('',#43059,#9680);
#7193=LINE('',#43060,#9681);
#7194=LINE('',#43064,#9682);
#7195=LINE('',#43066,#9683);
#7196=LINE('',#43067,#9684);
#7197=LINE('',#43068,#9685);
#7198=LINE('',#43071,#9686);
#7199=LINE('',#43072,#9687);
#7200=LINE('',#43075,#9688);
#7201=LINE('',#43077,#9689);
#7202=LINE('',#43078,#9690);
#7203=LINE('',#43082,#9691);
#7204=LINE('',#43083,#9692);
#7205=LINE('',#43085,#9693);
#7206=LINE('',#43086,#9694);
#7207=LINE('',#43088,#9695);
#7208=LINE('',#43092,#9696);
#7209=LINE('',#43093,#9697);
#7210=LINE('',#43094,#9698);
#7211=LINE('',#43096,#9699);
#7212=LINE('',#43097,#9700);
#7213=LINE('',#43100,#9701);
#7214=LINE('',#43101,#9702);
#7215=LINE('',#43102,#9703);
#7216=LINE('',#43105,#9704);
#7217=LINE('',#43107,#9705);
#7218=LINE('',#43108,#9706);
#7219=LINE('',#43111,#9707);
#7220=LINE('',#43113,#9708);
#7221=LINE('',#43115,#9709);
#7222=LINE('',#43116,#9710);
#7223=LINE('',#43118,#9711);
#7224=LINE('',#43121,#9712);
#7225=LINE('',#43125,#9713);
#7226=LINE('',#43129,#9714);
#7227=LINE('',#43131,#9715);
#7228=LINE('',#43132,#9716);
#7229=LINE('',#43135,#9717);
#7230=LINE('',#43137,#9718);
#7231=LINE('',#43139,#9719);
#7232=LINE('',#43140,#9720);
#7233=LINE('',#43144,#9721);
#7234=LINE('',#43146,#9722);
#7235=LINE('',#43147,#9723);
#7236=LINE('',#43149,#9724);
#7237=LINE('',#43150,#9725);
#7238=LINE('',#43153,#9726);
#7239=LINE('',#43155,#9727);
#7240=LINE('',#43156,#9728);
#7241=LINE('',#43158,#9729);
#7242=LINE('',#43159,#9730);
#7243=LINE('',#43162,#9731);
#7244=LINE('',#43166,#9732);
#7245=LINE('',#43169,#9733);
#7246=LINE('',#43171,#9734);
#7247=LINE('',#43174,#9735);
#7248=LINE('',#43175,#9736);
#7249=LINE('',#43177,#9737);
#7250=LINE('',#43180,#9738);
#7251=LINE('',#43182,#9739);
#7252=LINE('',#43184,#9740);
#7253=LINE('',#43186,#9741);
#7254=LINE('',#43188,#9742);
#7255=LINE('',#43190,#9743);
#7256=LINE('',#43191,#9744);
#7257=LINE('',#43192,#9745);
#7258=LINE('',#43194,#9746);
#7259=LINE('',#43199,#9747);
#7260=LINE('',#43200,#9748);
#7261=LINE('',#43201,#9749);
#7262=LINE('',#43204,#9750);
#7263=LINE('',#43205,#9751);
#7264=LINE('',#43209,#9752);
#7265=LINE('',#43210,#9753);
#7266=LINE('',#43211,#9754);
#7267=LINE('',#43213,#9755);
#7268=LINE('',#43215,#9756);
#7269=LINE('',#43216,#9757);
#7270=LINE('',#43218,#9758);
#7271=LINE('',#43221,#9759);
#7272=LINE('',#43223,#9760);
#7273=LINE('',#43224,#9761);
#7274=LINE('',#43226,#9762);
#7275=LINE('',#43230,#9763);
#7276=LINE('',#43232,#9764);
#7277=LINE('',#43234,#9765);
#7278=LINE('',#43235,#9766);
#7279=LINE('',#43237,#9767);
#7280=LINE('',#43238,#9768);
#7281=LINE('',#43242,#9769);
#7282=LINE('',#43243,#9770);
#7283=LINE('',#43246,#9771);
#7284=LINE('',#43247,#9772);
#7285=LINE('',#43250,#9773);
#7286=LINE('',#43254,#9774);
#7287=LINE('',#43258,#9775);
#7288=LINE('',#43260,#9776);
#7289=LINE('',#43261,#9777);
#7290=LINE('',#43263,#9778);
#7291=LINE('',#43266,#9779);
#7292=LINE('',#43267,#9780);
#7293=LINE('',#43269,#9781);
#7294=LINE('',#43270,#9782);
#7295=LINE('',#43274,#9783);
#7296=LINE('',#43278,#9784);
#7297=LINE('',#43282,#9785);
#7298=LINE('',#43284,#9786);
#7299=LINE('',#43285,#9787);
#7300=LINE('',#43288,#9788);
#7301=LINE('',#43292,#9789);
#7302=LINE('',#43293,#9790);
#7303=LINE('',#43298,#9791);
#7304=LINE('',#43301,#9792);
#7305=LINE('',#43304,#9793);
#7306=LINE('',#43305,#9794);
#7307=LINE('',#43307,#9795);
#7308=LINE('',#43308,#9796);
#7309=LINE('',#43311,#9797);
#7310=LINE('',#43314,#9798);
#7311=LINE('',#43315,#9799);
#7312=LINE('',#43318,#9800);
#7313=LINE('',#43321,#9801);
#7314=LINE('',#43323,#9802);
#7315=LINE('',#43324,#9803);
#7316=LINE('',#43327,#9804);
#7317=LINE('',#43331,#9805);
#7318=LINE('',#43332,#9806);
#7319=LINE('',#43337,#9807);
#7320=LINE('',#43340,#9808);
#7321=LINE('',#43343,#9809);
#7322=LINE('',#43344,#9810);
#7323=LINE('',#43346,#9811);
#7324=LINE('',#43347,#9812);
#7325=LINE('',#43350,#9813);
#7326=LINE('',#43353,#9814);
#7327=LINE('',#43354,#9815);
#7328=LINE('',#43357,#9816);
#7329=LINE('',#43368,#9817);
#7330=LINE('',#43370,#9818);
#7331=LINE('',#43372,#9819);
#7332=LINE('',#43374,#9820);
#7333=LINE('',#43376,#9821);
#7334=LINE('',#43377,#9822);
#7335=LINE('',#43380,#9823);
#7336=LINE('',#43382,#9824);
#7337=LINE('',#43384,#9825);
#7338=LINE('',#43386,#9826);
#7339=LINE('',#43387,#9827);
#7340=LINE('',#43390,#9828);
#7341=LINE('',#43391,#9829);
#7342=LINE('',#43394,#9830);
#7343=LINE('',#43396,#9831);
#7344=LINE('',#43398,#9832);
#7345=LINE('',#43399,#9833);
#7346=LINE('',#43402,#9834);
#7347=LINE('',#43404,#9835);
#7348=LINE('',#43405,#9836);
#7349=LINE('',#43409,#9837);
#7350=LINE('',#43411,#9838);
#7351=LINE('',#43413,#9839);
#7352=LINE('',#43415,#9840);
#7353=LINE('',#43417,#9841);
#7354=LINE('',#43418,#9842);
#7355=LINE('',#43421,#9843);
#7356=LINE('',#43423,#9844);
#7357=LINE('',#43425,#9845);
#7358=LINE('',#43427,#9846);
#7359=LINE('',#43428,#9847);
#7360=LINE('',#43431,#9848);
#7361=LINE('',#43433,#9849);
#7362=LINE('',#43434,#9850);
#7363=LINE('',#43437,#9851);
#7364=LINE('',#43438,#9852);
#7365=LINE('',#43446,#9853);
#7366=LINE('',#43448,#9854);
#7367=LINE('',#43450,#9855);
#7368=LINE('',#43452,#9856);
#7369=LINE('',#43454,#9857);
#7370=LINE('',#43455,#9858);
#7371=LINE('',#43458,#9859);
#7372=LINE('',#43459,#9860);
#7373=LINE('',#43461,#9861);
#7374=LINE('',#43462,#9862);
#7375=LINE('',#43465,#9863);
#7376=LINE('',#43466,#9864);
#7377=LINE('',#43473,#9865);
#7378=LINE('',#43475,#9866);
#7379=LINE('',#43477,#9867);
#7380=LINE('',#43478,#9868);
#7381=LINE('',#43481,#9869);
#7382=LINE('',#43482,#9870);
#7383=LINE('',#43484,#9871);
#7384=LINE('',#43486,#9872);
#7385=LINE('',#43487,#9873);
#7386=LINE('',#43490,#9874);
#7387=LINE('',#43495,#9875);
#7388=LINE('',#43497,#9876);
#7389=LINE('',#43500,#9877);
#7390=LINE('',#43505,#9878);
#7391=LINE('',#43507,#9879);
#7392=LINE('',#43510,#9880);
#7393=LINE('',#43511,#9881);
#7394=LINE('',#43513,#9882);
#7395=LINE('',#43514,#9883);
#7396=LINE('',#43516,#9884);
#7397=LINE('',#43517,#9885);
#7398=LINE('',#43521,#9886);
#7399=LINE('',#43522,#9887);
#7400=LINE('',#43524,#9888);
#7401=LINE('',#43525,#9889);
#7402=LINE('',#43533,#9890);
#7403=LINE('',#43537,#9891);
#7404=LINE('',#43542,#9892);
#7405=LINE('',#43543,#9893);
#7406=LINE('',#43544,#9894);
#7407=LINE('',#43548,#9895);
#7408=LINE('',#43554,#9896);
#7409=LINE('',#43555,#9897);
#7410=LINE('',#43556,#9898);
#7411=LINE('',#43560,#9899);
#7412=LINE('',#43566,#9900);
#7413=LINE('',#43567,#9901);
#7414=LINE('',#43568,#9902);
#7415=LINE('',#43572,#9903);
#7416=LINE('',#43576,#9904);
#7417=LINE('',#43577,#9905);
#7418=LINE('',#43580,#9906);
#7419=LINE('',#43582,#9907);
#7420=LINE('',#43583,#9908);
#7421=LINE('',#43586,#9909);
#7422=LINE('',#43590,#9910);
#7423=LINE('',#43591,#9911);
#7424=LINE('',#43594,#9912);
#7425=LINE('',#43606,#9913);
#7426=LINE('',#43608,#9914);
#7427=LINE('',#43610,#9915);
#7428=LINE('',#43611,#9916);
#7429=LINE('',#43616,#9917);
#7430=LINE('',#43620,#9918);
#7431=LINE('',#43622,#9919);
#7432=LINE('',#43623,#9920);
#7433=LINE('',#43626,#9921);
#7434=LINE('',#43628,#9922);
#7435=LINE('',#43629,#9923);
#7436=LINE('',#43632,#9924);
#7437=LINE('',#43636,#9925);
#7438=LINE('',#43637,#9926);
#7439=LINE('',#43641,#9927);
#7440=LINE('',#43647,#9928);
#7441=LINE('',#43648,#9929);
#7442=LINE('',#43649,#9930);
#7443=LINE('',#43653,#9931);
#7444=LINE('',#43658,#9932);
#7445=LINE('',#43659,#9933);
#7446=LINE('',#43660,#9934);
#7447=LINE('',#43665,#9935);
#7448=LINE('',#43668,#9936);
#7449=LINE('',#43671,#9937);
#7450=LINE('',#43672,#9938);
#7451=LINE('',#43675,#9939);
#7452=LINE('',#43679,#9940);
#7453=LINE('',#43680,#9941);
#7454=LINE('',#43684,#9942);
#7455=LINE('',#43685,#9943);
#7456=LINE('',#43690,#9944);
#7457=LINE('',#43692,#9945);
#7458=LINE('',#43694,#9946);
#7459=LINE('',#43695,#9947);
#7460=LINE('',#43699,#9948);
#7461=LINE('',#43705,#9949);
#7462=LINE('',#43706,#9950);
#7463=LINE('',#43707,#9951);
#7464=LINE('',#43711,#9952);
#7465=LINE('',#43717,#9953);
#7466=LINE('',#43718,#9954);
#7467=LINE('',#43719,#9955);
#7468=LINE('',#43722,#9956);
#7469=LINE('',#43725,#9957);
#7470=LINE('',#43728,#9958);
#7471=LINE('',#43729,#9959);
#7472=LINE('',#43733,#9960);
#7473=LINE('',#43735,#9961);
#7474=LINE('',#43737,#9962);
#7475=LINE('',#43738,#9963);
#7476=LINE('',#43742,#9964);
#7477=LINE('',#43748,#9965);
#7478=LINE('',#43749,#9966);
#7479=LINE('',#43750,#9967);
#7480=LINE('',#43754,#9968);
#7481=LINE('',#43760,#9969);
#7482=LINE('',#43761,#9970);
#7483=LINE('',#43762,#9971);
#7484=LINE('',#43764,#9972);
#7485=LINE('',#43770,#9973);
#7486=LINE('',#43772,#9974);
#7487=LINE('',#43774,#9975);
#7488=LINE('',#43775,#9976);
#7489=LINE('',#43779,#9977);
#7490=LINE('',#43785,#9978);
#7491=LINE('',#43786,#9979);
#7492=LINE('',#43787,#9980);
#7493=LINE('',#43791,#9981);
#7494=LINE('',#43797,#9982);
#7495=LINE('',#43798,#9983);
#7496=LINE('',#43799,#9984);
#7497=LINE('',#43801,#9985);
#7498=LINE('',#43807,#9986);
#7499=LINE('',#43809,#9987);
#7500=LINE('',#43811,#9988);
#7501=LINE('',#43812,#9989);
#7502=LINE('',#43816,#9990);
#7503=LINE('',#43822,#9991);
#7504=LINE('',#43823,#9992);
#7505=LINE('',#43824,#9993);
#7506=LINE('',#43828,#9994);
#7507=LINE('',#43834,#9995);
#7508=LINE('',#43835,#9996);
#7509=LINE('',#43836,#9997);
#7510=LINE('',#43839,#9998);
#7511=LINE('',#43840,#9999);
#7512=LINE('',#43841,#10000);
#7513=LINE('',#43843,#10001);
#7514=LINE('',#43845,#10002);
#7515=LINE('',#43847,#10003);
#7516=LINE('',#43850,#10004);
#7517=LINE('',#43851,#10005);
#7518=LINE('',#43854,#10006);
#7519=LINE('',#43860,#10007);
#7520=LINE('',#43866,#10008);
#7521=LINE('',#43869,#10009);
#7522=LINE('',#43874,#10010);
#7523=LINE('',#43877,#10011);
#7524=LINE('',#43881,#10012);
#7525=LINE('',#43885,#10013);
#7526=LINE('',#43888,#10014);
#7527=LINE('',#43890,#10015);
#7528=LINE('',#43892,#10016);
#7529=LINE('',#43893,#10017);
#7530=LINE('',#43895,#10018);
#7531=LINE('',#43897,#10019);
#7532=LINE('',#43900,#10020);
#7533=LINE('',#43903,#10021);
#7534=LINE('',#43905,#10022);
#7535=LINE('',#43911,#10023);
#7536=LINE('',#43913,#10024);
#7537=LINE('',#43923,#10025);
#7538=LINE('',#43926,#10026);
#7539=LINE('',#43931,#10027);
#7540=LINE('',#43936,#10028);
#7541=LINE('',#43954,#10029);
#7542=LINE('',#43961,#10030);
#7543=LINE('',#43965,#10031);
#7544=LINE('',#43967,#10032);
#7545=LINE('',#43970,#10033);
#7546=LINE('',#43972,#10034);
#7547=LINE('',#43973,#10035);
#7548=LINE('',#43976,#10036);
#7549=LINE('',#43981,#10037);
#7550=LINE('',#43982,#10038);
#7551=LINE('',#43983,#10039);
#7552=LINE('',#43987,#10040);
#7553=LINE('',#43993,#10041);
#7554=LINE('',#43994,#10042);
#7555=LINE('',#43995,#10043);
#7556=LINE('',#43998,#10044);
#7557=LINE('',#44003,#10045);
#7558=LINE('',#44004,#10046);
#7559=LINE('',#44008,#10047);
#7560=LINE('',#44011,#10048);
#7561=LINE('',#44014,#10049);
#7562=LINE('',#44016,#10050);
#7563=LINE('',#44022,#10051);
#7564=LINE('',#44055,#10052);
#7565=LINE('',#44145,#10053);
#7566=LINE('',#44235,#10054);
#7567=LINE('',#44325,#10055);
#7568=LINE('',#44414,#10056);
#7569=LINE('',#44442,#10057);
#7570=LINE('',#44480,#10058);
#7571=LINE('',#44518,#10059);
#7572=LINE('',#44556,#10060);
#7573=LINE('',#44558,#10061);
#7574=LINE('',#44560,#10062);
#7575=LINE('',#44570,#10063);
#7576=LINE('',#44571,#10064);
#7577=LINE('',#44577,#10065);
#7578=LINE('',#44579,#10066);
#7579=LINE('',#44581,#10067);
#7580=LINE('',#44591,#10068);
#7581=LINE('',#44592,#10069);
#7582=LINE('',#44598,#10070);
#7583=LINE('',#44600,#10071);
#7584=LINE('',#44602,#10072);
#7585=LINE('',#44612,#10073);
#7586=LINE('',#44613,#10074);
#7587=LINE('',#44619,#10075);
#7588=LINE('',#44621,#10076);
#7589=LINE('',#44623,#10077);
#7590=LINE('',#44633,#10078);
#7591=LINE('',#44634,#10079);
#7592=LINE('',#44640,#10080);
#7593=LINE('',#44642,#10081);
#7594=LINE('',#44644,#10082);
#7595=LINE('',#44654,#10083);
#7596=LINE('',#44655,#10084);
#7597=LINE('',#44661,#10085);
#7598=LINE('',#44663,#10086);
#7599=LINE('',#44665,#10087);
#7600=LINE('',#44675,#10088);
#7601=LINE('',#44676,#10089);
#7602=LINE('',#44684,#10090);
#7603=LINE('',#44686,#10091);
#7604=LINE('',#44688,#10092);
#7605=LINE('',#44698,#10093);
#7606=LINE('',#44699,#10094);
#7607=LINE('',#44705,#10095);
#7608=LINE('',#44707,#10096);
#7609=LINE('',#44709,#10097);
#7610=LINE('',#44719,#10098);
#7611=LINE('',#44720,#10099);
#7612=LINE('',#44726,#10100);
#7613=LINE('',#44728,#10101);
#7614=LINE('',#44730,#10102);
#7615=LINE('',#44740,#10103);
#7616=LINE('',#44741,#10104);
#7617=LINE('',#44747,#10105);
#7618=LINE('',#44749,#10106);
#7619=LINE('',#44751,#10107);
#7620=LINE('',#44761,#10108);
#7621=LINE('',#44762,#10109);
#7622=LINE('',#44768,#10110);
#7623=LINE('',#44770,#10111);
#7624=LINE('',#44772,#10112);
#7625=LINE('',#44782,#10113);
#7626=LINE('',#44783,#10114);
#7627=LINE('',#44789,#10115);
#7628=LINE('',#44791,#10116);
#7629=LINE('',#44793,#10117);
#7630=LINE('',#44803,#10118);
#7631=LINE('',#44804,#10119);
#7632=LINE('',#44810,#10120);
#7633=LINE('',#44812,#10121);
#7634=LINE('',#44814,#10122);
#7635=LINE('',#44824,#10123);
#7636=LINE('',#44825,#10124);
#7637=LINE('',#44831,#10125);
#7638=LINE('',#44833,#10126);
#7639=LINE('',#44835,#10127);
#7640=LINE('',#44845,#10128);
#7641=LINE('',#44846,#10129);
#7642=LINE('',#44852,#10130);
#7643=LINE('',#44854,#10131);
#7644=LINE('',#44856,#10132);
#7645=LINE('',#44866,#10133);
#7646=LINE('',#44867,#10134);
#7647=LINE('',#44873,#10135);
#7648=LINE('',#44875,#10136);
#7649=LINE('',#44877,#10137);
#7650=LINE('',#44887,#10138);
#7651=LINE('',#44888,#10139);
#7652=LINE('',#44894,#10140);
#7653=LINE('',#44896,#10141);
#7654=LINE('',#44898,#10142);
#7655=LINE('',#44908,#10143);
#7656=LINE('',#44909,#10144);
#7657=LINE('',#44915,#10145);
#7658=LINE('',#44917,#10146);
#7659=LINE('',#44919,#10147);
#7660=LINE('',#44929,#10148);
#7661=LINE('',#44930,#10149);
#7662=LINE('',#44936,#10150);
#7663=LINE('',#44938,#10151);
#7664=LINE('',#44940,#10152);
#7665=LINE('',#44950,#10153);
#7666=LINE('',#44951,#10154);
#7667=LINE('',#44957,#10155);
#7668=LINE('',#44959,#10156);
#7669=LINE('',#44961,#10157);
#7670=LINE('',#44971,#10158);
#7671=LINE('',#44972,#10159);
#7672=LINE('',#44978,#10160);
#7673=LINE('',#44980,#10161);
#7674=LINE('',#44982,#10162);
#7675=LINE('',#44992,#10163);
#7676=LINE('',#44993,#10164);
#7677=LINE('',#44999,#10165);
#7678=LINE('',#45001,#10166);
#7679=LINE('',#45003,#10167);
#7680=LINE('',#45013,#10168);
#7681=LINE('',#45014,#10169);
#7682=LINE('',#45020,#10170);
#7683=LINE('',#45022,#10171);
#7684=LINE('',#45024,#10172);
#7685=LINE('',#45034,#10173);
#7686=LINE('',#45035,#10174);
#7687=LINE('',#45041,#10175);
#7688=LINE('',#45043,#10176);
#7689=LINE('',#45045,#10177);
#7690=LINE('',#45055,#10178);
#7691=LINE('',#45056,#10179);
#7692=LINE('',#45062,#10180);
#7693=LINE('',#46048,#10181);
#7694=LINE('',#46052,#10182);
#7695=LINE('',#46056,#10183);
#7696=LINE('',#46063,#10184);
#7697=LINE('',#46070,#10185);
#7698=LINE('',#46097,#10186);
#7699=LINE('',#46145,#10187);
#7700=LINE('',#46193,#10188);
#7701=LINE('',#46247,#10189);
#7702=LINE('',#46295,#10190);
#7703=LINE('',#46343,#10191);
#7704=LINE('',#46397,#10192);
#7705=LINE('',#46445,#10193);
#7706=LINE('',#46493,#10194);
#7707=LINE('',#46547,#10195);
#7708=LINE('',#46595,#10196);
#7709=LINE('',#46643,#10197);
#7710=LINE('',#46691,#10198);
#7711=LINE('',#46739,#10199);
#7712=LINE('',#46787,#10200);
#7713=LINE('',#46803,#10201);
#7714=LINE('',#46828,#10202);
#7715=LINE('',#46852,#10203);
#7716=LINE('',#46878,#10204);
#7717=LINE('',#46902,#10205);
#7718=LINE('',#46926,#10206);
#7719=LINE('',#46951,#10207);
#7720=LINE('',#46976,#10208);
#7721=LINE('',#47000,#10209);
#7722=LINE('',#47025,#10210);
#7723=LINE('',#47050,#10211);
#7724=LINE('',#47074,#10212);
#7725=LINE('',#47099,#10213);
#7726=LINE('',#47124,#10214);
#7727=LINE('',#47152,#10215);
#7728=LINE('',#47154,#10216);
#7729=LINE('',#47155,#10217);
#7730=LINE('',#47159,#10218);
#7731=LINE('',#47165,#10219);
#7732=LINE('',#47173,#10220);
#7733=LINE('',#47175,#10221);
#7734=LINE('',#47176,#10222);
#7735=LINE('',#47180,#10223);
#7736=LINE('',#47186,#10224);
#7737=LINE('',#47194,#10225);
#7738=LINE('',#47196,#10226);
#7739=LINE('',#47197,#10227);
#7740=LINE('',#47201,#10228);
#7741=LINE('',#47207,#10229);
#7742=LINE('',#47215,#10230);
#7743=LINE('',#47217,#10231);
#7744=LINE('',#47218,#10232);
#7745=LINE('',#47222,#10233);
#7746=LINE('',#47228,#10234);
#7747=LINE('',#47236,#10235);
#7748=LINE('',#47238,#10236);
#7749=LINE('',#47239,#10237);
#7750=LINE('',#47243,#10238);
#7751=LINE('',#47249,#10239);
#7752=LINE('',#47257,#10240);
#7753=LINE('',#47259,#10241);
#7754=LINE('',#47260,#10242);
#7755=LINE('',#47264,#10243);
#7756=LINE('',#47270,#10244);
#7757=LINE('',#47278,#10245);
#7758=LINE('',#47280,#10246);
#7759=LINE('',#47281,#10247);
#7760=LINE('',#47285,#10248);
#7761=LINE('',#47291,#10249);
#7762=LINE('',#47299,#10250);
#7763=LINE('',#47301,#10251);
#7764=LINE('',#47302,#10252);
#7765=LINE('',#47306,#10253);
#7766=LINE('',#47312,#10254);
#7767=LINE('',#47320,#10255);
#7768=LINE('',#47322,#10256);
#7769=LINE('',#47323,#10257);
#7770=LINE('',#47327,#10258);
#7771=LINE('',#47333,#10259);
#7772=LINE('',#47341,#10260);
#7773=LINE('',#47343,#10261);
#7774=LINE('',#47344,#10262);
#7775=LINE('',#47348,#10263);
#7776=LINE('',#47354,#10264);
#7777=LINE('',#47362,#10265);
#7778=LINE('',#47364,#10266);
#7779=LINE('',#47365,#10267);
#7780=LINE('',#47369,#10268);
#7781=LINE('',#47375,#10269);
#7782=LINE('',#47383,#10270);
#7783=LINE('',#47385,#10271);
#7784=LINE('',#47386,#10272);
#7785=LINE('',#47390,#10273);
#7786=LINE('',#47396,#10274);
#7787=LINE('',#47404,#10275);
#7788=LINE('',#47406,#10276);
#7789=LINE('',#47407,#10277);
#7790=LINE('',#47411,#10278);
#7791=LINE('',#47417,#10279);
#7792=LINE('',#47425,#10280);
#7793=LINE('',#47427,#10281);
#7794=LINE('',#47428,#10282);
#7795=LINE('',#47433,#10283);
#7796=LINE('',#47440,#10284);
#7797=LINE('',#47448,#10285);
#7798=LINE('',#47450,#10286);
#7799=LINE('',#47451,#10287);
#7800=LINE('',#47455,#10288);
#7801=LINE('',#47461,#10289);
#7802=LINE('',#47469,#10290);
#7803=LINE('',#47471,#10291);
#7804=LINE('',#47472,#10292);
#7805=LINE('',#47476,#10293);
#7806=LINE('',#47482,#10294);
#7807=LINE('',#47490,#10295);
#7808=LINE('',#47492,#10296);
#7809=LINE('',#47493,#10297);
#7810=LINE('',#47497,#10298);
#7811=LINE('',#47503,#10299);
#7812=LINE('',#47511,#10300);
#7813=LINE('',#47513,#10301);
#7814=LINE('',#47514,#10302);
#7815=LINE('',#47518,#10303);
#7816=LINE('',#47524,#10304);
#7817=LINE('',#47534,#10305);
#7818=LINE('',#48675,#10306);
#7819=LINE('',#48682,#10307);
#7820=LINE('',#48686,#10308);
#7821=LINE('',#48693,#10309);
#7822=LINE('',#48699,#10310);
#7823=LINE('',#48701,#10311);
#7824=LINE('',#48703,#10312);
#7825=LINE('',#48705,#10313);
#7826=LINE('',#48707,#10314);
#7827=LINE('',#48708,#10315);
#7828=LINE('',#48714,#10316);
#7829=LINE('',#48715,#10317);
#7830=LINE('',#48716,#10318);
#7831=LINE('',#48719,#10319);
#7832=LINE('',#48720,#10320);
#7833=LINE('',#48723,#10321);
#7834=LINE('',#48724,#10322);
#7835=LINE('',#48727,#10323);
#7836=LINE('',#48728,#10324);
#7837=LINE('',#48731,#10325);
#7838=LINE('',#48732,#10326);
#7839=LINE('',#48734,#10327);
#7840=LINE('',#48739,#10328);
#7841=LINE('',#48744,#10329);
#7842=LINE('',#48767,#10330);
#7843=LINE('',#48791,#10331);
#7844=LINE('',#48794,#10332);
#7845=LINE('',#48797,#10333);
#7846=LINE('',#48799,#10334);
#7847=LINE('',#48800,#10335);
#7848=LINE('',#48803,#10336);
#7849=LINE('',#48805,#10337);
#7850=LINE('',#48806,#10338);
#7851=LINE('',#48809,#10339);
#7852=LINE('',#48811,#10340);
#7853=LINE('',#48812,#10341);
#7854=LINE('',#48818,#10342);
#7855=LINE('',#48821,#10343);
#7856=LINE('',#48823,#10344);
#7857=LINE('',#48824,#10345);
#7858=LINE('',#48826,#10346);
#7859=LINE('',#48827,#10347);
#7860=LINE('',#48832,#10348);
#7861=LINE('',#48834,#10349);
#7862=LINE('',#48836,#10350);
#7863=LINE('',#48837,#10351);
#7864=LINE('',#48840,#10352);
#7865=LINE('',#48842,#10353);
#7866=LINE('',#48843,#10354);
#7867=LINE('',#48846,#10355);
#7868=LINE('',#48848,#10356);
#7869=LINE('',#48849,#10357);
#7870=LINE('',#48851,#10358);
#7871=LINE('',#48852,#10359);
#7872=LINE('',#48857,#10360);
#7873=LINE('',#48859,#10361);
#7874=LINE('',#48861,#10362);
#7875=LINE('',#48862,#10363);
#7876=LINE('',#48865,#10364);
#7877=LINE('',#48867,#10365);
#7878=LINE('',#48868,#10366);
#7879=LINE('',#48871,#10367);
#7880=LINE('',#48873,#10368);
#7881=LINE('',#48874,#10369);
#7882=LINE('',#48876,#10370);
#7883=LINE('',#48877,#10371);
#7884=LINE('',#48882,#10372);
#7885=LINE('',#48884,#10373);
#7886=LINE('',#48886,#10374);
#7887=LINE('',#48887,#10375);
#7888=LINE('',#48890,#10376);
#7889=LINE('',#48892,#10377);
#7890=LINE('',#48893,#10378);
#7891=LINE('',#48896,#10379);
#7892=LINE('',#48898,#10380);
#7893=LINE('',#48899,#10381);
#7894=LINE('',#48901,#10382);
#7895=LINE('',#48902,#10383);
#7896=LINE('',#48907,#10384);
#7897=LINE('',#48909,#10385);
#7898=LINE('',#48911,#10386);
#7899=LINE('',#48912,#10387);
#7900=LINE('',#48915,#10388);
#7901=LINE('',#48917,#10389);
#7902=LINE('',#48918,#10390);
#7903=LINE('',#48921,#10391);
#7904=LINE('',#48923,#10392);
#7905=LINE('',#48924,#10393);
#7906=LINE('',#48926,#10394);
#7907=LINE('',#48927,#10395);
#7908=LINE('',#48932,#10396);
#7909=LINE('',#48934,#10397);
#7910=LINE('',#48936,#10398);
#7911=LINE('',#48937,#10399);
#7912=LINE('',#48940,#10400);
#7913=LINE('',#48942,#10401);
#7914=LINE('',#48943,#10402);
#7915=LINE('',#48946,#10403);
#7916=LINE('',#48948,#10404);
#7917=LINE('',#48949,#10405);
#7918=LINE('',#48951,#10406);
#7919=LINE('',#48952,#10407);
#7920=LINE('',#48957,#10408);
#7921=LINE('',#48959,#10409);
#7922=LINE('',#48961,#10410);
#7923=LINE('',#48962,#10411);
#7924=LINE('',#48965,#10412);
#7925=LINE('',#48967,#10413);
#7926=LINE('',#48968,#10414);
#7927=LINE('',#48971,#10415);
#7928=LINE('',#48973,#10416);
#7929=LINE('',#48974,#10417);
#7930=LINE('',#48976,#10418);
#7931=LINE('',#48977,#10419);
#7932=LINE('',#48982,#10420);
#7933=LINE('',#48984,#10421);
#7934=LINE('',#48986,#10422);
#7935=LINE('',#48987,#10423);
#7936=LINE('',#48990,#10424);
#7937=LINE('',#48992,#10425);
#7938=LINE('',#48993,#10426);
#7939=LINE('',#48996,#10427);
#7940=LINE('',#48998,#10428);
#7941=LINE('',#48999,#10429);
#7942=LINE('',#49001,#10430);
#7943=LINE('',#49002,#10431);
#7944=LINE('',#49007,#10432);
#7945=LINE('',#49009,#10433);
#7946=LINE('',#49011,#10434);
#7947=LINE('',#49012,#10435);
#7948=LINE('',#49015,#10436);
#7949=LINE('',#49017,#10437);
#7950=LINE('',#49018,#10438);
#7951=LINE('',#49021,#10439);
#7952=LINE('',#49023,#10440);
#7953=LINE('',#49024,#10441);
#7954=LINE('',#49026,#10442);
#7955=LINE('',#49027,#10443);
#7956=LINE('',#49032,#10444);
#7957=LINE('',#49034,#10445);
#7958=LINE('',#49036,#10446);
#7959=LINE('',#49037,#10447);
#7960=LINE('',#49040,#10448);
#7961=LINE('',#49042,#10449);
#7962=LINE('',#49043,#10450);
#7963=LINE('',#49046,#10451);
#7964=LINE('',#49048,#10452);
#7965=LINE('',#49049,#10453);
#7966=LINE('',#49051,#10454);
#7967=LINE('',#49052,#10455);
#7968=LINE('',#49057,#10456);
#7969=LINE('',#49059,#10457);
#7970=LINE('',#49061,#10458);
#7971=LINE('',#49062,#10459);
#7972=LINE('',#49065,#10460);
#7973=LINE('',#49067,#10461);
#7974=LINE('',#49068,#10462);
#7975=LINE('',#49071,#10463);
#7976=LINE('',#49073,#10464);
#7977=LINE('',#49074,#10465);
#7978=LINE('',#49076,#10466);
#7979=LINE('',#49077,#10467);
#7980=LINE('',#49082,#10468);
#7981=LINE('',#49084,#10469);
#7982=LINE('',#49086,#10470);
#7983=LINE('',#49087,#10471);
#7984=LINE('',#49090,#10472);
#7985=LINE('',#49092,#10473);
#7986=LINE('',#49093,#10474);
#7987=LINE('',#49096,#10475);
#7988=LINE('',#49098,#10476);
#7989=LINE('',#49099,#10477);
#7990=LINE('',#49101,#10478);
#7991=LINE('',#49102,#10479);
#7992=LINE('',#49109,#10480);
#7993=LINE('',#49117,#10481);
#7994=LINE('',#49121,#10482);
#7995=LINE('',#49128,#10483);
#7996=LINE('',#49132,#10484);
#7997=LINE('',#49261,#10485);
#7998=LINE('',#49330,#10486);
#7999=LINE('',#49370,#10487);
#8000=LINE('',#49528,#10488);
#8001=LINE('',#49605,#10489);
#8002=LINE('',#49607,#10490);
#8003=LINE('',#49613,#10491);
#8004=LINE('',#49620,#10492);
#8005=LINE('',#49624,#10493);
#8006=LINE('',#49628,#10494);
#8007=LINE('',#49633,#10495);
#8008=LINE('',#50006,#10496);
#8009=LINE('',#50008,#10497);
#8010=LINE('',#50010,#10498);
#8011=LINE('',#50011,#10499);
#8012=LINE('',#50014,#10500);
#8013=LINE('',#50016,#10501);
#8014=LINE('',#50017,#10502);
#8015=LINE('',#50020,#10503);
#8016=LINE('',#50022,#10504);
#8017=LINE('',#50023,#10505);
#8018=LINE('',#50027,#10506);
#8019=LINE('',#50029,#10507);
#8020=LINE('',#50031,#10508);
#8021=LINE('',#50032,#10509);
#8022=LINE('',#50035,#10510);
#8023=LINE('',#50037,#10511);
#8024=LINE('',#50038,#10512);
#8025=LINE('',#50041,#10513);
#8026=LINE('',#50043,#10514);
#8027=LINE('',#50044,#10515);
#8028=LINE('',#50048,#10516);
#8029=LINE('',#50050,#10517);
#8030=LINE('',#50052,#10518);
#8031=LINE('',#50054,#10519);
#8032=LINE('',#50055,#10520);
#8033=LINE('',#50058,#10521);
#8034=LINE('',#50060,#10522);
#8035=LINE('',#50062,#10523);
#8036=LINE('',#50064,#10524);
#8037=LINE('',#50066,#10525);
#8038=LINE('',#50068,#10526);
#8039=LINE('',#50069,#10527);
#8040=LINE('',#50072,#10528);
#8041=LINE('',#50073,#10529);
#8042=LINE('',#50076,#10530);
#8043=LINE('',#50078,#10531);
#8044=LINE('',#50080,#10532);
#8045=LINE('',#50081,#10533);
#8046=LINE('',#50084,#10534);
#8047=LINE('',#50085,#10535);
#8048=LINE('',#50088,#10536);
#8049=LINE('',#50090,#10537);
#8050=LINE('',#50092,#10538);
#8051=LINE('',#50093,#10539);
#8052=LINE('',#50094,#10540);
#8053=LINE('',#50097,#10541);
#8054=LINE('',#50099,#10542);
#8055=LINE('',#50101,#10543);
#8056=LINE('',#50103,#10544);
#8057=LINE('',#50104,#10545);
#8058=LINE('',#50107,#10546);
#8059=LINE('',#50109,#10547);
#8060=LINE('',#50111,#10548);
#8061=LINE('',#50113,#10549);
#8062=LINE('',#50114,#10550);
#8063=LINE('',#50117,#10551);
#8064=LINE('',#50119,#10552);
#8065=LINE('',#50121,#10553);
#8066=LINE('',#50122,#10554);
#8067=LINE('',#50125,#10555);
#8068=LINE('',#50127,#10556);
#8069=LINE('',#50128,#10557);
#8070=LINE('',#50131,#10558);
#8071=LINE('',#50133,#10559);
#8072=LINE('',#50135,#10560);
#8073=LINE('',#50136,#10561);
#8074=LINE('',#50139,#10562);
#8075=LINE('',#50140,#10563);
#8076=LINE('',#50143,#10564);
#8077=LINE('',#50145,#10565);
#8078=LINE('',#50146,#10566);
#8079=LINE('',#50150,#10567);
#8080=LINE('',#50152,#10568);
#8081=LINE('',#50154,#10569);
#8082=LINE('',#50156,#10570);
#8083=LINE('',#50157,#10571);
#8084=LINE('',#50160,#10572);
#8085=LINE('',#50162,#10573);
#8086=LINE('',#50164,#10574);
#8087=LINE('',#50166,#10575);
#8088=LINE('',#50168,#10576);
#8089=LINE('',#50170,#10577);
#8090=LINE('',#50171,#10578);
#8091=LINE('',#50174,#10579);
#8092=LINE('',#50175,#10580);
#8093=LINE('',#50178,#10581);
#8094=LINE('',#50180,#10582);
#8095=LINE('',#50182,#10583);
#8096=LINE('',#50183,#10584);
#8097=LINE('',#50184,#10585);
#8098=LINE('',#50187,#10586);
#8099=LINE('',#50189,#10587);
#8100=LINE('',#50190,#10588);
#8101=LINE('',#50193,#10589);
#8102=LINE('',#50194,#10590);
#8103=LINE('',#50196,#10591);
#8104=LINE('',#50198,#10592);
#8105=LINE('',#50200,#10593);
#8106=LINE('',#50201,#10594);
#8107=LINE('',#50204,#10595);
#8108=LINE('',#50205,#10596);
#8109=LINE('',#50208,#10597);
#8110=LINE('',#50209,#10598);
#8111=LINE('',#50212,#10599);
#8112=LINE('',#50214,#10600);
#8113=LINE('',#50216,#10601);
#8114=LINE('',#50218,#10602);
#8115=LINE('',#50219,#10603);
#8116=LINE('',#50222,#10604);
#8117=LINE('',#50224,#10605);
#8118=LINE('',#50226,#10606);
#8119=LINE('',#50228,#10607);
#8120=LINE('',#50229,#10608);
#8121=LINE('',#50232,#10609);
#8122=LINE('',#50234,#10610);
#8123=LINE('',#50236,#10611);
#8124=LINE('',#50237,#10612);
#8125=LINE('',#50240,#10613);
#8126=LINE('',#50242,#10614);
#8127=LINE('',#50243,#10615);
#8128=LINE('',#50246,#10616);
#8129=LINE('',#50248,#10617);
#8130=LINE('',#50250,#10618);
#8131=LINE('',#50251,#10619);
#8132=LINE('',#50254,#10620);
#8133=LINE('',#50256,#10621);
#8134=LINE('',#50257,#10622);
#8135=LINE('',#50261,#10623);
#8136=LINE('',#50265,#10624);
#8137=LINE('',#50270,#10625);
#8138=LINE('',#50271,#10626);
#8139=LINE('',#50272,#10627);
#8140=LINE('',#50276,#10628);
#8141=LINE('',#50282,#10629);
#8142=LINE('',#50283,#10630);
#8143=LINE('',#50284,#10631);
#8144=LINE('',#50288,#10632);
#8145=LINE('',#50294,#10633);
#8146=LINE('',#50295,#10634);
#8147=LINE('',#50296,#10635);
#8148=LINE('',#50300,#10636);
#8149=LINE('',#50304,#10637);
#8150=LINE('',#50305,#10638);
#8151=LINE('',#50308,#10639);
#8152=LINE('',#50310,#10640);
#8153=LINE('',#50311,#10641);
#8154=LINE('',#50314,#10642);
#8155=LINE('',#50318,#10643);
#8156=LINE('',#50319,#10644);
#8157=LINE('',#50322,#10645);
#8158=LINE('',#50331,#10646);
#8159=LINE('',#50332,#10647);
#8160=LINE('',#50335,#10648);
#8161=LINE('',#50336,#10649);
#8162=LINE('',#50339,#10650);
#8163=LINE('',#50341,#10651);
#8164=LINE('',#50342,#10652);
#8165=LINE('',#50344,#10653);
#8166=LINE('',#50347,#10654);
#8167=LINE('',#50349,#10655);
#8168=LINE('',#50350,#10656);
#8169=LINE('',#50356,#10657);
#8170=LINE('',#50357,#10658);
#8171=LINE('',#50361,#10659);
#8172=LINE('',#50363,#10660);
#8173=LINE('',#50365,#10661);
#8174=LINE('',#50366,#10662);
#8175=LINE('',#50368,#10663);
#8176=LINE('',#50370,#10664);
#8177=LINE('',#50371,#10665);
#8178=LINE('',#50378,#10666);
#8179=LINE('',#50379,#10667);
#8180=LINE('',#50382,#10668);
#8181=LINE('',#50383,#10669);
#8182=LINE('',#50385,#10670);
#8183=LINE('',#50390,#10671);
#8184=LINE('',#50395,#10672);
#8185=LINE('',#50397,#10673);
#8186=LINE('',#50401,#10674);
#8187=LINE('',#50404,#10675);
#8188=LINE('',#50409,#10676);
#8189=LINE('',#50413,#10677);
#8190=LINE('',#50415,#10678);
#8191=LINE('',#50420,#10679);
#8192=LINE('',#50425,#10680);
#8193=LINE('',#50427,#10681);
#8194=LINE('',#50430,#10682);
#8195=LINE('',#50435,#10683);
#8196=LINE('',#50437,#10684);
#8197=LINE('',#50440,#10685);
#8198=LINE('',#50444,#10686);
#8199=LINE('',#50448,#10687);
#8200=LINE('',#50452,#10688);
#8201=LINE('',#50456,#10689);
#8202=LINE('',#50458,#10690);
#8203=LINE('',#50459,#10691);
#8204=LINE('',#50463,#10692);
#8205=LINE('',#50469,#10693);
#8206=LINE('',#50470,#10694);
#8207=LINE('',#50471,#10695);
#8208=LINE('',#50475,#10696);
#8209=LINE('',#50479,#10697);
#8210=LINE('',#50480,#10698);
#8211=LINE('',#50483,#10699);
#8212=LINE('',#50485,#10700);
#8213=LINE('',#50489,#10701);
#8214=LINE('',#50492,#10702);
#8215=LINE('',#50499,#10703);
#8216=LINE('',#50500,#10704);
#8217=LINE('',#50503,#10705);
#8218=LINE('',#50507,#10706);
#8219=LINE('',#50508,#10707);
#8220=LINE('',#50511,#10708);
#8221=LINE('',#50515,#10709);
#8222=LINE('',#50516,#10710);
#8223=LINE('',#50518,#10711);
#8224=LINE('',#50520,#10712);
#8225=LINE('',#50522,#10713);
#8226=LINE('',#50525,#10714);
#8227=LINE('',#50526,#10715);
#8228=LINE('',#50528,#10716);
#8229=LINE('',#50530,#10717);
#8230=LINE('',#50531,#10718);
#8231=LINE('',#50533,#10719);
#8232=LINE('',#50535,#10720);
#8233=LINE('',#50537,#10721);
#8234=LINE('',#50540,#10722);
#8235=LINE('',#50544,#10723);
#8236=LINE('',#50545,#10724);
#8237=LINE('',#50548,#10725);
#8238=LINE('',#50551,#10726);
#8239=LINE('',#50553,#10727);
#8240=LINE('',#50554,#10728);
#8241=LINE('',#50556,#10729);
#8242=LINE('',#50945,#10730);
#8243=LINE('',#56994,#10731);
#8244=LINE('',#57021,#10732);
#8245=LINE('',#57069,#10733);
#8246=LINE('',#57117,#10734);
#8247=LINE('',#57171,#10735);
#8248=LINE('',#57219,#10736);
#8249=LINE('',#57267,#10737);
#8250=LINE('',#57321,#10738);
#8251=LINE('',#57369,#10739);
#8252=LINE('',#57417,#10740);
#8253=LINE('',#57471,#10741);
#8254=LINE('',#57519,#10742);
#8255=LINE('',#57535,#10743);
#8256=LINE('',#57560,#10744);
#8257=LINE('',#57585,#10745);
#8258=LINE('',#57610,#10746);
#8259=LINE('',#57634,#10747);
#8260=LINE('',#57659,#10748);
#8261=LINE('',#57684,#10749);
#8262=LINE('',#57708,#10750);
#8263=LINE('',#57733,#10751);
#8264=LINE('',#57758,#10752);
#8265=LINE('',#58048,#10753);
#8266=LINE('',#58050,#10754);
#8267=LINE('',#58852,#10755);
#8268=LINE('',#58858,#10756);
#8269=LINE('',#58860,#10757);
#8270=LINE('',#58862,#10758);
#8271=LINE('',#58864,#10759);
#8272=LINE('',#58866,#10760);
#8273=LINE('',#58867,#10761);
#8274=LINE('',#58870,#10762);
#8275=LINE('',#58872,#10763);
#8276=LINE('',#58873,#10764);
#8277=LINE('',#58876,#10765);
#8278=LINE('',#58878,#10766);
#8279=LINE('',#58880,#10767);
#8280=LINE('',#58881,#10768);
#8281=LINE('',#58884,#10769);
#8282=LINE('',#58886,#10770);
#8283=LINE('',#58888,#10771);
#8284=LINE('',#58889,#10772);
#8285=LINE('',#58892,#10773);
#8286=LINE('',#58894,#10774);
#8287=LINE('',#58896,#10775);
#8288=LINE('',#58898,#10776);
#8289=LINE('',#58900,#10777);
#8290=LINE('',#58902,#10778);
#8291=LINE('',#58904,#10779);
#8292=LINE('',#58905,#10780);
#8293=LINE('',#58908,#10781);
#8294=LINE('',#58909,#10782);
#8295=LINE('',#58912,#10783);
#8296=LINE('',#58914,#10784);
#8297=LINE('',#58916,#10785);
#8298=LINE('',#58917,#10786);
#8299=LINE('',#58920,#10787);
#8300=LINE('',#58922,#10788);
#8301=LINE('',#58923,#10789);
#8302=LINE('',#58926,#10790);
#8303=LINE('',#58928,#10791);
#8304=LINE('',#58929,#10792);
#8305=LINE('',#58933,#10793);
#8306=LINE('',#58935,#10794);
#8307=LINE('',#58937,#10795);
#8308=LINE('',#58939,#10796);
#8309=LINE('',#58941,#10797);
#8310=LINE('',#58942,#10798);
#8311=LINE('',#58945,#10799);
#8312=LINE('',#58947,#10800);
#8313=LINE('',#58948,#10801);
#8314=LINE('',#58950,#10802);
#8315=LINE('',#58952,#10803);
#8316=LINE('',#58953,#10804);
#8317=LINE('',#58955,#10805);
#8318=LINE('',#58958,#10806);
#8319=LINE('',#58959,#10807);
#8320=LINE('',#58962,#10808);
#8321=LINE('',#58964,#10809);
#8322=LINE('',#58966,#10810);
#8323=LINE('',#58967,#10811);
#8324=LINE('',#58970,#10812);
#8325=LINE('',#58972,#10813);
#8326=LINE('',#58973,#10814);
#8327=LINE('',#58976,#10815);
#8328=LINE('',#58977,#10816);
#8329=LINE('',#58980,#10817);
#8330=LINE('',#58981,#10818);
#8331=LINE('',#58983,#10819);
#8332=LINE('',#58984,#10820);
#8333=LINE('',#58988,#10821);
#8334=LINE('',#58989,#10822);
#8335=LINE('',#58991,#10823);
#8336=LINE('',#58992,#10824);
#8337=LINE('',#58995,#10825);
#8338=LINE('',#58997,#10826);
#8339=LINE('',#58998,#10827);
#8340=LINE('',#59002,#10828);
#8341=LINE('',#59003,#10829);
#8342=LINE('',#59004,#10830);
#8343=LINE('',#59007,#10831);
#8344=LINE('',#59009,#10832);
#8345=LINE('',#59010,#10833);
#8346=LINE('',#59013,#10834);
#8347=LINE('',#59015,#10835);
#8348=LINE('',#59016,#10836);
#8349=LINE('',#59019,#10837);
#8350=LINE('',#59021,#10838);
#8351=LINE('',#59022,#10839);
#8352=LINE('',#59026,#10840);
#8353=LINE('',#59027,#10841);
#8354=LINE('',#59028,#10842);
#8355=LINE('',#59030,#10843);
#8356=LINE('',#59033,#10844);
#8357=LINE('',#59034,#10845);
#8358=LINE('',#59036,#10846);
#8359=LINE('',#59037,#10847);
#8360=LINE('',#59041,#10848);
#8361=LINE('',#59042,#10849);
#8362=LINE('',#59043,#10850);
#8363=LINE('',#59046,#10851);
#8364=LINE('',#59047,#10852);
#8365=LINE('',#59049,#10853);
#8366=LINE('',#59052,#10854);
#8367=LINE('',#59053,#10855);
#8368=LINE('',#59056,#10856);
#8369=LINE('',#59058,#10857);
#8370=LINE('',#59059,#10858);
#8371=LINE('',#59061,#10859);
#8372=LINE('',#59062,#10860);
#8373=LINE('',#59064,#10861);
#8374=LINE('',#59065,#10862);
#8375=LINE('',#59067,#10863);
#8376=LINE('',#59071,#10864);
#8377=LINE('',#59075,#10865);
#8378=LINE('',#59081,#10866);
#8379=LINE('',#59108,#10867);
#8380=LINE('',#59174,#10868);
#8381=LINE('',#59234,#10869);
#8382=LINE('',#59294,#10870);
#8383=LINE('',#59357,#10871);
#8384=LINE('',#59417,#10872);
#8385=LINE('',#59477,#10873);
#8386=LINE('',#59540,#10874);
#8387=LINE('',#59600,#10875);
#8388=LINE('',#59666,#10876);
#8389=LINE('',#59735,#10877);
#8390=LINE('',#59801,#10878);
#8391=LINE('',#59861,#10879);
#8392=LINE('',#59924,#10880);
#8393=LINE('',#59990,#10881);
#8394=LINE('',#60050,#10882);
#8395=LINE('',#60104,#10883);
#8396=LINE('',#60158,#10884);
#8397=LINE('',#60218,#10885);
#8398=LINE('',#60284,#10886);
#8399=LINE('',#60350,#10887);
#8400=LINE('',#60419,#10888);
#8401=LINE('',#60479,#10889);
#8402=LINE('',#60542,#10890);
#8403=LINE('',#60608,#10891);
#8404=LINE('',#60674,#10892);
#8405=LINE('',#60728,#10893);
#8406=LINE('',#60782,#10894);
#8407=LINE('',#60845,#10895);
#8408=LINE('',#60911,#10896);
#8409=LINE('',#60962,#10897);
#8410=LINE('',#61025,#10898);
#8411=LINE('',#61079,#10899);
#8412=LINE('',#61142,#10900);
#8413=LINE('',#61211,#10901);
#8414=LINE('',#61274,#10902);
#8415=LINE('',#61328,#10903);
#8416=LINE('',#61388,#10904);
#8417=LINE('',#61448,#10905);
#8418=LINE('',#61508,#10906);
#8419=LINE('',#61571,#10907);
#8420=LINE('',#61625,#10908);
#8421=LINE('',#61679,#10909);
#8422=LINE('',#61745,#10910);
#8423=LINE('',#61814,#10911);
#8424=LINE('',#61877,#10912);
#8425=LINE('',#61931,#10913);
#8426=LINE('',#61997,#10914);
#8427=LINE('',#62063,#10915);
#8428=LINE('',#62123,#10916);
#8429=LINE('',#62183,#10917);
#8430=LINE('',#62237,#10918);
#8431=LINE('',#62294,#10919);
#8432=LINE('',#62360,#10920);
#8433=LINE('',#62429,#10921);
#8434=LINE('',#62492,#10922);
#8435=LINE('',#62546,#10923);
#8436=LINE('',#62612,#10924);
#8437=LINE('',#62678,#10925);
#8438=LINE('',#62737,#10926);
#8439=LINE('',#62768,#10927);
#8440=LINE('',#62798,#10928);
#8441=LINE('',#62828,#10929);
#8442=LINE('',#62873,#10930);
#8443=LINE('',#62918,#10931);
#8444=LINE('',#62948,#10932);
#8445=LINE('',#62978,#10933);
#8446=LINE('',#63007,#10934);
#8447=LINE('',#63049,#10935);
#8448=LINE('',#63079,#10936);
#8449=LINE('',#63121,#10937);
#8450=LINE('',#63151,#10938);
#8451=LINE('',#63181,#10939);
#8452=LINE('',#63223,#10940);
#8453=LINE('',#63265,#10941);
#8454=LINE('',#63295,#10942);
#8455=LINE('',#63325,#10943);
#8456=LINE('',#63367,#10944);
#8457=LINE('',#63421,#10945);
#8458=LINE('',#63451,#10946);
#8459=LINE('',#63493,#10947);
#8460=LINE('',#63522,#10948);
#8461=LINE('',#63552,#10949);
#8462=LINE('',#63595,#10950);
#8463=LINE('',#63637,#10951);
#8464=LINE('',#63667,#10952);
#8465=LINE('',#63696,#10953);
#8466=LINE('',#63738,#10954);
#8467=LINE('',#63795,#10955);
#8468=LINE('',#63824,#10956);
#8469=LINE('',#63851,#10957);
#8470=LINE('',#63880,#10958);
#8471=LINE('',#63925,#10959);
#8472=LINE('',#63968,#10960);
#8473=LINE('',#64013,#10961);
#8474=LINE('',#64043,#10962);
#8475=LINE('',#64073,#10963);
#8476=LINE('',#64102,#10964);
#8477=LINE('',#64148,#10965);
#8478=LINE('',#64178,#10966);
#8479=LINE('',#64208,#10967);
#8480=LINE('',#64237,#10968);
#8481=LINE('',#64279,#10969);
#8482=LINE('',#64322,#10970);
#8483=LINE('',#64364,#10971);
#8484=LINE('',#64394,#10972);
#8485=LINE('',#64424,#10973);
#8486=LINE('',#64453,#10974);
#8487=LINE('',#64495,#10975);
#8488=LINE('',#64526,#10976);
#8489=LINE('',#64556,#10977);
#8490=LINE('',#64598,#10978);
#8491=LINE('',#64640,#10979);
#8492=LINE('',#64671,#10980);
#8493=LINE('',#64713,#10981);
#8494=LINE('',#64743,#10982);
#8495=LINE('',#64772,#10983);
#8496=LINE('',#64802,#10984);
#8497=LINE('',#64853,#10985);
#8498=LINE('',#64858,#10986);
#8499=LINE('',#64870,#10987);
#8500=LINE('',#64885,#10988);
#8501=LINE('',#64900,#10989);
#8502=LINE('',#64915,#10990);
#8503=LINE('',#64930,#10991);
#8504=LINE('',#64945,#10992);
#8505=LINE('',#64960,#10993);
#8506=LINE('',#64988,#10994);
#8507=LINE('',#64993,#10995);
#8508=LINE('',#65005,#10996);
#8509=LINE('',#65020,#10997);
#8510=LINE('',#65035,#10998);
#8511=LINE('',#65050,#10999);
#8512=LINE('',#65065,#11000);
#8513=LINE('',#65080,#11001);
#8514=LINE('',#65108,#11002);
#8515=LINE('',#65113,#11003);
#8516=LINE('',#65125,#11004);
#8517=LINE('',#65140,#11005);
#8518=LINE('',#65155,#11006);
#8519=LINE('',#65170,#11007);
#8520=LINE('',#65185,#11008);
#8521=LINE('',#65200,#11009);
#8522=LINE('',#65215,#11010);
#8523=LINE('',#65230,#11011);
#8524=LINE('',#65245,#11012);
#8525=LINE('',#65260,#11013);
#8526=LINE('',#65275,#11014);
#8527=LINE('',#65290,#11015);
#8528=LINE('',#65305,#11016);
#8529=LINE('',#65320,#11017);
#8530=LINE('',#65340,#11018);
#8531=LINE('',#65342,#11019);
#8532=LINE('',#65344,#11020);
#8533=LINE('',#65345,#11021);
#8534=LINE('',#65348,#11022);
#8535=LINE('',#65350,#11023);
#8536=LINE('',#65351,#11024);
#8537=LINE('',#65354,#11025);
#8538=LINE('',#65356,#11026);
#8539=LINE('',#65357,#11027);
#8540=LINE('',#65359,#11028);
#8541=LINE('',#65360,#11029);
#8542=LINE('',#65374,#11030);
#8543=LINE('',#65379,#11031);
#8544=LINE('',#65391,#11032);
#8545=LINE('',#65406,#11033);
#8546=LINE('',#65421,#11034);
#8547=LINE('',#65436,#11035);
#8548=LINE('',#65451,#11036);
#8549=LINE('',#65466,#11037);
#8550=LINE('',#65481,#11038);
#8551=LINE('',#65509,#11039);
#8552=LINE('',#65514,#11040);
#8553=LINE('',#65526,#11041);
#8554=LINE('',#65541,#11042);
#8555=LINE('',#65556,#11043);
#8556=LINE('',#65571,#11044);
#8557=LINE('',#65586,#11045);
#8558=LINE('',#65601,#11046);
#8559=LINE('',#65629,#11047);
#8560=LINE('',#65634,#11048);
#8561=LINE('',#65646,#11049);
#8562=LINE('',#65661,#11050);
#8563=LINE('',#65676,#11051);
#8564=LINE('',#65691,#11052);
#8565=LINE('',#65706,#11053);
#8566=LINE('',#65721,#11054);
#8567=LINE('',#65736,#11055);
#8568=LINE('',#65751,#11056);
#8569=LINE('',#65766,#11057);
#8570=LINE('',#65781,#11058);
#8571=LINE('',#65796,#11059);
#8572=LINE('',#65811,#11060);
#8573=LINE('',#65826,#11061);
#8574=LINE('',#65841,#11062);
#8575=LINE('',#70510,#11063);
#8576=LINE('',#70512,#11064);
#8577=LINE('',#70514,#11065);
#8578=LINE('',#70516,#11066);
#8579=LINE('',#70518,#11067);
#8580=LINE('',#70519,#11068);
#8581=LINE('',#70544,#11069);
#8582=LINE('',#70554,#11070);
#8583=LINE('',#70555,#11071);
#8584=LINE('',#70557,#11072);
#8585=LINE('',#70559,#11073);
#8586=LINE('',#70561,#11074);
#8587=LINE('',#70563,#11075);
#8588=LINE('',#70570,#11076);
#8589=LINE('',#70576,#11077);
#8590=LINE('',#70581,#11078);
#8591=LINE('',#70588,#11079);
#8592=LINE('',#70594,#11080);
#8593=LINE('',#70624,#11081);
#8594=LINE('',#70629,#11082);
#8595=LINE('',#70632,#11083);
#8596=LINE('',#70638,#11084);
#8597=LINE('',#70651,#11085);
#8598=LINE('',#70660,#11086);
#8599=LINE('',#70662,#11087);
#8600=LINE('',#70669,#11088);
#8601=LINE('',#70677,#11089);
#8602=LINE('',#70681,#11090);
#8603=LINE('',#70686,#11091);
#8604=LINE('',#70692,#11092);
#8605=LINE('',#70698,#11093);
#8606=LINE('',#70705,#11094);
#8607=LINE('',#70711,#11095);
#8608=LINE('',#70717,#11096);
#8609=LINE('',#70722,#11097);
#8610=LINE('',#70726,#11098);
#8611=LINE('',#70728,#11099);
#8612=LINE('',#70731,#11100);
#8613=LINE('',#70735,#11101);
#8614=LINE('',#70739,#11102);
#8615=LINE('',#70741,#11103);
#8616=LINE('',#70744,#11104);
#8617=LINE('',#70751,#11105);
#8618=LINE('',#70756,#11106);
#8619=LINE('',#70766,#11107);
#8620=LINE('',#70772,#11108);
#8621=LINE('',#70780,#11109);
#8622=LINE('',#70786,#11110);
#8623=LINE('',#70794,#11111);
#8624=LINE('',#70800,#11112);
#8625=LINE('',#70802,#11113);
#8626=LINE('',#70804,#11114);
#8627=LINE('',#70805,#11115);
#8628=LINE('',#70807,#11116);
#8629=LINE('',#70808,#11117);
#8630=LINE('',#70812,#11118);
#8631=LINE('',#70816,#11119);
#8632=LINE('',#70820,#11120);
#8633=LINE('',#70825,#11121);
#8634=LINE('',#70828,#11122);
#8635=LINE('',#70829,#11123);
#8636=LINE('',#70832,#11124);
#8637=LINE('',#70833,#11125);
#8638=LINE('',#70835,#11126);
#8639=LINE('',#70838,#11127);
#8640=LINE('',#70841,#11128);
#8641=LINE('',#70845,#11129);
#8642=LINE('',#70847,#11130);
#8643=LINE('',#70848,#11131);
#8644=LINE('',#70856,#11132);
#8645=LINE('',#70861,#11133);
#8646=LINE('',#70863,#11134);
#8647=LINE('',#70865,#11135);
#8648=LINE('',#70866,#11136);
#8649=LINE('',#70889,#11137);
#8650=LINE('',#70893,#11138);
#8651=LINE('',#70897,#11139);
#8652=LINE('',#70901,#11140);
#8653=LINE('',#70905,#11141);
#8654=LINE('',#70909,#11142);
#8655=LINE('',#70913,#11143);
#8656=LINE('',#70917,#11144);
#8657=LINE('',#70921,#11145);
#8658=LINE('',#70925,#11146);
#8659=LINE('',#70929,#11147);
#8660=LINE('',#70933,#11148);
#8661=LINE('',#70937,#11149);
#8662=LINE('',#70943,#11150);
#8663=LINE('',#70948,#11151);
#8664=LINE('',#70950,#11152);
#8665=LINE('',#70952,#11153);
#8666=LINE('',#70953,#11154);
#8667=LINE('',#70977,#11155);
#8668=LINE('',#70980,#11156);
#8669=LINE('',#70985,#11157);
#8670=LINE('',#70988,#11158);
#8671=LINE('',#70993,#11159);
#8672=LINE('',#70996,#11160);
#8673=LINE('',#71001,#11161);
#8674=LINE('',#71004,#11162);
#8675=LINE('',#71009,#11163);
#8676=LINE('',#71012,#11164);
#8677=LINE('',#71014,#11165);
#8678=LINE('',#71015,#11166);
#8679=LINE('',#71019,#11167);
#8680=LINE('',#71025,#11168);
#8681=LINE('',#71026,#11169);
#8682=LINE('',#71027,#11170);
#8683=LINE('',#71030,#11171);
#8684=LINE('',#71035,#11172);
#8685=LINE('',#71036,#11173);
#8686=LINE('',#71040,#11174);
#8687=LINE('',#71046,#11175);
#8688=LINE('',#71047,#11176);
#8689=LINE('',#71048,#11177);
#8690=LINE('',#71054,#11178);
#8691=LINE('',#71058,#11179);
#8692=LINE('',#71059,#11180);
#8693=LINE('',#71065,#11181);
#8694=LINE('',#71069,#11182);
#8695=LINE('',#71073,#11183);
#8696=LINE('',#71077,#11184);
#8697=LINE('',#71081,#11185);
#8698=LINE('',#71086,#11186);
#8699=LINE('',#71089,#11187);
#8700=LINE('',#71094,#11188);
#8701=LINE('',#71097,#11189);
#8702=LINE('',#71102,#11190);
#8703=LINE('',#71105,#11191);
#8704=LINE('',#71109,#11192);
#8705=LINE('',#71113,#11193);
#8706=LINE('',#71118,#11194);
#8707=LINE('',#71121,#11195);
#8708=LINE('',#71125,#11196);
#8709=LINE('',#71129,#11197);
#8710=LINE('',#71134,#11198);
#8711=LINE('',#71137,#11199);
#8712=LINE('',#71141,#11200);
#8713=LINE('',#71145,#11201);
#8714=LINE('',#71150,#11202);
#8715=LINE('',#71154,#11203);
#8716=LINE('',#71158,#11204);
#8717=LINE('',#71160,#11205);
#8718=LINE('',#71162,#11206);
#8719=LINE('',#71163,#11207);
#8720=LINE('',#71185,#11208);
#8721=LINE('',#71187,#11209);
#8722=LINE('',#71189,#11210);
#8723=LINE('',#71191,#11211);
#8724=LINE('',#71194,#11212);
#8725=LINE('',#71198,#11213);
#8726=LINE('',#71203,#11214);
#8727=LINE('',#71207,#11215);
#8728=LINE('',#71209,#11216);
#8729=LINE('',#71211,#11217);
#8730=LINE('',#71212,#11218);
#8731=LINE('',#71234,#11219);
#8732=LINE('',#71236,#11220);
#8733=LINE('',#71238,#11221);
#8734=LINE('',#71240,#11222);
#8735=LINE('',#71242,#11223);
#8736=LINE('',#71243,#11224);
#8737=LINE('',#71246,#11225);
#8738=LINE('',#71250,#11226);
#8739=LINE('',#71251,#11227);
#8740=LINE('',#71253,#11228);
#8741=LINE('',#71256,#11229);
#8742=LINE('',#71259,#11230);
#8743=LINE('',#71263,#11231);
#8744=LINE('',#71264,#11232);
#8745=LINE('',#71269,#11233);
#8746=LINE('',#71273,#11234);
#8747=LINE('',#71274,#11235);
#8748=LINE('',#71278,#11236);
#8749=LINE('',#71280,#11237);
#8750=LINE('',#71282,#11238);
#8751=LINE('',#71284,#11239);
#8752=LINE('',#71286,#11240);
#8753=LINE('',#71288,#11241);
#8754=LINE('',#71290,#11242);
#8755=LINE('',#71292,#11243);
#8756=LINE('',#71294,#11244);
#8757=LINE('',#71296,#11245);
#8758=LINE('',#71298,#11246);
#8759=LINE('',#71300,#11247);
#8760=LINE('',#71304,#11248);
#8761=LINE('',#71307,#11249);
#8762=LINE('',#71311,#11250);
#8763=LINE('',#71313,#11251);
#8764=LINE('',#71314,#11252);
#8765=LINE('',#71317,#11253);
#8766=LINE('',#71322,#11254);
#8767=LINE('',#71323,#11255);
#8768=LINE('',#71326,#11256);
#8769=LINE('',#71330,#11257);
#8770=LINE('',#71331,#11258);
#8771=LINE('',#71334,#11259);
#8772=LINE('',#71337,#11260);
#8773=LINE('',#71339,#11261);
#8774=LINE('',#71345,#11262);
#8775=LINE('',#71349,#11263);
#8776=LINE('',#71353,#11264);
#8777=LINE('',#71356,#11265);
#8778=LINE('',#71359,#11266);
#8779=LINE('',#71361,#11267);
#8780=LINE('',#71364,#11268);
#8781=LINE('',#71365,#11269);
#8782=LINE('',#71367,#11270);
#8783=LINE('',#71370,#11271);
#8784=LINE('',#71372,#11272);
#8785=LINE('',#71374,#11273);
#8786=LINE('',#71376,#11274);
#8787=LINE('',#71379,#11275);
#8788=LINE('',#71381,#11276);
#8789=LINE('',#71384,#11277);
#8790=VECTOR('',#30861,1.);
#8791=VECTOR('',#30862,1.);
#8792=VECTOR('',#30863,1.);
#8793=VECTOR('',#30864,1.);
#8794=VECTOR('',#30865,1.);
#8795=VECTOR('',#30868,1.);
#8796=VECTOR('',#30869,1.);
#8797=VECTOR('',#30870,1.);
#8798=VECTOR('',#30871,1.);
#8799=VECTOR('',#30872,1.);
#8800=VECTOR('',#30875,1.);
#8801=VECTOR('',#30876,1.);
#8802=VECTOR('',#30879,1.);
#8803=VECTOR('',#30880,1.);
#8804=VECTOR('',#30883,1.);
#8805=VECTOR('',#30884,1.);
#8806=VECTOR('',#30887,1.);
#8807=VECTOR('',#30888,1.);
#8808=VECTOR('',#30889,1.);
#8809=VECTOR('',#30890,1.);
#8810=VECTOR('',#30893,1.);
#8811=VECTOR('',#30894,1.);
#8812=VECTOR('',#30895,1.);
#8813=VECTOR('',#30896,1.);
#8814=VECTOR('',#30897,1.);
#8815=VECTOR('',#30898,1.);
#8816=VECTOR('',#30901,1.);
#8817=VECTOR('',#30902,1.);
#8818=VECTOR('',#30903,1.);
#8819=VECTOR('',#30904,1.);
#8820=VECTOR('',#30905,1.);
#8821=VECTOR('',#30908,1.);
#8822=VECTOR('',#30909,1.);
#8823=VECTOR('',#30910,1.);
#8824=VECTOR('',#30913,1.);
#8825=VECTOR('',#30914,1.);
#8826=VECTOR('',#30915,1.);
#8827=VECTOR('',#30918,1.);
#8828=VECTOR('',#30919,1.);
#8829=VECTOR('',#30922,1.);
#8830=VECTOR('',#30923,1.);
#8831=VECTOR('',#30926,1.);
#8832=VECTOR('',#30927,1.);
#8833=VECTOR('',#30934,0.925000000000001);
#8834=VECTOR('',#30939,1.);
#8835=VECTOR('',#30940,1.);
#8836=VECTOR('',#30941,1.);
#8837=VECTOR('',#30942,1.);
#8838=VECTOR('',#30951,0.875);
#8839=VECTOR('',#30956,0.925000000000001);
#8840=VECTOR('',#30961,0.875);
#8841=VECTOR('',#30966,0.925000000000001);
#8842=VECTOR('',#30971,0.875);
#8843=VECTOR('',#30976,0.925000000000001);
#8844=VECTOR('',#30981,0.875);
#8845=VECTOR('',#30988,0.925000000000001);
#8846=VECTOR('',#30991,1.);
#8847=VECTOR('',#30992,1.);
#8848=VECTOR('',#30993,1.);
#8849=VECTOR('',#30994,1.);
#8850=VECTOR('',#31003,0.925000000000001);
#8851=VECTOR('',#31006,0.925000000000001);
#8852=VECTOR('',#31009,0.925000000000001);
#8853=VECTOR('',#31014,0.925000000000001);
#8854=VECTOR('',#31019,1.);
#8855=VECTOR('',#31020,1.);
#8856=VECTOR('',#31021,1.);
#8857=VECTOR('',#31022,1.);
#8858=VECTOR('',#31033,0.875);
#8859=VECTOR('',#31036,0.925000000000001);
#8860=VECTOR('',#31043,0.875);
#8861=VECTOR('',#31046,0.925000000000001);
#8862=VECTOR('',#31053,0.875);
#8863=VECTOR('',#31056,0.925000000000001);
#8864=VECTOR('',#31063,0.875);
#8865=VECTOR('',#31066,1.);
#8866=VECTOR('',#31071,1.);
#8867=VECTOR('',#31074,1.);
#8868=VECTOR('',#31075,1.);
#8869=VECTOR('',#31078,1.);
#8870=VECTOR('',#31081,1.);
#8871=VECTOR('',#31084,1.);
#8872=VECTOR('',#31085,1.);
#8873=VECTOR('',#31088,1.8);
#8874=VECTOR('',#31097,0.925000000000001);
#8875=VECTOR('',#31100,1.);
#8876=VECTOR('',#31101,1.);
#8877=VECTOR('',#31102,1.);
#8878=VECTOR('',#31103,1.);
#8879=VECTOR('',#31112,0.925000000000001);
#8880=VECTOR('',#31115,0.925000000000001);
#8881=VECTOR('',#31118,0.925000000000001);
#8882=VECTOR('',#31121,1.);
#8883=VECTOR('',#31124,1.);
#8884=VECTOR('',#31129,1.);
#8885=VECTOR('',#31130,1.);
#8886=VECTOR('',#31131,1.);
#8887=VECTOR('',#31134,1.);
#8888=VECTOR('',#31139,1.);
#8889=VECTOR('',#31140,1.);
#8890=VECTOR('',#31141,1.);
#8891=VECTOR('',#31144,1.);
#8892=VECTOR('',#31151,1.);
#8893=VECTOR('',#31152,1.);
#8894=VECTOR('',#31155,1.);
#8895=VECTOR('',#31162,1.);
#8896=VECTOR('',#31163,1.);
#8897=VECTOR('',#31166,1.);
#8898=VECTOR('',#31167,1.);
#8899=VECTOR('',#31168,1.);
#8900=VECTOR('',#31173,1.);
#8901=VECTOR('',#31176,1.);
#8902=VECTOR('',#31177,1.);
#8903=VECTOR('',#31178,1.);
#8904=VECTOR('',#31181,1.);
#8905=VECTOR('',#31184,1.);
#8906=VECTOR('',#31187,1.);
#8907=VECTOR('',#31190,1.);
#8908=VECTOR('',#31193,1.);
#8909=VECTOR('',#31198,1.);
#8910=VECTOR('',#31199,1.);
#8911=VECTOR('',#31204,1.);
#8912=VECTOR('',#31205,1.);
#8913=VECTOR('',#31206,1.);
#8914=VECTOR('',#31209,1.);
#8915=VECTOR('',#31214,1.);
#8916=VECTOR('',#31215,1.);
#8917=VECTOR('',#31218,1.);
#8918=VECTOR('',#31225,1.);
#8919=VECTOR('',#31226,1.);
#8920=VECTOR('',#31227,1.);
#8921=VECTOR('',#31230,1.);
#8922=VECTOR('',#31235,1.);
#8923=VECTOR('',#31236,1.);
#8924=VECTOR('',#31239,1.);
#8925=VECTOR('',#31248,1.);
#8926=VECTOR('',#31249,1.);
#8927=VECTOR('',#31250,1.);
#8928=VECTOR('',#31251,1.);
#8929=VECTOR('',#31252,1.);
#8930=VECTOR('',#31253,1.);
#8931=VECTOR('',#31254,1.);
#8932=VECTOR('',#31255,1.);
#8933=VECTOR('',#31256,1.);
#8934=VECTOR('',#31257,1.);
#8935=VECTOR('',#31258,1.);
#8936=VECTOR('',#31259,1.);
#8937=VECTOR('',#31260,1.);
#8938=VECTOR('',#31261,1.);
#8939=VECTOR('',#31262,1.);
#8940=VECTOR('',#31263,1.);
#8941=VECTOR('',#31264,1.);
#8942=VECTOR('',#31265,1.);
#8943=VECTOR('',#31266,1.);
#8944=VECTOR('',#31267,1.);
#8945=VECTOR('',#31268,1.);
#8946=VECTOR('',#31269,1.);
#8947=VECTOR('',#31272,1.);
#8948=VECTOR('',#31275,1.);
#8949=VECTOR('',#31278,1.);
#8950=VECTOR('',#31281,1.);
#8951=VECTOR('',#31286,1.);
#8952=VECTOR('',#31291,1.);
#8953=VECTOR('',#31292,1.);
#8954=VECTOR('',#31293,1.);
#8955=VECTOR('',#31296,1.8);
#8956=VECTOR('',#31303,1.);
#8957=VECTOR('',#31308,1.);
#8958=VECTOR('',#31309,1.);
#8959=VECTOR('',#31310,1.);
#8960=VECTOR('',#31313,1.8);
#8961=VECTOR('',#31320,1.);
#8962=VECTOR('',#31321,1.);
#8963=VECTOR('',#31322,1.);
#8964=VECTOR('',#31325,1.);
#8965=VECTOR('',#31330,1.);
#8966=VECTOR('',#31331,1.);
#8967=VECTOR('',#31334,1.);
#8968=VECTOR('',#31339,1.);
#8969=VECTOR('',#31342,1.);
#8970=VECTOR('',#31347,1.);
#8971=VECTOR('',#31348,1.);
#8972=VECTOR('',#31355,1.);
#8973=VECTOR('',#31360,1.);
#8974=VECTOR('',#31361,1.);
#8975=VECTOR('',#31364,1.);
#8976=VECTOR('',#31365,1.);
#8977=VECTOR('',#31366,1.);
#8978=VECTOR('',#31371,1.);
#8979=VECTOR('',#31374,1.);
#8980=VECTOR('',#31377,1.);
#8981=VECTOR('',#31378,1.);
#8982=VECTOR('',#31383,1.);
#8983=VECTOR('',#31384,1.);
#8984=VECTOR('',#31387,1.);
#8985=VECTOR('',#31388,1.);
#8986=VECTOR('',#31391,1.);
#8987=VECTOR('',#31392,1.);
#8988=VECTOR('',#31397,1.);
#8989=VECTOR('',#31400,1.);
#8990=VECTOR('',#31401,1.);
#8991=VECTOR('',#31406,1.);
#8992=VECTOR('',#31409,1.);
#8993=VECTOR('',#31412,1.);
#8994=VECTOR('',#31415,1.);
#8995=VECTOR('',#31420,1.);
#8996=VECTOR('',#31423,1.);
#8997=VECTOR('',#31426,1.);
#8998=VECTOR('',#31427,1.);
#8999=VECTOR('',#31430,1.);
#9000=VECTOR('',#31431,1.);
#9001=VECTOR('',#31432,1.);
#9002=VECTOR('',#31433,1.);
#9003=VECTOR('',#31436,1.);
#9004=VECTOR('',#31437,1.);
#9005=VECTOR('',#31440,1.);
#9006=VECTOR('',#31445,1.);
#9007=VECTOR('',#31446,1.);
#9008=VECTOR('',#31447,1.);
#9009=VECTOR('',#31450,1.8);
#9010=VECTOR('',#31455,1.);
#9011=VECTOR('',#31456,1.);
#9012=VECTOR('',#31459,1.);
#9013=VECTOR('',#31460,1.);
#9014=VECTOR('',#31463,1.);
#9015=VECTOR('',#31466,1.);
#9016=VECTOR('',#31471,1.);
#9017=VECTOR('',#31472,1.);
#9018=VECTOR('',#31473,1.);
#9019=VECTOR('',#31476,1.);
#9020=VECTOR('',#31483,1.);
#9021=VECTOR('',#31484,1.);
#9022=VECTOR('',#31485,1.);
#9023=VECTOR('',#31488,1.);
#9024=VECTOR('',#31495,1.);
#9025=VECTOR('',#31496,1.);
#9026=VECTOR('',#31499,1.);
#9027=VECTOR('',#31506,1.);
#9028=VECTOR('',#31507,1.);
#9029=VECTOR('',#31510,1.);
#9030=VECTOR('',#31511,1.);
#9031=VECTOR('',#31512,1.);
#9032=VECTOR('',#31517,1.);
#9033=VECTOR('',#31518,1.);
#9034=VECTOR('',#31521,1.);
#9035=VECTOR('',#31522,1.);
#9036=VECTOR('',#31523,1.);
#9037=VECTOR('',#31526,1.);
#9038=VECTOR('',#31527,1.);
#9039=VECTOR('',#31530,1.);
#9040=VECTOR('',#31533,1.);
#9041=VECTOR('',#31536,1.);
#9042=VECTOR('',#31539,1.);
#9043=VECTOR('',#31544,1.);
#9044=VECTOR('',#31545,1.);
#9045=VECTOR('',#31550,1.);
#9046=VECTOR('',#31551,1.);
#9047=VECTOR('',#31552,1.);
#9048=VECTOR('',#31555,1.);
#9049=VECTOR('',#31560,1.);
#9050=VECTOR('',#31561,1.);
#9051=VECTOR('',#31564,1.);
#9052=VECTOR('',#31571,1.);
#9053=VECTOR('',#31572,1.);
#9054=VECTOR('',#31573,1.);
#9055=VECTOR('',#31576,1.);
#9056=VECTOR('',#31583,1.);
#9057=VECTOR('',#31584,1.);
#9058=VECTOR('',#31587,1.);
#9059=VECTOR('',#31588,1.);
#9060=VECTOR('',#31591,1.);
#9061=VECTOR('',#31592,1.);
#9062=VECTOR('',#31593,1.);
#9063=VECTOR('',#31606,1.);
#9064=VECTOR('',#31609,1.);
#9065=VECTOR('',#31612,1.);
#9066=VECTOR('',#31615,1.);
#9067=VECTOR('',#31618,1.);
#9068=VECTOR('',#31619,1.);
#9069=VECTOR('',#31622,1.);
#9070=VECTOR('',#31627,1.);
#9071=VECTOR('',#31630,1.8);
#9072=VECTOR('',#31637,1.);
#9073=VECTOR('',#31638,1.);
#9074=VECTOR('',#31639,1.);
#9075=VECTOR('',#31644,1.);
#9076=VECTOR('',#31647,1.);
#9077=VECTOR('',#31648,1.);
#9078=VECTOR('',#31653,1.);
#9079=VECTOR('',#31656,1.);
#9080=VECTOR('',#31661,1.);
#9081=VECTOR('',#31664,1.);
#9082=VECTOR('',#31665,1.);
#9083=VECTOR('',#31672,1.);
#9084=VECTOR('',#31677,1.);
#9085=VECTOR('',#31678,1.);
#9086=VECTOR('',#31681,1.);
#9087=VECTOR('',#31682,1.);
#9088=VECTOR('',#31683,1.);
#9089=VECTOR('',#31688,1.);
#9090=VECTOR('',#31691,1.);
#9091=VECTOR('',#31694,1.);
#9092=VECTOR('',#31695,1.);
#9093=VECTOR('',#31702,1.);
#9094=VECTOR('',#31703,1.);
#9095=VECTOR('',#31706,1.);
#9096=VECTOR('',#31709,1.);
#9097=VECTOR('',#31712,1.);
#9098=VECTOR('',#31715,1.);
#9099=VECTOR('',#31718,1.);
#9100=VECTOR('',#31723,1.);
#9101=VECTOR('',#31724,1.);
#9102=VECTOR('',#31731,1.);
#9103=VECTOR('',#31734,1.);
#9104=VECTOR('',#31737,1.);
#9105=VECTOR('',#31738,1.);
#9106=VECTOR('',#31741,1.);
#9107=VECTOR('',#31742,1.);
#9108=VECTOR('',#31745,1.);
#9109=VECTOR('',#31750,1.);
#9110=VECTOR('',#31751,1.);
#9111=VECTOR('',#31752,1.);
#9112=VECTOR('',#31755,1.8);
#9113=VECTOR('',#31760,1.);
#9114=VECTOR('',#31761,1.);
#9115=VECTOR('',#31764,1.);
#9116=VECTOR('',#31765,1.);
#9117=VECTOR('',#31766,1.);
#9118=VECTOR('',#31767,1.);
#9119=VECTOR('',#31770,1.);
#9120=VECTOR('',#31775,1.);
#9121=VECTOR('',#31778,1.8);
#9122=VECTOR('',#31783,1.);
#9123=VECTOR('',#31784,1.);
#9124=VECTOR('',#31787,1.);
#9125=VECTOR('',#31788,1.);
#9126=VECTOR('',#31791,1.);
#9127=VECTOR('',#31796,1.);
#9128=VECTOR('',#31797,1.);
#9129=VECTOR('',#31798,1.);
#9130=VECTOR('',#31801,1.8);
#9131=VECTOR('',#31806,1.);
#9132=VECTOR('',#31807,1.);
#9133=VECTOR('',#31810,1.);
#9134=VECTOR('',#31811,1.);
#9135=VECTOR('',#31816,0.555);
#9136=VECTOR('',#31821,0.504999999999999);
#9137=VECTOR('',#31832,0.555);
#9138=VECTOR('',#31835,1.);
#9139=VECTOR('',#31840,0.555);
#9140=VECTOR('',#31845,0.504999999999999);
#9141=VECTOR('',#31850,0.555);
#9142=VECTOR('',#31851,1.);
#9143=VECTOR('',#31852,1.);
#9144=VECTOR('',#31853,1.);
#9145=VECTOR('',#31854,1.);
#9146=VECTOR('',#31855,1.);
#9147=VECTOR('',#31856,1.);
#9148=VECTOR('',#31857,1.);
#9149=VECTOR('',#31858,1.);
#9150=VECTOR('',#31859,1.);
#9151=VECTOR('',#31860,1.);
#9152=VECTOR('',#31861,1.);
#9153=VECTOR('',#31862,1.);
#9154=VECTOR('',#31863,1.);
#9155=VECTOR('',#31864,1.);
#9156=VECTOR('',#31865,1.);
#9157=VECTOR('',#31866,1.);
#9158=VECTOR('',#31867,1.);
#9159=VECTOR('',#31868,1.);
#9160=VECTOR('',#31873,1.);
#9161=VECTOR('',#31874,1.);
#9162=VECTOR('',#31875,1.);
#9163=VECTOR('',#31878,1.);
#9164=VECTOR('',#31879,1.);
#9165=VECTOR('',#31882,1.);
#9166=VECTOR('',#31883,1.);
#9167=VECTOR('',#31886,1.);
#9168=VECTOR('',#31887,1.);
#9169=VECTOR('',#31890,1.);
#9170=VECTOR('',#31891,1.);
#9171=VECTOR('',#31894,1.);
#9172=VECTOR('',#31895,1.);
#9173=VECTOR('',#31898,1.);
#9174=VECTOR('',#31899,1.);
#9175=VECTOR('',#31902,1.);
#9176=VECTOR('',#31905,1.);
#9177=VECTOR('',#31906,1.);
#9178=VECTOR('',#31907,1.);
#9179=VECTOR('',#31908,1.);
#9180=VECTOR('',#31909,1.);
#9181=VECTOR('',#31910,1.);
#9182=VECTOR('',#31911,1.);
#9183=VECTOR('',#31912,1.);
#9184=VECTOR('',#31913,1.);
#9185=VECTOR('',#31914,1.);
#9186=VECTOR('',#31915,1.);
#9187=VECTOR('',#31916,1.);
#9188=VECTOR('',#31917,1.);
#9189=VECTOR('',#31918,1.);
#9190=VECTOR('',#31919,1.);
#9191=VECTOR('',#31920,1.);
#9192=VECTOR('',#31921,1.);
#9193=VECTOR('',#31922,1.);
#9194=VECTOR('',#31923,1.);
#9195=VECTOR('',#31924,1.);
#9196=VECTOR('',#31925,1.);
#9197=VECTOR('',#31926,1.);
#9198=VECTOR('',#31931,1.);
#9199=VECTOR('',#31932,1.);
#9200=VECTOR('',#31933,1.);
#9201=VECTOR('',#31934,1.);
#9202=VECTOR('',#31935,1.);
#9203=VECTOR('',#31936,1.);
#9204=VECTOR('',#31937,1.);
#9205=VECTOR('',#31938,1.);
#9206=VECTOR('',#31939,1.);
#9207=VECTOR('',#31940,1.);
#9208=VECTOR('',#31941,1.);
#9209=VECTOR('',#31942,1.);
#9210=VECTOR('',#31943,1.);
#9211=VECTOR('',#31946,1.);
#9212=VECTOR('',#31947,1.);
#9213=VECTOR('',#31948,1.);
#9214=VECTOR('',#31949,1.);
#9215=VECTOR('',#31950,1.);
#9216=VECTOR('',#31951,1.);
#9217=VECTOR('',#31952,1.);
#9218=VECTOR('',#31953,1.);
#9219=VECTOR('',#31954,1.);
#9220=VECTOR('',#31955,1.);
#9221=VECTOR('',#31958,1.);
#9222=VECTOR('',#31959,1.);
#9223=VECTOR('',#31962,1.);
#9224=VECTOR('',#31967,1.);
#9225=VECTOR('',#31968,1.);
#9226=VECTOR('',#31969,1.);
#9227=VECTOR('',#31972,1.);
#9228=VECTOR('',#31973,1.);
#9229=VECTOR('',#31976,1.);
#9230=VECTOR('',#31977,1.);
#9231=VECTOR('',#31980,1.);
#9232=VECTOR('',#31981,1.);
#9233=VECTOR('',#31984,1.);
#9234=VECTOR('',#31985,1.);
#9235=VECTOR('',#31988,1.);
#9236=VECTOR('',#31989,1.);
#9237=VECTOR('',#31992,1.);
#9238=VECTOR('',#31993,1.);
#9239=VECTOR('',#31996,1.);
#9240=VECTOR('',#31997,1.);
#9241=VECTOR('',#32000,1.);
#9242=VECTOR('',#32001,1.);
#9243=VECTOR('',#32004,1.);
#9244=VECTOR('',#32013,1.);
#9245=VECTOR('',#32016,1.);
#9246=VECTOR('',#32029,1.);
#9247=VECTOR('',#32030,1.);
#9248=VECTOR('',#32031,1.);
#9249=VECTOR('',#32032,1.);
#9250=VECTOR('',#32035,1.);
#9251=VECTOR('',#32036,1.);
#9252=VECTOR('',#32037,1.);
#9253=VECTOR('',#32038,1.);
#9254=VECTOR('',#32041,1.);
#9255=VECTOR('',#32042,1.);
#9256=VECTOR('',#32043,1.);
#9257=VECTOR('',#32046,1.);
#9258=VECTOR('',#32047,1.);
#9259=VECTOR('',#32050,1.);
#9260=VECTOR('',#32051,1.);
#9261=VECTOR('',#32052,1.);
#9262=VECTOR('',#32053,1.);
#9263=VECTOR('',#32056,1.);
#9264=VECTOR('',#32057,1.);
#9265=VECTOR('',#32058,1.);
#9266=VECTOR('',#32059,1.);
#9267=VECTOR('',#32060,1.);
#9268=VECTOR('',#32063,1.);
#9269=VECTOR('',#32064,1.);
#9270=VECTOR('',#32065,1.);
#9271=VECTOR('',#32068,1.);
#9272=VECTOR('',#32069,1.);
#9273=VECTOR('',#32070,1.);
#9274=VECTOR('',#32071,1.);
#9275=VECTOR('',#32074,1.);
#9276=VECTOR('',#32075,1.);
#9277=VECTOR('',#32076,1.);
#9278=VECTOR('',#32077,1.);
#9279=VECTOR('',#32078,1.);
#9280=VECTOR('',#32081,1.);
#9281=VECTOR('',#32082,1.);
#9282=VECTOR('',#32085,1.);
#9283=VECTOR('',#32086,1.);
#9284=VECTOR('',#32089,1.);
#9285=VECTOR('',#32090,1.);
#9286=VECTOR('',#32093,1.);
#9287=VECTOR('',#32094,1.);
#9288=VECTOR('',#32095,1.);
#9289=VECTOR('',#32096,1.);
#9290=VECTOR('',#32099,1.);
#9291=VECTOR('',#32100,1.);
#9292=VECTOR('',#32101,1.);
#9293=VECTOR('',#32102,1.);
#9294=VECTOR('',#32103,1.);
#9295=VECTOR('',#32104,1.);
#9296=VECTOR('',#32107,1.);
#9297=VECTOR('',#32108,1.);
#9298=VECTOR('',#32109,1.);
#9299=VECTOR('',#32110,1.);
#9300=VECTOR('',#32113,1.);
#9301=VECTOR('',#32114,1.);
#9302=VECTOR('',#32115,1.);
#9303=VECTOR('',#32116,1.);
#9304=VECTOR('',#32119,1.);
#9305=VECTOR('',#32120,1.);
#9306=VECTOR('',#32121,1.);
#9307=VECTOR('',#32122,1.);
#9308=VECTOR('',#32125,1.);
#9309=VECTOR('',#32126,1.);
#9310=VECTOR('',#32127,1.);
#9311=VECTOR('',#32128,1.);
#9312=VECTOR('',#32129,1.);
#9313=VECTOR('',#32132,1.);
#9314=VECTOR('',#32133,1.);
#9315=VECTOR('',#32134,1.);
#9316=VECTOR('',#32135,1.);
#9317=VECTOR('',#32138,1.);
#9318=VECTOR('',#32139,1.);
#9319=VECTOR('',#32140,1.);
#9320=VECTOR('',#32141,1.);
#9321=VECTOR('',#32144,1.);
#9322=VECTOR('',#32145,1.);
#9323=VECTOR('',#32146,1.);
#9324=VECTOR('',#32147,1.);
#9325=VECTOR('',#32150,1.);
#9326=VECTOR('',#32151,1.);
#9327=VECTOR('',#32152,1.);
#9328=VECTOR('',#32153,1.);
#9329=VECTOR('',#32156,1.);
#9330=VECTOR('',#32157,1.);
#9331=VECTOR('',#32160,1.);
#9332=VECTOR('',#32161,1.);
#9333=VECTOR('',#32162,1.);
#9334=VECTOR('',#32165,1.);
#9335=VECTOR('',#32166,1.);
#9336=VECTOR('',#32167,1.);
#9337=VECTOR('',#32170,1.);
#9338=VECTOR('',#32171,1.);
#9339=VECTOR('',#32172,1.);
#9340=VECTOR('',#32175,1.);
#9341=VECTOR('',#32176,1.);
#9342=VECTOR('',#32177,1.);
#9343=VECTOR('',#32178,1.);
#9344=VECTOR('',#32181,1.);
#9345=VECTOR('',#32182,1.);
#9346=VECTOR('',#32183,1.);
#9347=VECTOR('',#32184,1.);
#9348=VECTOR('',#32185,1.);
#9349=VECTOR('',#32186,1.);
#9350=VECTOR('',#32189,1.);
#9351=VECTOR('',#32190,1.);
#9352=VECTOR('',#32191,1.);
#9353=VECTOR('',#32194,1.);
#9354=VECTOR('',#32195,1.);
#9355=VECTOR('',#32196,1.);
#9356=VECTOR('',#32199,1.);
#9357=VECTOR('',#32200,1.);
#9358=VECTOR('',#32203,1.);
#9359=VECTOR('',#32204,1.);
#9360=VECTOR('',#32207,1.);
#9361=VECTOR('',#32208,1.);
#9362=VECTOR('',#32209,1.);
#9363=VECTOR('',#32210,1.);
#9364=VECTOR('',#32211,1.);
#9365=VECTOR('',#32212,1.);
#9366=VECTOR('',#32213,1.);
#9367=VECTOR('',#32214,1.);
#9368=VECTOR('',#32217,1.);
#9369=VECTOR('',#32218,1.);
#9370=VECTOR('',#32219,1.);
#9371=VECTOR('',#32222,1.);
#9372=VECTOR('',#32223,1.);
#9373=VECTOR('',#32226,1.);
#9374=VECTOR('',#32227,1.);
#9375=VECTOR('',#32228,1.);
#9376=VECTOR('',#32229,1.);
#9377=VECTOR('',#32232,1.);
#9378=VECTOR('',#32233,1.);
#9379=VECTOR('',#32234,1.);
#9380=VECTOR('',#32237,1.);
#9381=VECTOR('',#32238,1.);
#9382=VECTOR('',#32241,1.);
#9383=VECTOR('',#32242,1.);
#9384=VECTOR('',#32243,1.);
#9385=VECTOR('',#32244,1.);
#9386=VECTOR('',#32247,1.);
#9387=VECTOR('',#32248,1.);
#9388=VECTOR('',#32251,1.);
#9389=VECTOR('',#32252,1.);
#9390=VECTOR('',#32253,1.);
#9391=VECTOR('',#32254,1.);
#9392=VECTOR('',#32255,1.);
#9393=VECTOR('',#32256,1.);
#9394=VECTOR('',#32257,1.);
#9395=VECTOR('',#32258,1.);
#9396=VECTOR('',#32259,1.);
#9397=VECTOR('',#32260,1.);
#9398=VECTOR('',#32261,1.);
#9399=VECTOR('',#32262,1.);
#9400=VECTOR('',#32265,1.);
#9401=VECTOR('',#32266,1.);
#9402=VECTOR('',#32267,1.);
#9403=VECTOR('',#32268,1.);
#9404=VECTOR('',#32271,1.);
#9405=VECTOR('',#32272,1.);
#9406=VECTOR('',#32273,1.);
#9407=VECTOR('',#32274,1.);
#9408=VECTOR('',#32275,1.);
#9409=VECTOR('',#32278,1.);
#9410=VECTOR('',#32279,1.);
#9411=VECTOR('',#32280,1.);
#9412=VECTOR('',#32283,1.);
#9413=VECTOR('',#32284,1.);
#9414=VECTOR('',#32285,1.);
#9415=VECTOR('',#32286,1.);
#9416=VECTOR('',#32289,1.);
#9417=VECTOR('',#32290,1.);
#9418=VECTOR('',#32291,1.);
#9419=VECTOR('',#32294,1.);
#9420=VECTOR('',#32295,1.);
#9421=VECTOR('',#32296,1.);
#9422=VECTOR('',#32299,1.);
#9423=VECTOR('',#32300,1.);
#9424=VECTOR('',#32301,1.);
#9425=VECTOR('',#32302,1.);
#9426=VECTOR('',#32305,1.);
#9427=VECTOR('',#32306,1.);
#9428=VECTOR('',#32307,1.);
#9429=VECTOR('',#32310,1.);
#9430=VECTOR('',#32311,1.);
#9431=VECTOR('',#32312,1.);
#9432=VECTOR('',#32313,1.);
#9433=VECTOR('',#32314,1.);
#9434=VECTOR('',#32315,1.);
#9435=VECTOR('',#32316,1.);
#9436=VECTOR('',#32319,1.);
#9437=VECTOR('',#32320,1.);
#9438=VECTOR('',#32323,1.);
#9439=VECTOR('',#32324,1.);
#9440=VECTOR('',#32327,1.);
#9441=VECTOR('',#32328,1.);
#9442=VECTOR('',#32329,1.);
#9443=VECTOR('',#32332,1.);
#9444=VECTOR('',#32333,1.);
#9445=VECTOR('',#32336,1.);
#9446=VECTOR('',#32339,1.);
#9447=VECTOR('',#32342,1.);
#9448=VECTOR('',#32343,1.);
#9449=VECTOR('',#32348,1.);
#9450=VECTOR('',#32349,1.);
#9451=VECTOR('',#32352,1.);
#9452=VECTOR('',#32353,1.);
#9453=VECTOR('',#32356,1.);
#9454=VECTOR('',#32357,1.);
#9455=VECTOR('',#32358,1.);
#9456=VECTOR('',#32359,1.);
#9457=VECTOR('',#32360,1.);
#9458=VECTOR('',#32363,1.);
#9459=VECTOR('',#32364,1.);
#9460=VECTOR('',#32367,1.);
#9461=VECTOR('',#32368,1.);
#9462=VECTOR('',#32371,1.);
#9463=VECTOR('',#32374,1.);
#9464=VECTOR('',#32375,1.);
#9465=VECTOR('',#32380,1.);
#9466=VECTOR('',#32381,1.);
#9467=VECTOR('',#32384,1.);
#9468=VECTOR('',#32385,1.);
#9469=VECTOR('',#32386,1.);
#9470=VECTOR('',#32389,1.);
#9471=VECTOR('',#32390,1.);
#9472=VECTOR('',#32391,1.);
#9473=VECTOR('',#32392,1.);
#9474=VECTOR('',#32393,1.);
#9475=VECTOR('',#32394,1.);
#9476=VECTOR('',#32397,1.);
#9477=VECTOR('',#32398,1.);
#9478=VECTOR('',#32399,1.);
#9479=VECTOR('',#32402,1.);
#9480=VECTOR('',#32403,1.);
#9481=VECTOR('',#32410,1.);
#9482=VECTOR('',#32411,1.);
#9483=VECTOR('',#32412,1.);
#9484=VECTOR('',#32413,1.);
#9485=VECTOR('',#32414,1.);
#9486=VECTOR('',#32417,1.);
#9487=VECTOR('',#32418,1.);
#9488=VECTOR('',#32419,1.);
#9489=VECTOR('',#32420,1.);
#9490=VECTOR('',#32421,1.);
#9491=VECTOR('',#32422,1.);
#9492=VECTOR('',#32423,1.);
#9493=VECTOR('',#32424,1.);
#9494=VECTOR('',#32427,1.);
#9495=VECTOR('',#32428,1.);
#9496=VECTOR('',#32429,1.);
#9497=VECTOR('',#32432,1.);
#9498=VECTOR('',#32433,1.);
#9499=VECTOR('',#32440,1.);
#9500=VECTOR('',#32441,1.);
#9501=VECTOR('',#32442,1.);
#9502=VECTOR('',#32447,1.);
#9503=VECTOR('',#32448,1.);
#9504=VECTOR('',#32451,1.);
#9505=VECTOR('',#32452,1.);
#9506=VECTOR('',#32453,1.);
#9507=VECTOR('',#32456,1.);
#9508=VECTOR('',#32459,1.);
#9509=VECTOR('',#32460,1.);
#9510=VECTOR('',#32463,1.);
#9511=VECTOR('',#32464,1.);
#9512=VECTOR('',#32465,1.);
#9513=VECTOR('',#32468,1.);
#9514=VECTOR('',#32469,1.);
#9515=VECTOR('',#32472,1.);
#9516=VECTOR('',#32475,1.);
#9517=VECTOR('',#32476,1.);
#9518=VECTOR('',#32479,1.);
#9519=VECTOR('',#32482,1.);
#9520=VECTOR('',#32483,1.);
#9521=VECTOR('',#32486,1.);
#9522=VECTOR('',#32487,1.);
#9523=VECTOR('',#32488,1.);
#9524=VECTOR('',#32491,1.);
#9525=VECTOR('',#32492,1.);
#9526=VECTOR('',#32493,1.);
#9527=VECTOR('',#32494,1.);
#9528=VECTOR('',#32499,1.);
#9529=VECTOR('',#32500,1.);
#9530=VECTOR('',#32501,1.);
#9531=VECTOR('',#32502,1.);
#9532=VECTOR('',#32505,1.);
#9533=VECTOR('',#32506,1.);
#9534=VECTOR('',#32509,1.);
#9535=VECTOR('',#32510,1.);
#9536=VECTOR('',#32513,1.);
#9537=VECTOR('',#32514,1.);
#9538=VECTOR('',#32515,1.);
#9539=VECTOR('',#32518,1.);
#9540=VECTOR('',#32521,1.);
#9541=VECTOR('',#32530,2.46464466094067);
#9542=VECTOR('',#32537,2.4);
#9543=VECTOR('',#32546,2.5);
#9544=VECTOR('',#32549,2.28535533905933);
#9545=VECTOR('',#32556,0.555);
#9546=VECTOR('',#32561,0.504999999999999);
#9547=VECTOR('',#32568,0.555);
#9548=VECTOR('',#32575,0.555);
#9549=VECTOR('',#32580,0.504999999999999);
#9550=VECTOR('',#32585,0.555);
#9551=VECTOR('',#32590,2.65);
#9552=VECTOR('',#32601,1.);
#9553=VECTOR('',#32608,1.);
#9554=VECTOR('',#32609,1.);
#9555=VECTOR('',#32610,1.);
#9556=VECTOR('',#32611,1.);
#9557=VECTOR('',#32614,1.);
#9558=VECTOR('',#32615,1.);
#9559=VECTOR('',#32616,1.);
#9560=VECTOR('',#32619,1.);
#9561=VECTOR('',#32620,1.);
#9562=VECTOR('',#32621,1.);
#9563=VECTOR('',#32622,1.);
#9564=VECTOR('',#32623,1.);
#9565=VECTOR('',#32624,1.);
#9566=VECTOR('',#32627,1.);
#9567=VECTOR('',#32628,1.);
#9568=VECTOR('',#32629,1.);
#9569=VECTOR('',#32632,1.);
#9570=VECTOR('',#32633,1.);
#9571=VECTOR('',#32634,1.);
#9572=VECTOR('',#32635,1.);
#9573=VECTOR('',#32638,1.);
#9574=VECTOR('',#32639,1.);
#9575=VECTOR('',#32640,1.);
#9576=VECTOR('',#32641,1.);
#9577=VECTOR('',#32644,1.);
#9578=VECTOR('',#32645,1.);
#9579=VECTOR('',#32646,1.);
#9580=VECTOR('',#32647,1.);
#9581=VECTOR('',#32650,1.);
#9582=VECTOR('',#32651,1.);
#9583=VECTOR('',#32654,1.);
#9584=VECTOR('',#32655,1.);
#9585=VECTOR('',#32656,1.);
#9586=VECTOR('',#32657,1.);
#9587=VECTOR('',#32660,1.);
#9588=VECTOR('',#32661,1.);
#9589=VECTOR('',#32662,1.);
#9590=VECTOR('',#32665,1.);
#9591=VECTOR('',#32666,1.);
#9592=VECTOR('',#32667,1.);
#9593=VECTOR('',#32668,1.);
#9594=VECTOR('',#32669,1.);
#9595=VECTOR('',#32670,1.);
#9596=VECTOR('',#32673,1.);
#9597=VECTOR('',#32674,1.);
#9598=VECTOR('',#32675,1.);
#9599=VECTOR('',#32676,1.);
#9600=VECTOR('',#32677,1.);
#9601=VECTOR('',#32680,1.);
#9602=VECTOR('',#32681,1.);
#9603=VECTOR('',#32684,1.);
#9604=VECTOR('',#32685,1.);
#9605=VECTOR('',#32686,1.);
#9606=VECTOR('',#32687,1.);
#9607=VECTOR('',#32690,1.);
#9608=VECTOR('',#32691,1.);
#9609=VECTOR('',#32692,1.);
#9610=VECTOR('',#32695,1.);
#9611=VECTOR('',#32696,1.);
#9612=VECTOR('',#32697,1.);
#9613=VECTOR('',#32700,1.);
#9614=VECTOR('',#32701,1.);
#9615=VECTOR('',#32704,1.);
#9616=VECTOR('',#32705,1.);
#9617=VECTOR('',#32706,1.);
#9618=VECTOR('',#32709,1.);
#9619=VECTOR('',#32710,1.);
#9620=VECTOR('',#32711,1.);
#9621=VECTOR('',#32714,1.);
#9622=VECTOR('',#32715,1.);
#9623=VECTOR('',#32716,1.);
#9624=VECTOR('',#32719,1.);
#9625=VECTOR('',#32720,1.);
#9626=VECTOR('',#32723,1.);
#9627=VECTOR('',#32724,1.);
#9628=VECTOR('',#32727,1.);
#9629=VECTOR('',#32728,1.);
#9630=VECTOR('',#32729,1.);
#9631=VECTOR('',#32730,1.);
#9632=VECTOR('',#32733,1.);
#9633=VECTOR('',#32734,1.);
#9634=VECTOR('',#32737,1.);
#9635=VECTOR('',#32738,1.);
#9636=VECTOR('',#32741,1.);
#9637=VECTOR('',#32742,1.);
#9638=VECTOR('',#32745,1.);
#9639=VECTOR('',#32746,1.);
#9640=VECTOR('',#32747,1.);
#9641=VECTOR('',#32750,1.);
#9642=VECTOR('',#32751,1.);
#9643=VECTOR('',#32752,1.);
#9644=VECTOR('',#32755,1.);
#9645=VECTOR('',#32756,1.);
#9646=VECTOR('',#32757,1.);
#9647=VECTOR('',#32760,1.);
#9648=VECTOR('',#32761,1.);
#9649=VECTOR('',#32762,1.);
#9650=VECTOR('',#32765,1.);
#9651=VECTOR('',#32766,1.);
#9652=VECTOR('',#32769,1.);
#9653=VECTOR('',#32770,1.);
#9654=VECTOR('',#32773,1.);
#9655=VECTOR('',#32774,1.);
#9656=VECTOR('',#32775,1.);
#9657=VECTOR('',#32778,1.);
#9658=VECTOR('',#32779,1.);
#9659=VECTOR('',#32780,1.);
#9660=VECTOR('',#32781,1.);
#9661=VECTOR('',#32782,1.);
#9662=VECTOR('',#32783,1.);
#9663=VECTOR('',#32784,1.);
#9664=VECTOR('',#32785,1.);
#9665=VECTOR('',#32786,1.);
#9666=VECTOR('',#32787,1.);
#9667=VECTOR('',#32788,1.);
#9668=VECTOR('',#32789,1.);
#9669=VECTOR('',#32792,1.);
#9670=VECTOR('',#32793,1.);
#9671=VECTOR('',#32794,1.);
#9672=VECTOR('',#32795,1.);
#9673=VECTOR('',#32798,1.);
#9674=VECTOR('',#32799,1.);
#9675=VECTOR('',#32800,1.);
#9676=VECTOR('',#32803,1.);
#9677=VECTOR('',#32804,1.);
#9678=VECTOR('',#32807,1.);
#9679=VECTOR('',#32808,1.);
#9680=VECTOR('',#32811,1.);
#9681=VECTOR('',#32812,1.);
#9682=VECTOR('',#32815,1.);
#9683=VECTOR('',#32816,1.);
#9684=VECTOR('',#32817,1.);
#9685=VECTOR('',#32818,1.);
#9686=VECTOR('',#32821,1.);
#9687=VECTOR('',#32822,1.);
#9688=VECTOR('',#32825,1.);
#9689=VECTOR('',#32826,1.);
#9690=VECTOR('',#32827,1.);
#9691=VECTOR('',#32830,1.);
#9692=VECTOR('',#32831,1.);
#9693=VECTOR('',#32832,1.);
#9694=VECTOR('',#32833,1.);
#9695=VECTOR('',#32836,1.);
#9696=VECTOR('',#32839,1.);
#9697=VECTOR('',#32840,1.);
#9698=VECTOR('',#32841,1.);
#9699=VECTOR('',#32844,1.);
#9700=VECTOR('',#32845,1.);
#9701=VECTOR('',#32848,1.);
#9702=VECTOR('',#32849,1.);
#9703=VECTOR('',#32850,1.);
#9704=VECTOR('',#32853,1.);
#9705=VECTOR('',#32854,1.);
#9706=VECTOR('',#32855,1.);
#9707=VECTOR('',#32858,1.);
#9708=VECTOR('',#32859,1.);
#9709=VECTOR('',#32860,1.);
#9710=VECTOR('',#32861,1.);
#9711=VECTOR('',#32864,1.);
#9712=VECTOR('',#32865,1.);
#9713=VECTOR('',#32868,1.);
#9714=VECTOR('',#32873,1.);
#9715=VECTOR('',#32874,1.);
#9716=VECTOR('',#32875,1.);
#9717=VECTOR('',#32878,1.);
#9718=VECTOR('',#32879,1.);
#9719=VECTOR('',#32880,1.);
#9720=VECTOR('',#32881,1.);
#9721=VECTOR('',#32884,1.);
#9722=VECTOR('',#32885,1.);
#9723=VECTOR('',#32886,1.);
#9724=VECTOR('',#32887,1.);
#9725=VECTOR('',#32888,1.);
#9726=VECTOR('',#32891,1.);
#9727=VECTOR('',#32892,1.);
#9728=VECTOR('',#32893,1.);
#9729=VECTOR('',#32896,1.);
#9730=VECTOR('',#32897,1.);
#9731=VECTOR('',#32898,1.);
#9732=VECTOR('',#32901,1.);
#9733=VECTOR('',#32906,1.);
#9734=VECTOR('',#32909,1.);
#9735=VECTOR('',#32912,1.);
#9736=VECTOR('',#32913,1.);
#9737=VECTOR('',#32916,1.);
#9738=VECTOR('',#32919,1.);
#9739=VECTOR('',#32920,1.);
#9740=VECTOR('',#32921,1.);
#9741=VECTOR('',#32922,1.);
#9742=VECTOR('',#32923,1.);
#9743=VECTOR('',#32924,1.);
#9744=VECTOR('',#32925,1.);
#9745=VECTOR('',#32926,1.);
#9746=VECTOR('',#32929,1.);
#9747=VECTOR('',#32934,1.);
#9748=VECTOR('',#32935,1.);
#9749=VECTOR('',#32936,1.);
#9750=VECTOR('',#32939,1.);
#9751=VECTOR('',#32940,1.);
#9752=VECTOR('',#32943,1.);
#9753=VECTOR('',#32944,1.);
#9754=VECTOR('',#32945,1.);
#9755=VECTOR('',#32948,1.);
#9756=VECTOR('',#32949,1.);
#9757=VECTOR('',#32950,1.);
#9758=VECTOR('',#32953,1.);
#9759=VECTOR('',#32956,1.);
#9760=VECTOR('',#32957,1.);
#9761=VECTOR('',#32958,1.);
#9762=VECTOR('',#32961,1.);
#9763=VECTOR('',#32966,1.);
#9764=VECTOR('',#32967,1.);
#9765=VECTOR('',#32968,1.);
#9766=VECTOR('',#32969,1.);
#9767=VECTOR('',#32972,1.);
#9768=VECTOR('',#32973,1.);
#9769=VECTOR('',#32978,1.);
#9770=VECTOR('',#32979,1.);
#9771=VECTOR('',#32982,1.);
#9772=VECTOR('',#32983,1.);
#9773=VECTOR('',#32984,1.);
#9774=VECTOR('',#32987,1.);
#9775=VECTOR('',#32992,1.);
#9776=VECTOR('',#32993,1.);
#9777=VECTOR('',#32994,1.);
#9778=VECTOR('',#32997,1.);
#9779=VECTOR('',#33000,1.);
#9780=VECTOR('',#33001,1.);
#9781=VECTOR('',#33004,1.);
#9782=VECTOR('',#33005,1.);
#9783=VECTOR('',#33008,1.);
#9784=VECTOR('',#33011,1.);
#9785=VECTOR('',#33016,1.);
#9786=VECTOR('',#33017,1.);
#9787=VECTOR('',#33018,1.);
#9788=VECTOR('',#33021,1.);
#9789=VECTOR('',#33026,1.);
#9790=VECTOR('',#33027,1.);
#9791=VECTOR('',#33034,1.);
#9792=VECTOR('',#33037,1.);
#9793=VECTOR('',#33040,1.);
#9794=VECTOR('',#33041,1.);
#9795=VECTOR('',#33044,1.);
#9796=VECTOR('',#33045,1.);
#9797=VECTOR('',#33048,1.);
#9798=VECTOR('',#33053,1.);
#9799=VECTOR('',#33054,1.);
#9800=VECTOR('',#33059,1.);
#9801=VECTOR('',#33062,1.);
#9802=VECTOR('',#33063,1.);
#9803=VECTOR('',#33064,1.);
#9804=VECTOR('',#33067,1.);
#9805=VECTOR('',#33072,1.);
#9806=VECTOR('',#33073,1.);
#9807=VECTOR('',#33080,1.);
#9808=VECTOR('',#33083,1.);
#9809=VECTOR('',#33086,1.);
#9810=VECTOR('',#33087,1.);
#9811=VECTOR('',#33090,1.);
#9812=VECTOR('',#33091,1.);
#9813=VECTOR('',#33094,1.);
#9814=VECTOR('',#33099,1.);
#9815=VECTOR('',#33100,1.);
#9816=VECTOR('',#33105,1.);
#9817=VECTOR('',#33122,1.);
#9818=VECTOR('',#33123,1.);
#9819=VECTOR('',#33124,1.);
#9820=VECTOR('',#33125,1.);
#9821=VECTOR('',#33126,1.);
#9822=VECTOR('',#33127,1.);
#9823=VECTOR('',#33130,1.);
#9824=VECTOR('',#33131,1.);
#9825=VECTOR('',#33132,1.);
#9826=VECTOR('',#33133,1.);
#9827=VECTOR('',#33134,1.);
#9828=VECTOR('',#33137,1.);
#9829=VECTOR('',#33138,1.);
#9830=VECTOR('',#33141,1.);
#9831=VECTOR('',#33142,1.);
#9832=VECTOR('',#33143,1.);
#9833=VECTOR('',#33144,1.);
#9834=VECTOR('',#33147,1.);
#9835=VECTOR('',#33148,1.);
#9836=VECTOR('',#33149,1.);
#9837=VECTOR('',#33152,1.);
#9838=VECTOR('',#33153,1.);
#9839=VECTOR('',#33154,1.);
#9840=VECTOR('',#33155,1.);
#9841=VECTOR('',#33156,1.);
#9842=VECTOR('',#33157,1.);
#9843=VECTOR('',#33160,1.);
#9844=VECTOR('',#33161,1.);
#9845=VECTOR('',#33162,1.);
#9846=VECTOR('',#33163,1.);
#9847=VECTOR('',#33164,1.);
#9848=VECTOR('',#33167,1.);
#9849=VECTOR('',#33168,1.);
#9850=VECTOR('',#33169,1.);
#9851=VECTOR('',#33172,1.);
#9852=VECTOR('',#33173,1.);
#9853=VECTOR('',#33180,1.);
#9854=VECTOR('',#33181,1.);
#9855=VECTOR('',#33182,1.);
#9856=VECTOR('',#33183,1.);
#9857=VECTOR('',#33184,1.);
#9858=VECTOR('',#33185,1.);
#9859=VECTOR('',#33188,1.);
#9860=VECTOR('',#33189,1.);
#9861=VECTOR('',#33190,1.);
#9862=VECTOR('',#33191,1.);
#9863=VECTOR('',#33194,1.);
#9864=VECTOR('',#33195,1.);
#9865=VECTOR('',#33202,1.);
#9866=VECTOR('',#33203,1.);
#9867=VECTOR('',#33204,1.);
#9868=VECTOR('',#33205,1.);
#9869=VECTOR('',#33208,1.);
#9870=VECTOR('',#33209,1.);
#9871=VECTOR('',#33212,1.);
#9872=VECTOR('',#33213,1.);
#9873=VECTOR('',#33214,1.);
#9874=VECTOR('',#33217,0.925000000000001);
#9875=VECTOR('',#33224,0.875);
#9876=VECTOR('',#33227,0.925000000000001);
#9877=VECTOR('',#33230,0.925000000000001);
#9878=VECTOR('',#33237,0.875);
#9879=VECTOR('',#33240,0.925000000000001);
#9880=VECTOR('',#33243,1.);
#9881=VECTOR('',#33244,1.);
#9882=VECTOR('',#33247,1.);
#9883=VECTOR('',#33248,1.);
#9884=VECTOR('',#33251,1.);
#9885=VECTOR('',#33252,1.);
#9886=VECTOR('',#33259,1.);
#9887=VECTOR('',#33260,1.);
#9888=VECTOR('',#33263,1.);
#9889=VECTOR('',#33264,1.);
#9890=VECTOR('',#33275,1.);
#9891=VECTOR('',#33278,1.);
#9892=VECTOR('',#33283,1.);
#9893=VECTOR('',#33284,1.);
#9894=VECTOR('',#33285,1.);
#9895=VECTOR('',#33288,1.);
#9896=VECTOR('',#33295,1.);
#9897=VECTOR('',#33296,1.);
#9898=VECTOR('',#33297,1.);
#9899=VECTOR('',#33300,1.);
#9900=VECTOR('',#33307,1.);
#9901=VECTOR('',#33308,1.);
#9902=VECTOR('',#33309,1.);
#9903=VECTOR('',#33312,1.);
#9904=VECTOR('',#33319,1.);
#9905=VECTOR('',#33320,1.);
#9906=VECTOR('',#33323,1.);
#9907=VECTOR('',#33324,1.);
#9908=VECTOR('',#33325,1.);
#9909=VECTOR('',#33328,1.);
#9910=VECTOR('',#33333,1.);
#9911=VECTOR('',#33334,1.);
#9912=VECTOR('',#33337,1.);
#9913=VECTOR('',#33350,1.);
#9914=VECTOR('',#33351,1.);
#9915=VECTOR('',#33352,1.);
#9916=VECTOR('',#33353,1.);
#9917=VECTOR('',#33358,1.);
#9918=VECTOR('',#33363,1.);
#9919=VECTOR('',#33364,1.);
#9920=VECTOR('',#33365,1.);
#9921=VECTOR('',#33368,1.);
#9922=VECTOR('',#33369,1.);
#9923=VECTOR('',#33370,1.);
#9924=VECTOR('',#33373,1.);
#9925=VECTOR('',#33378,1.);
#9926=VECTOR('',#33379,1.);
#9927=VECTOR('',#33382,1.);
#9928=VECTOR('',#33389,1.);
#9929=VECTOR('',#33390,1.);
#9930=VECTOR('',#33391,1.);
#9931=VECTOR('',#33394,1.);
#9932=VECTOR('',#33401,1.);
#9933=VECTOR('',#33402,1.);
#9934=VECTOR('',#33403,1.);
#9935=VECTOR('',#33410,1.);
#9936=VECTOR('',#33413,1.);
#9937=VECTOR('',#33416,1.);
#9938=VECTOR('',#33417,1.);
#9939=VECTOR('',#33420,1.);
#9940=VECTOR('',#33425,1.);
#9941=VECTOR('',#33426,1.);
#9942=VECTOR('',#33431,1.);
#9943=VECTOR('',#33432,1.);
#9944=VECTOR('',#33437,1.);
#9945=VECTOR('',#33438,1.);
#9946=VECTOR('',#33439,1.);
#9947=VECTOR('',#33440,1.);
#9948=VECTOR('',#33443,1.);
#9949=VECTOR('',#33450,1.);
#9950=VECTOR('',#33451,1.);
#9951=VECTOR('',#33452,1.);
#9952=VECTOR('',#33455,1.);
#9953=VECTOR('',#33462,1.);
#9954=VECTOR('',#33463,1.);
#9955=VECTOR('',#33464,1.);
#9956=VECTOR('',#33467,1.);
#9957=VECTOR('',#33470,1.);
#9958=VECTOR('',#33473,1.);
#9959=VECTOR('',#33474,1.);
#9960=VECTOR('',#33477,1.);
#9961=VECTOR('',#33478,1.);
#9962=VECTOR('',#33479,1.);
#9963=VECTOR('',#33480,1.);
#9964=VECTOR('',#33483,1.);
#9965=VECTOR('',#33490,1.);
#9966=VECTOR('',#33491,1.);
#9967=VECTOR('',#33492,1.);
#9968=VECTOR('',#33495,1.);
#9969=VECTOR('',#33502,1.);
#9970=VECTOR('',#33503,1.);
#9971=VECTOR('',#33504,1.);
#9972=VECTOR('',#33507,1.);
#9973=VECTOR('',#33512,1.);
#9974=VECTOR('',#33513,1.);
#9975=VECTOR('',#33514,1.);
#9976=VECTOR('',#33515,1.);
#9977=VECTOR('',#33518,1.);
#9978=VECTOR('',#33525,1.);
#9979=VECTOR('',#33526,1.);
#9980=VECTOR('',#33527,1.);
#9981=VECTOR('',#33530,1.);
#9982=VECTOR('',#33537,1.);
#9983=VECTOR('',#33538,1.);
#9984=VECTOR('',#33539,1.);
#9985=VECTOR('',#33542,1.);
#9986=VECTOR('',#33547,1.);
#9987=VECTOR('',#33548,1.);
#9988=VECTOR('',#33549,1.);
#9989=VECTOR('',#33550,1.);
#9990=VECTOR('',#33553,1.);
#9991=VECTOR('',#33560,1.);
#9992=VECTOR('',#33561,1.);
#9993=VECTOR('',#33562,1.);
#9994=VECTOR('',#33565,1.);
#9995=VECTOR('',#33572,1.);
#9996=VECTOR('',#33573,1.);
#9997=VECTOR('',#33574,1.);
#9998=VECTOR('',#33577,1.);
#9999=VECTOR('',#33578,1.);
#10000=VECTOR('',#33579,1.);
#10001=VECTOR('',#33582,1.);
#10002=VECTOR('',#33585,1.);
#10003=VECTOR('',#33588,1.);
#10004=VECTOR('',#33591,1.);
#10005=VECTOR('',#33592,1.);
#10006=VECTOR('',#33595,1.);
#10007=VECTOR('',#33602,0.95);
#10008=VECTOR('',#33611,1.);
#10009=VECTOR('',#33614,0.46);
#10010=VECTOR('',#33621,0.41);
#10011=VECTOR('',#33624,0.454999999999998);
#10012=VECTOR('',#33629,0.405000000000001);
#10013=VECTOR('',#33634,0.405000000000001);
#10014=VECTOR('',#33637,0.205);
#10015=VECTOR('',#33640,0.5);
#10016=VECTOR('',#33643,1.);
#10017=VECTOR('',#33644,1.);
#10018=VECTOR('',#33647,1.);
#10019=VECTOR('',#33650,1.);
#10020=VECTOR('',#33653,1.);
#10021=VECTOR('',#33658,1.);
#10022=VECTOR('',#33661,1.);
#10023=VECTOR('',#33670,1.);
#10024=VECTOR('',#33673,1.);
#10025=VECTOR('',#33688,1.725);
#10026=VECTOR('',#33693,1.8);
#10027=VECTOR('',#33698,2.705);
#10028=VECTOR('',#33705,2.655);
#10029=VECTOR('',#33732,5.);
#10030=VECTOR('',#33741,5.35);
#10031=VECTOR('',#33746,5.4);
#10032=VECTOR('',#33749,5.35);
#10033=VECTOR('',#33752,1.);
#10034=VECTOR('',#33753,1.);
#10035=VECTOR('',#33754,1.);
#10036=VECTOR('',#33757,1.);
#10037=VECTOR('',#33762,1.);
#10038=VECTOR('',#33763,1.);
#10039=VECTOR('',#33764,1.);
#10040=VECTOR('',#33767,1.);
#10041=VECTOR('',#33774,1.);
#10042=VECTOR('',#33775,1.);
#10043=VECTOR('',#33776,1.);
#10044=VECTOR('',#33779,1.);
#10045=VECTOR('',#33786,1.);
#10046=VECTOR('',#33787,1.);
#10047=VECTOR('',#33794,1.);
#10048=VECTOR('',#33799,1.);
#10049=VECTOR('',#33804,1.);
#10050=VECTOR('',#33807,1.);
#10051=VECTOR('',#33814,1.5);
#10052=VECTOR('',#33819,1.5);
#10053=VECTOR('',#33822,1.5);
#10054=VECTOR('',#33825,1.5);
#10055=VECTOR('',#33828,1.5);
#10056=VECTOR('',#33833,1.2866);
#10057=VECTOR('',#33838,1.2866);
#10058=VECTOR('',#33841,1.2866);
#10059=VECTOR('',#33844,1.2866);
#10060=VECTOR('',#33847,1.);
#10061=VECTOR('',#33848,1.);
#10062=VECTOR('',#33849,1.);
#10063=VECTOR('',#33852,1.);
#10064=VECTOR('',#33853,1.);
#10065=VECTOR('',#33860,1.);
#10066=VECTOR('',#33861,1.);
#10067=VECTOR('',#33862,1.);
#10068=VECTOR('',#33865,1.);
#10069=VECTOR('',#33866,1.);
#10070=VECTOR('',#33873,1.);
#10071=VECTOR('',#33874,1.);
#10072=VECTOR('',#33875,1.);
#10073=VECTOR('',#33878,1.);
#10074=VECTOR('',#33879,1.);
#10075=VECTOR('',#33886,1.);
#10076=VECTOR('',#33887,1.);
#10077=VECTOR('',#33888,1.);
#10078=VECTOR('',#33891,1.);
#10079=VECTOR('',#33892,1.);
#10080=VECTOR('',#33899,1.);
#10081=VECTOR('',#33900,1.);
#10082=VECTOR('',#33901,1.);
#10083=VECTOR('',#33904,1.);
#10084=VECTOR('',#33905,1.);
#10085=VECTOR('',#33912,1.);
#10086=VECTOR('',#33913,1.);
#10087=VECTOR('',#33914,1.);
#10088=VECTOR('',#33917,1.);
#10089=VECTOR('',#33918,1.);
#10090=VECTOR('',#33927,1.);
#10091=VECTOR('',#33928,1.);
#10092=VECTOR('',#33929,1.);
#10093=VECTOR('',#33932,1.);
#10094=VECTOR('',#33933,1.);
#10095=VECTOR('',#33940,1.);
#10096=VECTOR('',#33941,1.);
#10097=VECTOR('',#33942,1.);
#10098=VECTOR('',#33945,1.);
#10099=VECTOR('',#33946,1.);
#10100=VECTOR('',#33953,1.);
#10101=VECTOR('',#33954,1.);
#10102=VECTOR('',#33955,1.);
#10103=VECTOR('',#33958,1.);
#10104=VECTOR('',#33959,1.);
#10105=VECTOR('',#33966,1.);
#10106=VECTOR('',#33967,1.);
#10107=VECTOR('',#33968,1.);
#10108=VECTOR('',#33971,1.);
#10109=VECTOR('',#33972,1.);
#10110=VECTOR('',#33979,1.);
#10111=VECTOR('',#33980,1.);
#10112=VECTOR('',#33981,1.);
#10113=VECTOR('',#33984,1.);
#10114=VECTOR('',#33985,1.);
#10115=VECTOR('',#33992,1.);
#10116=VECTOR('',#33993,1.);
#10117=VECTOR('',#33994,1.);
#10118=VECTOR('',#33997,1.);
#10119=VECTOR('',#33998,1.);
#10120=VECTOR('',#34005,1.);
#10121=VECTOR('',#34006,1.);
#10122=VECTOR('',#34007,1.);
#10123=VECTOR('',#34010,1.);
#10124=VECTOR('',#34011,1.);
#10125=VECTOR('',#34018,1.);
#10126=VECTOR('',#34019,1.);
#10127=VECTOR('',#34020,1.);
#10128=VECTOR('',#34023,1.);
#10129=VECTOR('',#34024,1.);
#10130=VECTOR('',#34031,1.);
#10131=VECTOR('',#34032,1.);
#10132=VECTOR('',#34033,1.);
#10133=VECTOR('',#34036,1.);
#10134=VECTOR('',#34037,1.);
#10135=VECTOR('',#34044,1.);
#10136=VECTOR('',#34045,1.);
#10137=VECTOR('',#34046,1.);
#10138=VECTOR('',#34049,1.);
#10139=VECTOR('',#34050,1.);
#10140=VECTOR('',#34057,1.);
#10141=VECTOR('',#34058,1.);
#10142=VECTOR('',#34059,1.);
#10143=VECTOR('',#34062,1.);
#10144=VECTOR('',#34063,1.);
#10145=VECTOR('',#34070,1.);
#10146=VECTOR('',#34071,1.);
#10147=VECTOR('',#34072,1.);
#10148=VECTOR('',#34075,1.);
#10149=VECTOR('',#34076,1.);
#10150=VECTOR('',#34083,1.);
#10151=VECTOR('',#34084,1.);
#10152=VECTOR('',#34085,1.);
#10153=VECTOR('',#34088,1.);
#10154=VECTOR('',#34089,1.);
#10155=VECTOR('',#34096,1.);
#10156=VECTOR('',#34097,1.);
#10157=VECTOR('',#34098,1.);
#10158=VECTOR('',#34101,1.);
#10159=VECTOR('',#34102,1.);
#10160=VECTOR('',#34109,1.);
#10161=VECTOR('',#34110,1.);
#10162=VECTOR('',#34111,1.);
#10163=VECTOR('',#34114,1.);
#10164=VECTOR('',#34115,1.);
#10165=VECTOR('',#34122,1.);
#10166=VECTOR('',#34123,1.);
#10167=VECTOR('',#34124,1.);
#10168=VECTOR('',#34127,1.);
#10169=VECTOR('',#34128,1.);
#10170=VECTOR('',#34135,1.);
#10171=VECTOR('',#34136,1.);
#10172=VECTOR('',#34137,1.);
#10173=VECTOR('',#34140,1.);
#10174=VECTOR('',#34141,1.);
#10175=VECTOR('',#34148,1.);
#10176=VECTOR('',#34149,1.);
#10177=VECTOR('',#34150,1.);
#10178=VECTOR('',#34153,1.);
#10179=VECTOR('',#34154,1.);
#10180=VECTOR('',#34163,2.175);
#10181=VECTOR('',#34320,2.6);
#10182=VECTOR('',#34325,2.65);
#10183=VECTOR('',#34330,2.575);
#10184=VECTOR('',#34341,2.2);
#10185=VECTOR('',#34350,0.4);
#10186=VECTOR('',#34355,0.4);
#10187=VECTOR('',#34358,0.4);
#10188=VECTOR('',#34361,0.4);
#10189=VECTOR('',#34364,0.4);
#10190=VECTOR('',#34367,0.4);
#10191=VECTOR('',#34370,0.4);
#10192=VECTOR('',#34373,0.4);
#10193=VECTOR('',#34376,0.4);
#10194=VECTOR('',#34379,0.4);
#10195=VECTOR('',#34382,0.4);
#10196=VECTOR('',#34385,0.4);
#10197=VECTOR('',#34388,0.4);
#10198=VECTOR('',#34391,0.4);
#10199=VECTOR('',#34394,0.4);
#10200=VECTOR('',#34397,0.322275);
#10201=VECTOR('',#34402,0.322275);
#10202=VECTOR('',#34405,0.322275);
#10203=VECTOR('',#34408,0.322275);
#10204=VECTOR('',#34411,0.322275);
#10205=VECTOR('',#34414,0.322275);
#10206=VECTOR('',#34417,0.322275);
#10207=VECTOR('',#34420,0.322275);
#10208=VECTOR('',#34423,0.322275);
#10209=VECTOR('',#34426,0.322275);
#10210=VECTOR('',#34429,0.322275);
#10211=VECTOR('',#34432,0.322275);
#10212=VECTOR('',#34435,0.322275);
#10213=VECTOR('',#34438,0.322275);
#10214=VECTOR('',#34441,0.322275);
#10215=VECTOR('',#34444,1.);
#10216=VECTOR('',#34445,1.);
#10217=VECTOR('',#34446,1.);
#10218=VECTOR('',#34451,1.);
#10219=VECTOR('',#34454,1.);
#10220=VECTOR('',#34457,1.);
#10221=VECTOR('',#34458,1.);
#10222=VECTOR('',#34459,1.);
#10223=VECTOR('',#34464,1.);
#10224=VECTOR('',#34467,1.);
#10225=VECTOR('',#34470,1.);
#10226=VECTOR('',#34471,1.);
#10227=VECTOR('',#34472,1.);
#10228=VECTOR('',#34477,1.);
#10229=VECTOR('',#34480,1.);
#10230=VECTOR('',#34483,1.);
#10231=VECTOR('',#34484,1.);
#10232=VECTOR('',#34485,1.);
#10233=VECTOR('',#34490,1.);
#10234=VECTOR('',#34493,1.);
#10235=VECTOR('',#34496,1.);
#10236=VECTOR('',#34497,1.);
#10237=VECTOR('',#34498,1.);
#10238=VECTOR('',#34503,1.);
#10239=VECTOR('',#34506,1.);
#10240=VECTOR('',#34509,1.);
#10241=VECTOR('',#34510,1.);
#10242=VECTOR('',#34511,1.);
#10243=VECTOR('',#34516,1.);
#10244=VECTOR('',#34519,1.);
#10245=VECTOR('',#34522,1.);
#10246=VECTOR('',#34523,1.);
#10247=VECTOR('',#34524,1.);
#10248=VECTOR('',#34529,1.);
#10249=VECTOR('',#34532,1.);
#10250=VECTOR('',#34535,1.);
#10251=VECTOR('',#34536,1.);
#10252=VECTOR('',#34537,1.);
#10253=VECTOR('',#34542,1.);
#10254=VECTOR('',#34545,1.);
#10255=VECTOR('',#34548,1.);
#10256=VECTOR('',#34549,1.);
#10257=VECTOR('',#34550,1.);
#10258=VECTOR('',#34555,1.);
#10259=VECTOR('',#34558,1.);
#10260=VECTOR('',#34561,1.);
#10261=VECTOR('',#34562,1.);
#10262=VECTOR('',#34563,1.);
#10263=VECTOR('',#34568,1.);
#10264=VECTOR('',#34571,1.);
#10265=VECTOR('',#34574,1.);
#10266=VECTOR('',#34575,1.);
#10267=VECTOR('',#34576,1.);
#10268=VECTOR('',#34581,1.);
#10269=VECTOR('',#34584,1.);
#10270=VECTOR('',#34587,1.);
#10271=VECTOR('',#34588,1.);
#10272=VECTOR('',#34589,1.);
#10273=VECTOR('',#34594,1.);
#10274=VECTOR('',#34597,1.);
#10275=VECTOR('',#34600,1.);
#10276=VECTOR('',#34601,1.);
#10277=VECTOR('',#34602,1.);
#10278=VECTOR('',#34607,1.);
#10279=VECTOR('',#34610,1.);
#10280=VECTOR('',#34613,1.);
#10281=VECTOR('',#34614,1.);
#10282=VECTOR('',#34615,1.);
#10283=VECTOR('',#34620,1.);
#10284=VECTOR('',#34625,1.);
#10285=VECTOR('',#34628,1.);
#10286=VECTOR('',#34629,1.);
#10287=VECTOR('',#34630,1.);
#10288=VECTOR('',#34635,1.);
#10289=VECTOR('',#34638,1.);
#10290=VECTOR('',#34641,1.);
#10291=VECTOR('',#34642,1.);
#10292=VECTOR('',#34643,1.);
#10293=VECTOR('',#34648,1.);
#10294=VECTOR('',#34651,1.);
#10295=VECTOR('',#34654,1.);
#10296=VECTOR('',#34655,1.);
#10297=VECTOR('',#34656,1.);
#10298=VECTOR('',#34661,1.);
#10299=VECTOR('',#34664,1.);
#10300=VECTOR('',#34667,1.);
#10301=VECTOR('',#34668,1.);
#10302=VECTOR('',#34669,1.);
#10303=VECTOR('',#34674,1.);
#10304=VECTOR('',#34677,1.);
#10305=VECTOR('',#34694,1.1);
#10306=VECTOR('',#34735,0.375);
#10307=VECTOR('',#34746,1.);
#10308=VECTOR('',#34751,1.05);
#10309=VECTOR('',#34760,0.4);
#10310=VECTOR('',#34767,1.);
#10311=VECTOR('',#34768,1.);
#10312=VECTOR('',#34769,1.);
#10313=VECTOR('',#34770,1.);
#10314=VECTOR('',#34771,1.);
#10315=VECTOR('',#34772,1.);
#10316=VECTOR('',#34777,1.);
#10317=VECTOR('',#34778,1.);
#10318=VECTOR('',#34779,1.);
#10319=VECTOR('',#34782,1.);
#10320=VECTOR('',#34783,1.);
#10321=VECTOR('',#34786,1.);
#10322=VECTOR('',#34787,1.);
#10323=VECTOR('',#34790,1.);
#10324=VECTOR('',#34791,1.);
#10325=VECTOR('',#34794,1.);
#10326=VECTOR('',#34795,1.);
#10327=VECTOR('',#34798,1.);
#10328=VECTOR('',#34803,1.);
#10329=VECTOR('',#34808,1.);
#10330=VECTOR('',#34815,0.6);
#10331=VECTOR('',#34820,1.);
#10332=VECTOR('',#34823,1.);
#10333=VECTOR('',#34826,1.);
#10334=VECTOR('',#34827,1.);
#10335=VECTOR('',#34828,1.);
#10336=VECTOR('',#34831,1.);
#10337=VECTOR('',#34832,1.);
#10338=VECTOR('',#34833,1.);
#10339=VECTOR('',#34836,1.);
#10340=VECTOR('',#34837,1.);
#10341=VECTOR('',#34838,1.);
#10342=VECTOR('',#34845,1.);
#10343=VECTOR('',#34848,1.);
#10344=VECTOR('',#34849,1.);
#10345=VECTOR('',#34850,1.);
#10346=VECTOR('',#34853,1.);
#10347=VECTOR('',#34854,1.);
#10348=VECTOR('',#34859,1.);
#10349=VECTOR('',#34860,1.);
#10350=VECTOR('',#34861,1.);
#10351=VECTOR('',#34862,1.);
#10352=VECTOR('',#34865,1.);
#10353=VECTOR('',#34866,1.);
#10354=VECTOR('',#34867,1.);
#10355=VECTOR('',#34870,1.);
#10356=VECTOR('',#34871,1.);
#10357=VECTOR('',#34872,1.);
#10358=VECTOR('',#34875,1.);
#10359=VECTOR('',#34876,1.);
#10360=VECTOR('',#34881,1.);
#10361=VECTOR('',#34882,1.);
#10362=VECTOR('',#34883,1.);
#10363=VECTOR('',#34884,1.);
#10364=VECTOR('',#34887,1.);
#10365=VECTOR('',#34888,1.);
#10366=VECTOR('',#34889,1.);
#10367=VECTOR('',#34892,1.);
#10368=VECTOR('',#34893,1.);
#10369=VECTOR('',#34894,1.);
#10370=VECTOR('',#34897,1.);
#10371=VECTOR('',#34898,1.);
#10372=VECTOR('',#34903,1.);
#10373=VECTOR('',#34904,1.);
#10374=VECTOR('',#34905,1.);
#10375=VECTOR('',#34906,1.);
#10376=VECTOR('',#34909,1.);
#10377=VECTOR('',#34910,1.);
#10378=VECTOR('',#34911,1.);
#10379=VECTOR('',#34914,1.);
#10380=VECTOR('',#34915,1.);
#10381=VECTOR('',#34916,1.);
#10382=VECTOR('',#34919,1.);
#10383=VECTOR('',#34920,1.);
#10384=VECTOR('',#34925,1.);
#10385=VECTOR('',#34926,1.);
#10386=VECTOR('',#34927,1.);
#10387=VECTOR('',#34928,1.);
#10388=VECTOR('',#34931,1.);
#10389=VECTOR('',#34932,1.);
#10390=VECTOR('',#34933,1.);
#10391=VECTOR('',#34936,1.);
#10392=VECTOR('',#34937,1.);
#10393=VECTOR('',#34938,1.);
#10394=VECTOR('',#34941,1.);
#10395=VECTOR('',#34942,1.);
#10396=VECTOR('',#34947,1.);
#10397=VECTOR('',#34948,1.);
#10398=VECTOR('',#34949,1.);
#10399=VECTOR('',#34950,1.);
#10400=VECTOR('',#34953,1.);
#10401=VECTOR('',#34954,1.);
#10402=VECTOR('',#34955,1.);
#10403=VECTOR('',#34958,1.);
#10404=VECTOR('',#34959,1.);
#10405=VECTOR('',#34960,1.);
#10406=VECTOR('',#34963,1.);
#10407=VECTOR('',#34964,1.);
#10408=VECTOR('',#34969,1.);
#10409=VECTOR('',#34970,1.);
#10410=VECTOR('',#34971,1.);
#10411=VECTOR('',#34972,1.);
#10412=VECTOR('',#34975,1.);
#10413=VECTOR('',#34976,1.);
#10414=VECTOR('',#34977,1.);
#10415=VECTOR('',#34980,1.);
#10416=VECTOR('',#34981,1.);
#10417=VECTOR('',#34982,1.);
#10418=VECTOR('',#34985,1.);
#10419=VECTOR('',#34986,1.);
#10420=VECTOR('',#34991,1.);
#10421=VECTOR('',#34992,1.);
#10422=VECTOR('',#34993,1.);
#10423=VECTOR('',#34994,1.);
#10424=VECTOR('',#34997,1.);
#10425=VECTOR('',#34998,1.);
#10426=VECTOR('',#34999,1.);
#10427=VECTOR('',#35002,1.);
#10428=VECTOR('',#35003,1.);
#10429=VECTOR('',#35004,1.);
#10430=VECTOR('',#35007,1.);
#10431=VECTOR('',#35008,1.);
#10432=VECTOR('',#35013,1.);
#10433=VECTOR('',#35014,1.);
#10434=VECTOR('',#35015,1.);
#10435=VECTOR('',#35016,1.);
#10436=VECTOR('',#35019,1.);
#10437=VECTOR('',#35020,1.);
#10438=VECTOR('',#35021,1.);
#10439=VECTOR('',#35024,1.);
#10440=VECTOR('',#35025,1.);
#10441=VECTOR('',#35026,1.);
#10442=VECTOR('',#35029,1.);
#10443=VECTOR('',#35030,1.);
#10444=VECTOR('',#35035,1.);
#10445=VECTOR('',#35036,1.);
#10446=VECTOR('',#35037,1.);
#10447=VECTOR('',#35038,1.);
#10448=VECTOR('',#35041,1.);
#10449=VECTOR('',#35042,1.);
#10450=VECTOR('',#35043,1.);
#10451=VECTOR('',#35046,1.);
#10452=VECTOR('',#35047,1.);
#10453=VECTOR('',#35048,1.);
#10454=VECTOR('',#35051,1.);
#10455=VECTOR('',#35052,1.);
#10456=VECTOR('',#35057,1.);
#10457=VECTOR('',#35058,1.);
#10458=VECTOR('',#35059,1.);
#10459=VECTOR('',#35060,1.);
#10460=VECTOR('',#35063,1.);
#10461=VECTOR('',#35064,1.);
#10462=VECTOR('',#35065,1.);
#10463=VECTOR('',#35068,1.);
#10464=VECTOR('',#35069,1.);
#10465=VECTOR('',#35070,1.);
#10466=VECTOR('',#35073,1.);
#10467=VECTOR('',#35074,1.);
#10468=VECTOR('',#35079,1.);
#10469=VECTOR('',#35080,1.);
#10470=VECTOR('',#35081,1.);
#10471=VECTOR('',#35082,1.);
#10472=VECTOR('',#35085,1.);
#10473=VECTOR('',#35086,1.);
#10474=VECTOR('',#35087,1.);
#10475=VECTOR('',#35090,1.);
#10476=VECTOR('',#35091,1.);
#10477=VECTOR('',#35092,1.);
#10478=VECTOR('',#35095,1.);
#10479=VECTOR('',#35096,1.);
#10480=VECTOR('',#35105,2.9);
#10481=VECTOR('',#35116,3.05);
#10482=VECTOR('',#35121,3.15);
#10483=VECTOR('',#35130,3.3);
#10484=VECTOR('',#35135,3.25);
#10485=VECTOR('',#35140,1.);
#10486=VECTOR('',#35143,0.25);
#10487=VECTOR('',#35148,1.25);
#10488=VECTOR('',#35151,1.);
#10489=VECTOR('',#35162,0.599999999999994);
#10490=VECTOR('',#35163,0.599999999999994);
#10491=VECTOR('',#35172,0.549999999999997);
#10492=VECTOR('',#35181,1.65000000000001);
#10493=VECTOR('',#35186,1.7);
#10494=VECTOR('',#35191,1.65000000000001);
#10495=VECTOR('',#35198,1.175);
#10496=VECTOR('',#35215,1.);
#10497=VECTOR('',#35216,1.);
#10498=VECTOR('',#35217,1.);
#10499=VECTOR('',#35218,1.);
#10500=VECTOR('',#35221,1.);
#10501=VECTOR('',#35222,1.);
#10502=VECTOR('',#35223,1.);
#10503=VECTOR('',#35226,1.);
#10504=VECTOR('',#35227,1.);
#10505=VECTOR('',#35228,1.);
#10506=VECTOR('',#35231,1.);
#10507=VECTOR('',#35232,1.);
#10508=VECTOR('',#35233,1.);
#10509=VECTOR('',#35234,1.);
#10510=VECTOR('',#35237,1.);
#10511=VECTOR('',#35238,1.);
#10512=VECTOR('',#35239,1.);
#10513=VECTOR('',#35242,1.);
#10514=VECTOR('',#35243,1.);
#10515=VECTOR('',#35244,1.);
#10516=VECTOR('',#35247,1.);
#10517=VECTOR('',#35248,1.);
#10518=VECTOR('',#35249,1.);
#10519=VECTOR('',#35250,1.);
#10520=VECTOR('',#35251,1.);
#10521=VECTOR('',#35254,1.);
#10522=VECTOR('',#35255,1.);
#10523=VECTOR('',#35256,1.);
#10524=VECTOR('',#35257,1.);
#10525=VECTOR('',#35258,1.);
#10526=VECTOR('',#35259,1.);
#10527=VECTOR('',#35260,1.);
#10528=VECTOR('',#35263,1.);
#10529=VECTOR('',#35264,1.);
#10530=VECTOR('',#35267,1.);
#10531=VECTOR('',#35268,1.);
#10532=VECTOR('',#35269,1.);
#10533=VECTOR('',#35270,1.);
#10534=VECTOR('',#35273,1.);
#10535=VECTOR('',#35274,1.);
#10536=VECTOR('',#35277,1.);
#10537=VECTOR('',#35278,1.);
#10538=VECTOR('',#35279,1.);
#10539=VECTOR('',#35280,1.);
#10540=VECTOR('',#35281,1.);
#10541=VECTOR('',#35284,1.);
#10542=VECTOR('',#35285,1.);
#10543=VECTOR('',#35286,1.);
#10544=VECTOR('',#35287,1.);
#10545=VECTOR('',#35288,1.);
#10546=VECTOR('',#35291,1.);
#10547=VECTOR('',#35292,1.);
#10548=VECTOR('',#35293,1.);
#10549=VECTOR('',#35294,1.);
#10550=VECTOR('',#35295,1.);
#10551=VECTOR('',#35298,1.);
#10552=VECTOR('',#35299,1.);
#10553=VECTOR('',#35300,1.);
#10554=VECTOR('',#35301,1.);
#10555=VECTOR('',#35304,1.);
#10556=VECTOR('',#35305,1.);
#10557=VECTOR('',#35306,1.);
#10558=VECTOR('',#35309,1.);
#10559=VECTOR('',#35310,1.);
#10560=VECTOR('',#35311,1.);
#10561=VECTOR('',#35312,1.);
#10562=VECTOR('',#35315,1.);
#10563=VECTOR('',#35316,1.);
#10564=VECTOR('',#35319,1.);
#10565=VECTOR('',#35320,1.);
#10566=VECTOR('',#35321,1.);
#10567=VECTOR('',#35324,1.);
#10568=VECTOR('',#35325,1.);
#10569=VECTOR('',#35326,1.);
#10570=VECTOR('',#35327,1.);
#10571=VECTOR('',#35328,1.);
#10572=VECTOR('',#35331,1.);
#10573=VECTOR('',#35332,1.);
#10574=VECTOR('',#35333,1.);
#10575=VECTOR('',#35334,1.);
#10576=VECTOR('',#35335,1.);
#10577=VECTOR('',#35336,1.);
#10578=VECTOR('',#35337,1.);
#10579=VECTOR('',#35340,1.);
#10580=VECTOR('',#35341,1.);
#10581=VECTOR('',#35344,1.);
#10582=VECTOR('',#35345,1.);
#10583=VECTOR('',#35346,1.);
#10584=VECTOR('',#35347,1.);
#10585=VECTOR('',#35348,1.);
#10586=VECTOR('',#35351,1.);
#10587=VECTOR('',#35352,1.);
#10588=VECTOR('',#35353,1.);
#10589=VECTOR('',#35356,1.);
#10590=VECTOR('',#35357,1.);
#10591=VECTOR('',#35360,1.);
#10592=VECTOR('',#35361,1.);
#10593=VECTOR('',#35362,1.);
#10594=VECTOR('',#35363,1.);
#10595=VECTOR('',#35366,1.);
#10596=VECTOR('',#35367,1.);
#10597=VECTOR('',#35370,1.);
#10598=VECTOR('',#35371,1.);
#10599=VECTOR('',#35374,1.);
#10600=VECTOR('',#35375,1.);
#10601=VECTOR('',#35376,1.);
#10602=VECTOR('',#35377,1.);
#10603=VECTOR('',#35378,1.);
#10604=VECTOR('',#35381,1.);
#10605=VECTOR('',#35382,1.);
#10606=VECTOR('',#35383,1.);
#10607=VECTOR('',#35384,1.);
#10608=VECTOR('',#35385,1.);
#10609=VECTOR('',#35388,1.);
#10610=VECTOR('',#35389,1.);
#10611=VECTOR('',#35390,1.);
#10612=VECTOR('',#35391,1.);
#10613=VECTOR('',#35394,1.);
#10614=VECTOR('',#35395,1.);
#10615=VECTOR('',#35396,1.);
#10616=VECTOR('',#35399,1.);
#10617=VECTOR('',#35400,1.);
#10618=VECTOR('',#35401,1.);
#10619=VECTOR('',#35402,1.);
#10620=VECTOR('',#35405,1.);
#10621=VECTOR('',#35406,1.);
#10622=VECTOR('',#35407,1.);
#10623=VECTOR('',#35410,1.);
#10624=VECTOR('',#35413,1.);
#10625=VECTOR('',#35418,1.);
#10626=VECTOR('',#35419,1.);
#10627=VECTOR('',#35420,1.);
#10628=VECTOR('',#35423,1.);
#10629=VECTOR('',#35430,1.);
#10630=VECTOR('',#35431,1.);
#10631=VECTOR('',#35432,1.);
#10632=VECTOR('',#35435,1.);
#10633=VECTOR('',#35442,1.);
#10634=VECTOR('',#35443,1.);
#10635=VECTOR('',#35444,1.);
#10636=VECTOR('',#35447,1.);
#10637=VECTOR('',#35454,1.);
#10638=VECTOR('',#35455,1.);
#10639=VECTOR('',#35458,1.);
#10640=VECTOR('',#35459,1.);
#10641=VECTOR('',#35460,1.);
#10642=VECTOR('',#35463,1.);
#10643=VECTOR('',#35468,1.);
#10644=VECTOR('',#35469,1.);
#10645=VECTOR('',#35472,1.);
#10646=VECTOR('',#35483,1.);
#10647=VECTOR('',#35484,1.);
#10648=VECTOR('',#35487,1.);
#10649=VECTOR('',#35488,1.);
#10650=VECTOR('',#35491,1.);
#10651=VECTOR('',#35492,1.);
#10652=VECTOR('',#35493,1.);
#10653=VECTOR('',#35496,1.);
#10654=VECTOR('',#35499,1.);
#10655=VECTOR('',#35500,1.);
#10656=VECTOR('',#35501,1.);
#10657=VECTOR('',#35508,1.);
#10658=VECTOR('',#35509,1.);
#10659=VECTOR('',#35514,1.);
#10660=VECTOR('',#35515,1.);
#10661=VECTOR('',#35516,1.);
#10662=VECTOR('',#35517,1.);
#10663=VECTOR('',#35520,1.);
#10664=VECTOR('',#35523,1.);
#10665=VECTOR('',#35524,1.);
#10666=VECTOR('',#35531,1.);
#10667=VECTOR('',#35532,1.);
#10668=VECTOR('',#35535,1.);
#10669=VECTOR('',#35536,1.);
#10670=VECTOR('',#35539,1.);
#10671=VECTOR('',#35544,0.925000000000001);
#10672=VECTOR('',#35551,0.875);
#10673=VECTOR('',#35554,1.);
#10674=VECTOR('',#35559,0.925000000000001);
#10675=VECTOR('',#35562,0.925000000000001);
#10676=VECTOR('',#35569,0.875);
#10677=VECTOR('',#35574,0.925000000000001);
#10678=VECTOR('',#35577,1.);
#10679=VECTOR('',#35582,0.925000000000001);
#10680=VECTOR('',#35589,0.875);
#10681=VECTOR('',#35592,0.925000000000001);
#10682=VECTOR('',#35595,0.925000000000001);
#10683=VECTOR('',#35602,0.875);
#10684=VECTOR('',#35605,0.925000000000001);
#10685=VECTOR('',#35608,0.949999999999999);
#10686=VECTOR('',#35613,0.899999999999999);
#10687=VECTOR('',#35618,0.949999999999999);
#10688=VECTOR('',#35623,0.899999999999999);
#10689=VECTOR('',#35628,1.);
#10690=VECTOR('',#35629,1.);
#10691=VECTOR('',#35630,1.);
#10692=VECTOR('',#35633,1.);
#10693=VECTOR('',#35640,1.);
#10694=VECTOR('',#35641,1.);
#10695=VECTOR('',#35642,1.);
#10696=VECTOR('',#35645,1.);
#10697=VECTOR('',#35652,1.);
#10698=VECTOR('',#35653,1.);
#10699=VECTOR('',#35656,1.);
#10700=VECTOR('',#35657,1.);
#10701=VECTOR('',#35660,1.);
#10702=VECTOR('',#35663,1.);
#10703=VECTOR('',#35670,1.);
#10704=VECTOR('',#35671,1.);
#10705=VECTOR('',#35674,1.);
#10706=VECTOR('',#35679,1.);
#10707=VECTOR('',#35680,1.);
#10708=VECTOR('',#35683,1.);
#10709=VECTOR('',#35688,1.);
#10710=VECTOR('',#35689,1.);
#10711=VECTOR('',#35692,0.949999999999999);
#10712=VECTOR('',#35695,0.949999999999999);
#10713=VECTOR('',#35698,1.);
#10714=VECTOR('',#35701,1.);
#10715=VECTOR('',#35702,1.);
#10716=VECTOR('',#35705,1.);
#10717=VECTOR('',#35708,1.);
#10718=VECTOR('',#35709,1.);
#10719=VECTOR('',#35712,1.);
#10720=VECTOR('',#35715,1.);
#10721=VECTOR('',#35718,1.);
#10722=VECTOR('',#35721,1.);
#10723=VECTOR('',#35726,1.);
#10724=VECTOR('',#35727,1.);
#10725=VECTOR('',#35730,1.);
#10726=VECTOR('',#35735,1.);
#10727=VECTOR('',#35738,1.);
#10728=VECTOR('',#35739,1.);
#10729=VECTOR('',#35742,1.);
#10730=VECTOR('',#35779,1.);
#10731=VECTOR('',#35792,0.5);
#10732=VECTOR('',#35797,0.5);
#10733=VECTOR('',#35800,0.5);
#10734=VECTOR('',#35803,0.5);
#10735=VECTOR('',#35806,0.5);
#10736=VECTOR('',#35809,0.5);
#10737=VECTOR('',#35812,0.5);
#10738=VECTOR('',#35815,0.5);
#10739=VECTOR('',#35818,0.5);
#10740=VECTOR('',#35821,0.5);
#10741=VECTOR('',#35824,0.5);
#10742=VECTOR('',#35827,0.40705);
#10743=VECTOR('',#35832,0.40705);
#10744=VECTOR('',#35835,0.40705);
#10745=VECTOR('',#35838,0.40705);
#10746=VECTOR('',#35841,0.40705);
#10747=VECTOR('',#35844,0.40705);
#10748=VECTOR('',#35847,0.40705);
#10749=VECTOR('',#35850,0.40705);
#10750=VECTOR('',#35853,0.40705);
#10751=VECTOR('',#35856,0.40705);
#10752=VECTOR('',#35859,0.40705);
#10753=VECTOR('',#35898,1.25);
#10754=VECTOR('',#35901,1.15);
#10755=VECTOR('',#35918,0.46);
#10756=VECTOR('',#35925,1.);
#10757=VECTOR('',#35926,1.);
#10758=VECTOR('',#35927,1.);
#10759=VECTOR('',#35928,1.);
#10760=VECTOR('',#35929,1.);
#10761=VECTOR('',#35930,1.);
#10762=VECTOR('',#35933,1.);
#10763=VECTOR('',#35934,1.);
#10764=VECTOR('',#35935,1.);
#10765=VECTOR('',#35938,1.);
#10766=VECTOR('',#35939,1.);
#10767=VECTOR('',#35940,1.);
#10768=VECTOR('',#35941,1.);
#10769=VECTOR('',#35944,1.);
#10770=VECTOR('',#35945,1.);
#10771=VECTOR('',#35946,1.);
#10772=VECTOR('',#35947,1.);
#10773=VECTOR('',#35950,1.);
#10774=VECTOR('',#35951,1.);
#10775=VECTOR('',#35952,1.);
#10776=VECTOR('',#35953,1.);
#10777=VECTOR('',#35954,1.);
#10778=VECTOR('',#35955,1.);
#10779=VECTOR('',#35956,1.);
#10780=VECTOR('',#35957,1.);
#10781=VECTOR('',#35960,1.);
#10782=VECTOR('',#35961,1.);
#10783=VECTOR('',#35964,1.);
#10784=VECTOR('',#35965,1.);
#10785=VECTOR('',#35966,1.);
#10786=VECTOR('',#35967,1.);
#10787=VECTOR('',#35970,1.);
#10788=VECTOR('',#35971,1.);
#10789=VECTOR('',#35972,1.);
#10790=VECTOR('',#35975,1.);
#10791=VECTOR('',#35976,1.);
#10792=VECTOR('',#35977,1.);
#10793=VECTOR('',#35980,1.);
#10794=VECTOR('',#35981,1.);
#10795=VECTOR('',#35982,1.);
#10796=VECTOR('',#35983,1.);
#10797=VECTOR('',#35984,1.);
#10798=VECTOR('',#35985,1.);
#10799=VECTOR('',#35988,1.);
#10800=VECTOR('',#35989,1.);
#10801=VECTOR('',#35990,1.);
#10802=VECTOR('',#35993,1.);
#10803=VECTOR('',#35994,1.);
#10804=VECTOR('',#35995,1.);
#10805=VECTOR('',#35998,1.);
#10806=VECTOR('',#36001,1.);
#10807=VECTOR('',#36002,1.);
#10808=VECTOR('',#36005,1.);
#10809=VECTOR('',#36006,1.);
#10810=VECTOR('',#36007,1.);
#10811=VECTOR('',#36008,1.);
#10812=VECTOR('',#36011,1.);
#10813=VECTOR('',#36012,1.);
#10814=VECTOR('',#36013,1.);
#10815=VECTOR('',#36016,1.);
#10816=VECTOR('',#36017,1.);
#10817=VECTOR('',#36020,1.);
#10818=VECTOR('',#36021,1.);
#10819=VECTOR('',#36024,1.);
#10820=VECTOR('',#36025,1.);
#10821=VECTOR('',#36028,1.);
#10822=VECTOR('',#36029,1.);
#10823=VECTOR('',#36030,1.);
#10824=VECTOR('',#36031,1.);
#10825=VECTOR('',#36034,1.);
#10826=VECTOR('',#36035,1.);
#10827=VECTOR('',#36036,1.);
#10828=VECTOR('',#36041,1.);
#10829=VECTOR('',#36042,1.);
#10830=VECTOR('',#36043,1.);
#10831=VECTOR('',#36046,1.);
#10832=VECTOR('',#36047,1.);
#10833=VECTOR('',#36048,1.);
#10834=VECTOR('',#36051,1.);
#10835=VECTOR('',#36052,1.);
#10836=VECTOR('',#36053,1.);
#10837=VECTOR('',#36056,1.);
#10838=VECTOR('',#36057,1.);
#10839=VECTOR('',#36058,1.);
#10840=VECTOR('',#36061,1.);
#10841=VECTOR('',#36062,1.);
#10842=VECTOR('',#36063,1.);
#10843=VECTOR('',#36066,1.);
#10844=VECTOR('',#36069,1.);
#10845=VECTOR('',#36070,1.);
#10846=VECTOR('',#36073,1.);
#10847=VECTOR('',#36074,1.);
#10848=VECTOR('',#36077,1.);
#10849=VECTOR('',#36078,1.);
#10850=VECTOR('',#36079,1.);
#10851=VECTOR('',#36082,1.);
#10852=VECTOR('',#36083,1.);
#10853=VECTOR('',#36086,1.);
#10854=VECTOR('',#36089,1.);
#10855=VECTOR('',#36090,1.);
#10856=VECTOR('',#36093,1.);
#10857=VECTOR('',#36094,1.);
#10858=VECTOR('',#36095,1.);
#10859=VECTOR('',#36098,1.);
#10860=VECTOR('',#36099,1.);
#10861=VECTOR('',#36102,1.);
#10862=VECTOR('',#36103,1.);
#10863=VECTOR('',#36106,1.);
#10864=VECTOR('',#36113,1.);
#10865=VECTOR('',#36120,1.);
#10866=VECTOR('',#36127,0.8);
#10867=VECTOR('',#36132,0.8);
#10868=VECTOR('',#36135,0.8);
#10869=VECTOR('',#36138,0.8);
#10870=VECTOR('',#36141,0.8);
#10871=VECTOR('',#36144,0.8);
#10872=VECTOR('',#36147,0.8);
#10873=VECTOR('',#36150,0.8);
#10874=VECTOR('',#36153,0.8);
#10875=VECTOR('',#36156,0.8);
#10876=VECTOR('',#36159,0.8);
#10877=VECTOR('',#36162,0.8);
#10878=VECTOR('',#36165,0.8);
#10879=VECTOR('',#36168,0.8);
#10880=VECTOR('',#36171,0.8);
#10881=VECTOR('',#36174,0.8);
#10882=VECTOR('',#36177,0.8);
#10883=VECTOR('',#36180,0.8);
#10884=VECTOR('',#36183,0.8);
#10885=VECTOR('',#36186,0.8);
#10886=VECTOR('',#36189,0.8);
#10887=VECTOR('',#36192,0.8);
#10888=VECTOR('',#36195,0.8);
#10889=VECTOR('',#36198,0.8);
#10890=VECTOR('',#36201,0.8);
#10891=VECTOR('',#36204,0.8);
#10892=VECTOR('',#36207,0.8);
#10893=VECTOR('',#36210,0.8);
#10894=VECTOR('',#36213,0.8);
#10895=VECTOR('',#36216,0.8);
#10896=VECTOR('',#36219,0.8);
#10897=VECTOR('',#36222,0.8);
#10898=VECTOR('',#36225,0.8);
#10899=VECTOR('',#36228,0.8);
#10900=VECTOR('',#36231,0.8);
#10901=VECTOR('',#36234,0.8);
#10902=VECTOR('',#36237,0.8);
#10903=VECTOR('',#36240,0.8);
#10904=VECTOR('',#36243,0.8);
#10905=VECTOR('',#36246,0.8);
#10906=VECTOR('',#36249,0.8);
#10907=VECTOR('',#36252,0.8);
#10908=VECTOR('',#36255,0.8);
#10909=VECTOR('',#36258,0.8);
#10910=VECTOR('',#36261,0.8);
#10911=VECTOR('',#36264,0.8);
#10912=VECTOR('',#36267,0.8);
#10913=VECTOR('',#36270,0.8);
#10914=VECTOR('',#36273,0.8);
#10915=VECTOR('',#36276,0.8);
#10916=VECTOR('',#36279,0.8);
#10917=VECTOR('',#36282,0.8);
#10918=VECTOR('',#36285,0.8);
#10919=VECTOR('',#36288,0.8);
#10920=VECTOR('',#36291,0.8);
#10921=VECTOR('',#36294,0.8);
#10922=VECTOR('',#36297,0.8);
#10923=VECTOR('',#36300,0.8);
#10924=VECTOR('',#36303,0.8);
#10925=VECTOR('',#36306,0.8);
#10926=VECTOR('',#36311,0.6767);
#10927=VECTOR('',#36316,0.6767);
#10928=VECTOR('',#36319,0.6767);
#10929=VECTOR('',#36322,0.6767);
#10930=VECTOR('',#36325,0.6767);
#10931=VECTOR('',#36328,0.6767);
#10932=VECTOR('',#36331,0.6767);
#10933=VECTOR('',#36334,0.6767);
#10934=VECTOR('',#36337,0.6767);
#10935=VECTOR('',#36340,0.6767);
#10936=VECTOR('',#36343,0.6767);
#10937=VECTOR('',#36346,0.6767);
#10938=VECTOR('',#36349,0.6767);
#10939=VECTOR('',#36352,0.6767);
#10940=VECTOR('',#36355,0.6767);
#10941=VECTOR('',#36358,0.6767);
#10942=VECTOR('',#36361,0.6767);
#10943=VECTOR('',#36364,0.6767);
#10944=VECTOR('',#36367,0.6767);
#10945=VECTOR('',#36370,0.6767);
#10946=VECTOR('',#36373,0.6767);
#10947=VECTOR('',#36376,0.6767);
#10948=VECTOR('',#36379,0.6767);
#10949=VECTOR('',#36382,0.6767);
#10950=VECTOR('',#36385,0.6767);
#10951=VECTOR('',#36388,0.6767);
#10952=VECTOR('',#36391,0.6767);
#10953=VECTOR('',#36394,0.6767);
#10954=VECTOR('',#36397,0.6767);
#10955=VECTOR('',#36400,0.6767);
#10956=VECTOR('',#36403,0.6767);
#10957=VECTOR('',#36406,0.6767);
#10958=VECTOR('',#36409,0.6767);
#10959=VECTOR('',#36412,0.6767);
#10960=VECTOR('',#36415,0.6767);
#10961=VECTOR('',#36418,0.6767);
#10962=VECTOR('',#36421,0.6767);
#10963=VECTOR('',#36424,0.6767);
#10964=VECTOR('',#36427,0.6767);
#10965=VECTOR('',#36430,0.6767);
#10966=VECTOR('',#36433,0.6767);
#10967=VECTOR('',#36436,0.6767);
#10968=VECTOR('',#36439,0.6767);
#10969=VECTOR('',#36442,0.6767);
#10970=VECTOR('',#36445,0.6767);
#10971=VECTOR('',#36448,0.6767);
#10972=VECTOR('',#36451,0.6767);
#10973=VECTOR('',#36454,0.6767);
#10974=VECTOR('',#36457,0.6767);
#10975=VECTOR('',#36460,0.6767);
#10976=VECTOR('',#36463,0.6767);
#10977=VECTOR('',#36466,0.6767);
#10978=VECTOR('',#36469,0.6767);
#10979=VECTOR('',#36472,0.6767);
#10980=VECTOR('',#36475,0.6767);
#10981=VECTOR('',#36478,0.6767);
#10982=VECTOR('',#36481,0.6767);
#10983=VECTOR('',#36484,0.6767);
#10984=VECTOR('',#36487,0.6767);
#10985=VECTOR('',#36488,1.);
#10986=VECTOR('',#36489,1.);
#10987=VECTOR('',#36490,1.);
#10988=VECTOR('',#36491,1.);
#10989=VECTOR('',#36492,1.);
#10990=VECTOR('',#36493,1.);
#10991=VECTOR('',#36494,1.);
#10992=VECTOR('',#36495,1.);
#10993=VECTOR('',#36496,1.);
#10994=VECTOR('',#36497,1.);
#10995=VECTOR('',#36498,1.);
#10996=VECTOR('',#36499,1.);
#10997=VECTOR('',#36500,1.);
#10998=VECTOR('',#36501,1.);
#10999=VECTOR('',#36502,1.);
#11000=VECTOR('',#36503,1.);
#11001=VECTOR('',#36504,1.);
#11002=VECTOR('',#36505,1.);
#11003=VECTOR('',#36506,1.);
#11004=VECTOR('',#36507,1.);
#11005=VECTOR('',#36508,1.);
#11006=VECTOR('',#36509,1.);
#11007=VECTOR('',#36510,1.);
#11008=VECTOR('',#36511,1.);
#11009=VECTOR('',#36512,1.);
#11010=VECTOR('',#36513,1.);
#11011=VECTOR('',#36514,1.);
#11012=VECTOR('',#36515,1.);
#11013=VECTOR('',#36516,1.);
#11014=VECTOR('',#36517,1.);
#11015=VECTOR('',#36518,1.);
#11016=VECTOR('',#36519,1.);
#11017=VECTOR('',#36520,1.);
#11018=VECTOR('',#36525,1.);
#11019=VECTOR('',#36526,1.);
#11020=VECTOR('',#36527,1.);
#11021=VECTOR('',#36528,1.);
#11022=VECTOR('',#36531,1.);
#11023=VECTOR('',#36532,1.);
#11024=VECTOR('',#36533,1.);
#11025=VECTOR('',#36536,1.);
#11026=VECTOR('',#36537,1.);
#11027=VECTOR('',#36538,1.);
#11028=VECTOR('',#36541,1.);
#11029=VECTOR('',#36542,1.);
#11030=VECTOR('',#36545,1.);
#11031=VECTOR('',#36546,1.);
#11032=VECTOR('',#36547,1.);
#11033=VECTOR('',#36548,1.);
#11034=VECTOR('',#36549,1.);
#11035=VECTOR('',#36550,1.);
#11036=VECTOR('',#36551,1.);
#11037=VECTOR('',#36552,1.);
#11038=VECTOR('',#36553,1.);
#11039=VECTOR('',#36554,1.);
#11040=VECTOR('',#36555,1.);
#11041=VECTOR('',#36556,1.);
#11042=VECTOR('',#36557,1.);
#11043=VECTOR('',#36558,1.);
#11044=VECTOR('',#36559,1.);
#11045=VECTOR('',#36560,1.);
#11046=VECTOR('',#36561,1.);
#11047=VECTOR('',#36562,1.);
#11048=VECTOR('',#36563,1.);
#11049=VECTOR('',#36564,1.);
#11050=VECTOR('',#36565,1.);
#11051=VECTOR('',#36566,1.);
#11052=VECTOR('',#36567,1.);
#11053=VECTOR('',#36568,1.);
#11054=VECTOR('',#36569,1.);
#11055=VECTOR('',#36570,1.);
#11056=VECTOR('',#36571,1.);
#11057=VECTOR('',#36572,1.);
#11058=VECTOR('',#36573,1.);
#11059=VECTOR('',#36574,1.);
#11060=VECTOR('',#36575,1.);
#11061=VECTOR('',#36576,1.);
#11062=VECTOR('',#36577,1.);
#11063=VECTOR('',#36614,1.);
#11064=VECTOR('',#36615,1.);
#11065=VECTOR('',#36616,1.);
#11066=VECTOR('',#36617,1.);
#11067=VECTOR('',#36618,1.);
#11068=VECTOR('',#36619,1.);
#11069=VECTOR('',#36624,1.28782032302755);
#11070=VECTOR('',#36629,1.);
#11071=VECTOR('',#36630,1.);
#11072=VECTOR('',#36633,1.);
#11073=VECTOR('',#36636,1.);
#11074=VECTOR('',#36639,1.);
#11075=VECTOR('',#36642,1.);
#11076=VECTOR('',#36653,0.75);
#11077=VECTOR('',#36660,0.845);
#11078=VECTOR('',#36667,0.805);
#11079=VECTOR('',#36676,0.845);
#11080=VECTOR('',#36683,1.28782032302755);
#11081=VECTOR('',#36686,1.);
#11082=VECTOR('',#36687,1.);
#11083=VECTOR('',#36690,1.);
#11084=VECTOR('',#36693,1.);
#11085=VECTOR('',#36696,1.28782032302755);
#11086=VECTOR('',#36699,1.);
#11087=VECTOR('',#36702,1.);
#11088=VECTOR('',#36711,0.85);
#11089=VECTOR('',#36722,1.5);
#11090=VECTOR('',#36727,1.48);
#11091=VECTOR('',#36734,0.87);
#11092=VECTOR('',#36741,1.18535533905933);
#11093=VECTOR('',#36748,1.30000000000001);
#11094=VECTOR('',#36757,1.36464466094067);
#11095=VECTOR('',#36764,1.40000000000001);
#11096=VECTOR('',#36771,0.57);
#11097=VECTOR('',#36778,0.52);
#11098=VECTOR('',#36781,1.);
#11099=VECTOR('',#36782,1.);
#11100=VECTOR('',#36785,1.);
#11101=VECTOR('',#36790,0.57);
#11102=VECTOR('',#36793,1.);
#11103=VECTOR('',#36794,1.);
#11104=VECTOR('',#36797,1.);
#11105=VECTOR('',#36804,1.35000000000004);
#11106=VECTOR('',#36811,1.40000000000001);
#11107=VECTOR('',#36824,1.30000000000003);
#11108=VECTOR('',#36831,1.40000000000001);
#11109=VECTOR('',#36842,1.3);
#11110=VECTOR('',#36849,1.40000000000001);
#11111=VECTOR('',#36860,1.30000000000003);
#11112=VECTOR('',#36867,1.);
#11113=VECTOR('',#36868,1.);
#11114=VECTOR('',#36869,1.);
#11115=VECTOR('',#36870,1.);
#11116=VECTOR('',#36871,1.);
#11117=VECTOR('',#36872,1.);
#11118=VECTOR('',#36877,1.54999999999999);
#11119=VECTOR('',#36882,1.60000000000001);
#11120=VECTOR('',#36887,1.54999999999999);
#11121=VECTOR('',#36894,0.999999999999985);
#11122=VECTOR('',#36897,1.);
#11123=VECTOR('',#36898,1.);
#11124=VECTOR('',#36901,1.);
#11125=VECTOR('',#36902,1.);
#11126=VECTOR('',#36905,1.);
#11127=VECTOR('',#36908,1.);
#11128=VECTOR('',#36913,1.);
#11129=VECTOR('',#36918,1.);
#11130=VECTOR('',#36921,1.);
#11131=VECTOR('',#36922,1.);
#11132=VECTOR('',#36933,0.925000000000001);
#11133=VECTOR('',#36938,1.);
#11134=VECTOR('',#36939,1.);
#11135=VECTOR('',#36940,1.);
#11136=VECTOR('',#36941,1.);
#11137=VECTOR('',#36964,0.875);
#11138=VECTOR('',#36969,0.925000000000001);
#11139=VECTOR('',#36974,0.875);
#11140=VECTOR('',#36979,0.925000000000001);
#11141=VECTOR('',#36984,0.875);
#11142=VECTOR('',#36989,0.925000000000001);
#11143=VECTOR('',#36994,0.875);
#11144=VECTOR('',#36999,0.925);
#11145=VECTOR('',#37004,0.875);
#11146=VECTOR('',#37009,1.35);
#11147=VECTOR('',#37014,1.3);
#11148=VECTOR('',#37019,1.35);
#11149=VECTOR('',#37024,1.3);
#11150=VECTOR('',#37031,0.925000000000001);
#11151=VECTOR('',#37036,1.);
#11152=VECTOR('',#37037,1.);
#11153=VECTOR('',#37038,1.);
#11154=VECTOR('',#37039,1.);
#11155=VECTOR('',#37064,0.875);
#11156=VECTOR('',#37067,0.925000000000001);
#11157=VECTOR('',#37074,0.875);
#11158=VECTOR('',#37077,0.925000000000001);
#11159=VECTOR('',#37084,0.875);
#11160=VECTOR('',#37087,0.925000000000001);
#11161=VECTOR('',#37094,0.875);
#11162=VECTOR('',#37097,0.925);
#11163=VECTOR('',#37104,0.875);
#11164=VECTOR('',#37107,1.);
#11165=VECTOR('',#37108,1.);
#11166=VECTOR('',#37109,1.);
#11167=VECTOR('',#37112,1.);
#11168=VECTOR('',#37119,1.);
#11169=VECTOR('',#37120,1.);
#11170=VECTOR('',#37121,1.);
#11171=VECTOR('',#37124,1.);
#11172=VECTOR('',#37131,1.);
#11173=VECTOR('',#37132,1.);
#11174=VECTOR('',#37135,1.);
#11175=VECTOR('',#37142,1.);
#11176=VECTOR('',#37143,1.);
#11177=VECTOR('',#37144,1.);
#11178=VECTOR('',#37153,1.);
#11179=VECTOR('',#37158,1.);
#11180=VECTOR('',#37159,1.);
#11181=VECTOR('',#37166,1.);
#11182=VECTOR('',#37169,1.);
#11183=VECTOR('',#37172,1.);
#11184=VECTOR('',#37175,1.);
#11185=VECTOR('',#37180,1.35);
#11186=VECTOR('',#37187,1.3);
#11187=VECTOR('',#37190,1.35);
#11188=VECTOR('',#37197,1.3);
#11189=VECTOR('',#37200,1.35);
#11190=VECTOR('',#37207,1.3);
#11191=VECTOR('',#37210,1.35);
#11192=VECTOR('',#37215,1.3);
#11193=VECTOR('',#37220,1.35);
#11194=VECTOR('',#37227,1.3);
#11195=VECTOR('',#37230,1.35);
#11196=VECTOR('',#37235,1.3);
#11197=VECTOR('',#37240,1.35);
#11198=VECTOR('',#37247,1.3);
#11199=VECTOR('',#37250,1.35);
#11200=VECTOR('',#37255,1.3);
#11201=VECTOR('',#37260,1.35);
#11202=VECTOR('',#37267,1.3);
#11203=VECTOR('',#37272,0.925000000000001);
#11204=VECTOR('',#37275,1.);
#11205=VECTOR('',#37276,1.);
#11206=VECTOR('',#37277,1.);
#11207=VECTOR('',#37278,1.);
#11208=VECTOR('',#37301,0.925000000000001);
#11209=VECTOR('',#37304,0.925000000000001);
#11210=VECTOR('',#37307,0.925000000000001);
#11211=VECTOR('',#37310,0.925);
#11212=VECTOR('',#37313,1.35);
#11213=VECTOR('',#37318,1.3);
#11214=VECTOR('',#37325,0.925000000000001);
#11215=VECTOR('',#37328,1.);
#11216=VECTOR('',#37329,1.);
#11217=VECTOR('',#37330,1.);
#11218=VECTOR('',#37331,1.);
#11219=VECTOR('',#37354,0.925000000000001);
#11220=VECTOR('',#37357,0.925000000000001);
#11221=VECTOR('',#37360,0.925000000000001);
#11222=VECTOR('',#37363,0.925);
#11223=VECTOR('',#37366,1.);
#11224=VECTOR('',#37367,1.);
#11225=VECTOR('',#37370,1.);
#11226=VECTOR('',#37375,1.);
#11227=VECTOR('',#37376,1.);
#11228=VECTOR('',#37379,1.);
#11229=VECTOR('',#37384,1.);
#11230=VECTOR('',#37387,1.);
#11231=VECTOR('',#37392,1.);
#11232=VECTOR('',#37393,1.);
#11233=VECTOR('',#37400,1.);
#11234=VECTOR('',#37405,1.);
#11235=VECTOR('',#37406,1.);
#11236=VECTOR('',#37413,1.35);
#11237=VECTOR('',#37416,1.35);
#11238=VECTOR('',#37419,1.35);
#11239=VECTOR('',#37422,1.35);
#11240=VECTOR('',#37425,1.35);
#11241=VECTOR('',#37428,1.35);
#11242=VECTOR('',#37431,1.35);
#11243=VECTOR('',#37434,1.35);
#11244=VECTOR('',#37437,1.35);
#11245=VECTOR('',#37440,1.35);
#11246=VECTOR('',#37443,1.35);
#11247=VECTOR('',#37446,1.35);
#11248=VECTOR('',#37449,1.);
#11249=VECTOR('',#37452,1.);
#11250=VECTOR('',#37457,1.);
#11251=VECTOR('',#37458,1.);
#11252=VECTOR('',#37459,1.);
#11253=VECTOR('',#37462,1.);
#11254=VECTOR('',#37469,1.);
#11255=VECTOR('',#37470,1.);
#11256=VECTOR('',#37473,1.);
#11257=VECTOR('',#37478,1.);
#11258=VECTOR('',#37479,1.);
#11259=VECTOR('',#37482,1.);
#11260=VECTOR('',#37487,1.);
#11261=VECTOR('',#37490,1.);
#11262=VECTOR('',#37495,1.);
#11263=VECTOR('',#37498,1.);
#11264=VECTOR('',#37501,1.);
#11265=VECTOR('',#37504,1.);
#11266=VECTOR('',#37507,1.);
#11267=VECTOR('',#37510,1.);
#11268=VECTOR('',#37513,1.);
#11269=VECTOR('',#37514,1.);
#11270=VECTOR('',#37517,1.);
#11271=VECTOR('',#37522,1.);
#11272=VECTOR('',#37525,1.);
#11273=VECTOR('',#37528,1.);
#11274=VECTOR('',#37531,1.);
#11275=VECTOR('',#37536,1.);
#11276=VECTOR('',#37539,1.);
#11277=VECTOR('',#37544,1.);
#11278=VERTEX_POINT('',#37680);
#11279=VERTEX_POINT('',#37681);
#11280=VERTEX_POINT('',#37683);
#11281=VERTEX_POINT('',#37685);
#11282=VERTEX_POINT('',#37687);
#11283=VERTEX_POINT('',#37691);
#11284=VERTEX_POINT('',#37693);
#11285=VERTEX_POINT('',#37695);
#11286=VERTEX_POINT('',#37697);
#11287=VERTEX_POINT('',#37701);
#11288=VERTEX_POINT('',#37705);
#11289=VERTEX_POINT('',#37709);
#11290=VERTEX_POINT('',#37713);
#11291=VERTEX_POINT('',#37715);
#11292=VERTEX_POINT('',#37717);
#11293=VERTEX_POINT('',#37721);
#11294=VERTEX_POINT('',#37723);
#11295=VERTEX_POINT('',#37725);
#11296=VERTEX_POINT('',#37727);
#11297=VERTEX_POINT('',#37729);
#11298=VERTEX_POINT('',#37733);
#11299=VERTEX_POINT('',#37734);
#11300=VERTEX_POINT('',#37736);
#11301=VERTEX_POINT('',#37738);
#11302=VERTEX_POINT('',#37740);
#11303=VERTEX_POINT('',#37744);
#11304=VERTEX_POINT('',#37746);
#11305=VERTEX_POINT('',#37750);
#11306=VERTEX_POINT('',#37761);
#11307=VERTEX_POINT('',#37766);
#11308=VERTEX_POINT('',#37768);
#11309=VERTEX_POINT('',#37772);
#11310=VERTEX_POINT('',#37773);
#11311=VERTEX_POINT('',#37775);
#11312=VERTEX_POINT('',#37777);
#11313=VERTEX_POINT('',#37780);
#11314=VERTEX_POINT('',#37782);
#11315=VERTEX_POINT('',#37784);
#11316=VERTEX_POINT('',#37787);
#11317=VERTEX_POINT('',#37791);
#11318=VERTEX_POINT('',#37795);
#11319=VERTEX_POINT('',#37799);
#11320=VERTEX_POINT('',#37803);
#11321=VERTEX_POINT('',#37807);
#11322=VERTEX_POINT('',#37811);
#11323=VERTEX_POINT('',#37815);
#11324=VERTEX_POINT('',#37819);
#11325=VERTEX_POINT('',#37820);
#11326=VERTEX_POINT('',#37822);
#11327=VERTEX_POINT('',#37824);
#11328=VERTEX_POINT('',#37827);
#11329=VERTEX_POINT('',#37829);
#11330=VERTEX_POINT('',#37831);
#11331=VERTEX_POINT('',#37840);
#11332=VERTEX_POINT('',#37842);
#11333=VERTEX_POINT('',#37846);
#11334=VERTEX_POINT('',#37847);
#11335=VERTEX_POINT('',#37849);
#11336=VERTEX_POINT('',#37851);
#11337=VERTEX_POINT('',#37854);
#11338=VERTEX_POINT('',#37856);
#11339=VERTEX_POINT('',#37858);
#11340=VERTEX_POINT('',#37861);
#11341=VERTEX_POINT('',#37865);
#11342=VERTEX_POINT('',#37869);
#11343=VERTEX_POINT('',#37873);
#11344=VERTEX_POINT('',#37877);
#11345=VERTEX_POINT('',#37881);
#11346=VERTEX_POINT('',#37885);
#11347=VERTEX_POINT('',#37889);
#11348=VERTEX_POINT('',#37890);
#11349=VERTEX_POINT('',#37892);
#11350=VERTEX_POINT('',#37894);
#11351=VERTEX_POINT('',#37896);
#11352=VERTEX_POINT('',#37935);
#11353=VERTEX_POINT('',#37936);
#11354=VERTEX_POINT('',#37938);
#11355=VERTEX_POINT('',#37948);
#11356=VERTEX_POINT('',#38008);
#11357=VERTEX_POINT('',#38010);
#11358=VERTEX_POINT('',#38012);
#11359=VERTEX_POINT('',#38014);
#11360=VERTEX_POINT('',#38016);
#11361=VERTEX_POINT('',#38018);
#11362=VERTEX_POINT('',#38023);
#11363=VERTEX_POINT('',#38034);
#11364=VERTEX_POINT('',#38041);
#11365=VERTEX_POINT('',#38043);
#11366=VERTEX_POINT('',#38045);
#11367=VERTEX_POINT('',#38050);
#11368=VERTEX_POINT('',#38088);
#11369=VERTEX_POINT('',#38095);
#11370=VERTEX_POINT('',#38099);
#11371=VERTEX_POINT('',#38100);
#11372=VERTEX_POINT('',#38102);
#11373=VERTEX_POINT('',#38104);
#11374=VERTEX_POINT('',#38107);
#11375=VERTEX_POINT('',#38109);
#11376=VERTEX_POINT('',#38111);
#11377=VERTEX_POINT('',#38120);
#11378=VERTEX_POINT('',#38121);
#11379=VERTEX_POINT('',#38123);
#11380=VERTEX_POINT('',#38125);
#11381=VERTEX_POINT('',#38129);
#11382=VERTEX_POINT('',#38134);
#11383=VERTEX_POINT('',#38138);
#11384=VERTEX_POINT('',#38140);
#11385=VERTEX_POINT('',#38144);
#11386=VERTEX_POINT('',#38149);
#11387=VERTEX_POINT('',#38153);
#11388=VERTEX_POINT('',#38154);
#11389=VERTEX_POINT('',#38163);
#11390=VERTEX_POINT('',#38165);
#11391=VERTEX_POINT('',#38171);
#11392=VERTEX_POINT('',#38173);
#11393=VERTEX_POINT('',#38178);
#11394=VERTEX_POINT('',#38189);
#11395=VERTEX_POINT('',#38194);
#11396=VERTEX_POINT('',#38196);
#11397=VERTEX_POINT('',#38201);
#11398=VERTEX_POINT('',#38213);
#11399=VERTEX_POINT('',#38218);
#11400=VERTEX_POINT('',#38220);
#11401=VERTEX_POINT('',#38224);
#11402=VERTEX_POINT('',#38225);
#11403=VERTEX_POINT('',#38227);
#11404=VERTEX_POINT('',#38229);
#11405=VERTEX_POINT('',#38231);
#11406=VERTEX_POINT('',#38233);
#11407=VERTEX_POINT('',#38235);
#11408=VERTEX_POINT('',#38237);
#11409=VERTEX_POINT('',#38241);
#11410=VERTEX_POINT('',#38243);
#11411=VERTEX_POINT('',#38247);
#11412=VERTEX_POINT('',#38252);
#11413=VERTEX_POINT('',#38256);
#11414=VERTEX_POINT('',#38260);
#11415=VERTEX_POINT('',#38261);
#11416=VERTEX_POINT('',#38266);
#11417=VERTEX_POINT('',#38271);
#11418=VERTEX_POINT('',#38283);
#11419=VERTEX_POINT('',#38284);
#11420=VERTEX_POINT('',#38288);
#11421=VERTEX_POINT('',#38292);
#11422=VERTEX_POINT('',#38296);
#11423=VERTEX_POINT('',#38300);
#11424=VERTEX_POINT('',#38304);
#11425=VERTEX_POINT('',#38308);
#11426=VERTEX_POINT('',#38312);
#11427=VERTEX_POINT('',#38316);
#11428=VERTEX_POINT('',#38323);
#11429=VERTEX_POINT('',#38324);
#11430=VERTEX_POINT('',#38326);
#11431=VERTEX_POINT('',#38328);
#11432=VERTEX_POINT('',#38330);
#11433=VERTEX_POINT('',#38332);
#11434=VERTEX_POINT('',#38334);
#11435=VERTEX_POINT('',#38336);
#11436=VERTEX_POINT('',#38339);
#11437=VERTEX_POINT('',#38340);
#11438=VERTEX_POINT('',#38344);
#11439=VERTEX_POINT('',#38348);
#11440=VERTEX_POINT('',#38352);
#11441=VERTEX_POINT('',#38356);
#11442=VERTEX_POINT('',#38360);
#11443=VERTEX_POINT('',#38364);
#11444=VERTEX_POINT('',#38368);
#11445=VERTEX_POINT('',#38372);
#11446=VERTEX_POINT('',#38376);
#11447=VERTEX_POINT('',#38380);
#11448=VERTEX_POINT('',#38384);
#11449=VERTEX_POINT('',#38391);
#11450=VERTEX_POINT('',#38392);
#11451=VERTEX_POINT('',#38394);
#11452=VERTEX_POINT('',#38396);
#11453=VERTEX_POINT('',#38398);
#11454=VERTEX_POINT('',#38402);
#11455=VERTEX_POINT('',#38406);
#11456=VERTEX_POINT('',#38410);
#11457=VERTEX_POINT('',#38414);
#11458=VERTEX_POINT('',#38418);
#11459=VERTEX_POINT('',#38422);
#11460=VERTEX_POINT('',#38426);
#11461=VERTEX_POINT('',#38430);
#11462=VERTEX_POINT('',#38432);
#11463=VERTEX_POINT('',#38436);
#11464=VERTEX_POINT('',#38440);
#11465=VERTEX_POINT('',#38444);
#11466=VERTEX_POINT('',#38448);
#11467=VERTEX_POINT('',#38452);
#11468=VERTEX_POINT('',#38456);
#11469=VERTEX_POINT('',#38460);
#11470=VERTEX_POINT('',#38464);
#11471=VERTEX_POINT('',#38471);
#11472=VERTEX_POINT('',#38472);
#11473=VERTEX_POINT('',#38474);
#11474=VERTEX_POINT('',#38476);
#11475=VERTEX_POINT('',#38478);
#11476=VERTEX_POINT('',#38480);
#11477=VERTEX_POINT('',#38482);
#11478=VERTEX_POINT('',#38484);
#11479=VERTEX_POINT('',#38486);
#11480=VERTEX_POINT('',#38488);
#11481=VERTEX_POINT('',#38492);
#11482=VERTEX_POINT('',#38493);
#11483=VERTEX_POINT('',#38495);
#11484=VERTEX_POINT('',#38497);
#11485=VERTEX_POINT('',#38499);
#11486=VERTEX_POINT('',#38501);
#11487=VERTEX_POINT('',#38503);
#11488=VERTEX_POINT('',#38505);
#11489=VERTEX_POINT('',#38509);
#11490=VERTEX_POINT('',#38511);
#11491=VERTEX_POINT('',#38513);
#11492=VERTEX_POINT('',#38560);
#11493=VERTEX_POINT('',#38562);
#11494=VERTEX_POINT('',#38616);
#11495=VERTEX_POINT('',#38618);
#11496=VERTEX_POINT('',#38620);
#11497=VERTEX_POINT('',#38625);
#11498=VERTEX_POINT('',#38657);
#11499=VERTEX_POINT('',#38664);
#11500=VERTEX_POINT('',#38666);
#11501=VERTEX_POINT('',#38668);
#11502=VERTEX_POINT('',#38711);
#11503=VERTEX_POINT('',#38713);
#11504=VERTEX_POINT('',#38766);
#11505=VERTEX_POINT('',#38768);
#11506=VERTEX_POINT('',#38770);
#11507=VERTEX_POINT('',#38775);
#11508=VERTEX_POINT('',#38813);
#11509=VERTEX_POINT('',#38820);
#11510=VERTEX_POINT('',#38822);
#11511=VERTEX_POINT('',#38826);
#11512=VERTEX_POINT('',#38830);
#11513=VERTEX_POINT('',#38839);
#11514=VERTEX_POINT('',#38843);
#11515=VERTEX_POINT('',#38849);
#11516=VERTEX_POINT('',#38853);
#11517=VERTEX_POINT('',#38857);
#11518=VERTEX_POINT('',#38859);
#11519=VERTEX_POINT('',#38864);
#11520=VERTEX_POINT('',#38875);
#11521=VERTEX_POINT('',#38891);
#11522=VERTEX_POINT('',#38897);
#11523=VERTEX_POINT('',#38902);
#11524=VERTEX_POINT('',#38907);
#11525=VERTEX_POINT('',#38909);
#11526=VERTEX_POINT('',#38914);
#11527=VERTEX_POINT('',#38925);
#11528=VERTEX_POINT('',#38938);
#11529=VERTEX_POINT('',#38945);
#11530=VERTEX_POINT('',#38950);
#11531=VERTEX_POINT('',#38955);
#11532=VERTEX_POINT('',#38959);
#11533=VERTEX_POINT('',#38961);
#11534=VERTEX_POINT('',#38963);
#11535=VERTEX_POINT('',#38965);
#11536=VERTEX_POINT('',#38967);
#11537=VERTEX_POINT('',#39093);
#11538=VERTEX_POINT('',#39097);
#11539=VERTEX_POINT('',#39115);
#11540=VERTEX_POINT('',#39120);
#11541=VERTEX_POINT('',#39131);
#11542=VERTEX_POINT('',#39148);
#11543=VERTEX_POINT('',#39154);
#11544=VERTEX_POINT('',#39163);
#11545=VERTEX_POINT('',#39168);
#11546=VERTEX_POINT('',#39179);
#11547=VERTEX_POINT('',#39198);
#11548=VERTEX_POINT('',#39205);
#11549=VERTEX_POINT('',#39469);
#11550=VERTEX_POINT('',#39471);
#11551=VERTEX_POINT('',#39473);
#11552=VERTEX_POINT('',#39516);
#11553=VERTEX_POINT('',#39518);
#11554=VERTEX_POINT('',#39571);
#11555=VERTEX_POINT('',#39573);
#11556=VERTEX_POINT('',#39575);
#11557=VERTEX_POINT('',#39580);
#11558=VERTEX_POINT('',#39612);
#11559=VERTEX_POINT('',#39728);
#11560=VERTEX_POINT('',#39729);
#11561=VERTEX_POINT('',#39731);
#11562=VERTEX_POINT('',#39733);
#11563=VERTEX_POINT('',#39737);
#11564=VERTEX_POINT('',#39738);
#11565=VERTEX_POINT('',#39743);
#11566=VERTEX_POINT('',#39744);
#11567=VERTEX_POINT('',#39749);
#11568=VERTEX_POINT('',#39750);
#11569=VERTEX_POINT('',#39755);
#11570=VERTEX_POINT('',#39760);
#11571=VERTEX_POINT('',#39764);
#11572=VERTEX_POINT('',#39765);
#11573=VERTEX_POINT('',#39773);
#11574=VERTEX_POINT('',#39776);
#11575=VERTEX_POINT('',#39780);
#11576=VERTEX_POINT('',#39784);
#11577=VERTEX_POINT('',#39786);
#11578=VERTEX_POINT('',#39791);
#11579=VERTEX_POINT('',#39802);
#11580=VERTEX_POINT('',#39807);
#11581=VERTEX_POINT('',#39809);
#11582=VERTEX_POINT('',#39814);
#11583=VERTEX_POINT('',#39825);
#11584=VERTEX_POINT('',#39830);
#11585=VERTEX_POINT('',#39832);
#11586=VERTEX_POINT('',#39837);
#11587=VERTEX_POINT('',#39838);
#11588=VERTEX_POINT('',#39840);
#11589=VERTEX_POINT('',#39842);
#11590=VERTEX_POINT('',#39844);
#11591=VERTEX_POINT('',#39846);
#11592=VERTEX_POINT('',#39848);
#11593=VERTEX_POINT('',#39850);
#11594=VERTEX_POINT('',#39854);
#11595=VERTEX_POINT('',#39856);
#11596=VERTEX_POINT('',#39860);
#11597=VERTEX_POINT('',#39865);
#11598=VERTEX_POINT('',#39869);
#11599=VERTEX_POINT('',#39873);
#11600=VERTEX_POINT('',#39874);
#11601=VERTEX_POINT('',#39879);
#11602=VERTEX_POINT('',#39881);
#11603=VERTEX_POINT('',#39885);
#11604=VERTEX_POINT('',#39886);
#11605=VERTEX_POINT('',#39897);
#11606=VERTEX_POINT('',#39899);
#11607=VERTEX_POINT('',#39904);
#11608=VERTEX_POINT('',#39915);
#11609=VERTEX_POINT('',#39920);
#11610=VERTEX_POINT('',#39922);
#11611=VERTEX_POINT('',#39927);
#11612=VERTEX_POINT('',#39939);
#11613=VERTEX_POINT('',#39951);
#11614=VERTEX_POINT('',#39952);
#11615=VERTEX_POINT('',#39954);
#11616=VERTEX_POINT('',#39956);
#11617=VERTEX_POINT('',#39958);
#11618=VERTEX_POINT('',#39960);
#11619=VERTEX_POINT('',#39962);
#11620=VERTEX_POINT('',#39964);
#11621=VERTEX_POINT('',#40007);
#11622=VERTEX_POINT('',#40009);
#11623=VERTEX_POINT('',#40022);
#11624=VERTEX_POINT('',#40024);
#11625=VERTEX_POINT('',#40026);
#11626=VERTEX_POINT('',#40070);
#11627=VERTEX_POINT('',#40072);
#11628=VERTEX_POINT('',#40074);
#11629=VERTEX_POINT('',#40079);
#11630=VERTEX_POINT('',#40114);
#11631=VERTEX_POINT('',#40121);
#11632=VERTEX_POINT('',#40123);
#11633=VERTEX_POINT('',#40127);
#11634=VERTEX_POINT('',#40131);
#11635=VERTEX_POINT('',#40140);
#11636=VERTEX_POINT('',#40144);
#11637=VERTEX_POINT('',#40150);
#11638=VERTEX_POINT('',#40154);
#11639=VERTEX_POINT('',#40158);
#11640=VERTEX_POINT('',#40160);
#11641=VERTEX_POINT('',#40165);
#11642=VERTEX_POINT('',#40176);
#11643=VERTEX_POINT('',#40191);
#11644=VERTEX_POINT('',#40198);
#11645=VERTEX_POINT('',#40203);
#11646=VERTEX_POINT('',#40205);
#11647=VERTEX_POINT('',#40210);
#11648=VERTEX_POINT('',#40221);
#11649=VERTEX_POINT('',#40237);
#11650=VERTEX_POINT('',#40243);
#11651=VERTEX_POINT('',#40248);
#11652=VERTEX_POINT('',#40253);
#11653=VERTEX_POINT('',#40257);
#11654=VERTEX_POINT('',#40259);
#11655=VERTEX_POINT('',#40261);
#11656=VERTEX_POINT('',#40263);
#11657=VERTEX_POINT('',#40265);
#11658=VERTEX_POINT('',#40282);
#11659=VERTEX_POINT('',#40286);
#11660=VERTEX_POINT('',#40296);
#11661=VERTEX_POINT('',#40301);
#11662=VERTEX_POINT('',#40312);
#11663=VERTEX_POINT('',#40329);
#11664=VERTEX_POINT('',#40339);
#11665=VERTEX_POINT('',#40344);
#11666=VERTEX_POINT('',#40355);
#11667=VERTEX_POINT('',#40370);
#11668=VERTEX_POINT('',#40377);
#11669=VERTEX_POINT('',#40504);
#11670=VERTEX_POINT('',#40506);
#11671=VERTEX_POINT('',#40508);
#11672=VERTEX_POINT('',#40551);
#11673=VERTEX_POINT('',#40553);
#11674=VERTEX_POINT('',#40606);
#11675=VERTEX_POINT('',#40608);
#11676=VERTEX_POINT('',#40610);
#11677=VERTEX_POINT('',#40615);
#11678=VERTEX_POINT('',#40647);
#11679=VERTEX_POINT('',#40814);
#11680=VERTEX_POINT('',#40816);
#11681=VERTEX_POINT('',#40830);
#11682=VERTEX_POINT('',#40832);
#11683=VERTEX_POINT('',#40834);
#11684=VERTEX_POINT('',#40878);
#11685=VERTEX_POINT('',#40880);
#11686=VERTEX_POINT('',#40882);
#11687=VERTEX_POINT('',#40887);
#11688=VERTEX_POINT('',#40919);
#11689=VERTEX_POINT('',#41047);
#11690=VERTEX_POINT('',#41049);
#11691=VERTEX_POINT('',#41051);
#11692=VERTEX_POINT('',#41094);
#11693=VERTEX_POINT('',#41096);
#11694=VERTEX_POINT('',#41149);
#11695=VERTEX_POINT('',#41151);
#11696=VERTEX_POINT('',#41153);
#11697=VERTEX_POINT('',#41158);
#11698=VERTEX_POINT('',#41190);
#11699=VERTEX_POINT('',#41314);
#11700=VERTEX_POINT('',#41316);
#11701=VERTEX_POINT('',#41320);
#11702=VERTEX_POINT('',#41324);
#11703=VERTEX_POINT('',#41327);
#11704=VERTEX_POINT('',#41332);
#11705=VERTEX_POINT('',#41335);
#11706=VERTEX_POINT('',#41339);
#11707=VERTEX_POINT('',#41350);
#11708=VERTEX_POINT('',#41351);
#11709=VERTEX_POINT('',#41355);
#11710=VERTEX_POINT('',#41357);
#11711=VERTEX_POINT('',#41368);
#11712=VERTEX_POINT('',#41372);
#11713=VERTEX_POINT('',#41383);
#11714=VERTEX_POINT('',#41387);
#11715=VERTEX_POINT('',#41398);
#11716=VERTEX_POINT('',#41402);
#11717=VERTEX_POINT('',#41413);
#11718=VERTEX_POINT('',#41417);
#11719=VERTEX_POINT('',#41428);
#11720=VERTEX_POINT('',#41432);
#11721=VERTEX_POINT('',#41443);
#11722=VERTEX_POINT('',#41447);
#11723=VERTEX_POINT('',#41470);
#11724=VERTEX_POINT('',#41472);
#11725=VERTEX_POINT('',#41483);
#11726=VERTEX_POINT('',#41494);
#11727=VERTEX_POINT('',#41505);
#11728=VERTEX_POINT('',#41516);
#11729=VERTEX_POINT('',#41527);
#11730=VERTEX_POINT('',#41538);
#11731=VERTEX_POINT('',#41549);
#11732=VERTEX_POINT('',#41560);
#11733=VERTEX_POINT('',#41576);
#11734=VERTEX_POINT('',#41578);
#11735=VERTEX_POINT('',#41582);
#11736=VERTEX_POINT('',#41586);
#11737=VERTEX_POINT('',#41590);
#11738=VERTEX_POINT('',#41594);
#11739=VERTEX_POINT('',#41598);
#11740=VERTEX_POINT('',#41602);
#11741=VERTEX_POINT('',#41614);
#11742=VERTEX_POINT('',#41615);
#11743=VERTEX_POINT('',#41619);
#11744=VERTEX_POINT('',#41621);
#11745=VERTEX_POINT('',#41632);
#11746=VERTEX_POINT('',#41636);
#11747=VERTEX_POINT('',#41647);
#11748=VERTEX_POINT('',#41651);
#11749=VERTEX_POINT('',#41662);
#11750=VERTEX_POINT('',#41666);
#11751=VERTEX_POINT('',#41677);
#11752=VERTEX_POINT('',#41681);
#11753=VERTEX_POINT('',#41692);
#11754=VERTEX_POINT('',#41696);
#11755=VERTEX_POINT('',#41707);
#11756=VERTEX_POINT('',#41711);
#11757=VERTEX_POINT('',#41722);
#11758=VERTEX_POINT('',#41726);
#11759=VERTEX_POINT('',#41749);
#11760=VERTEX_POINT('',#41751);
#11761=VERTEX_POINT('',#41762);
#11762=VERTEX_POINT('',#41773);
#11763=VERTEX_POINT('',#41784);
#11764=VERTEX_POINT('',#41795);
#11765=VERTEX_POINT('',#41806);
#11766=VERTEX_POINT('',#41817);
#11767=VERTEX_POINT('',#41828);
#11768=VERTEX_POINT('',#41839);
#11769=VERTEX_POINT('',#41850);
#11770=VERTEX_POINT('',#41861);
#11771=VERTEX_POINT('',#41872);
#11772=VERTEX_POINT('',#41888);
#11773=VERTEX_POINT('',#41890);
#11774=VERTEX_POINT('',#41899);
#11775=VERTEX_POINT('',#41910);
#11776=VERTEX_POINT('',#41921);
#11777=VERTEX_POINT('',#41932);
#11778=VERTEX_POINT('',#41943);
#11779=VERTEX_POINT('',#41954);
#11780=VERTEX_POINT('',#41965);
#11781=VERTEX_POINT('',#41976);
#11782=VERTEX_POINT('',#41987);
#11783=VERTEX_POINT('',#41998);
#11784=VERTEX_POINT('',#42004);
#11785=VERTEX_POINT('',#42013);
#11786=VERTEX_POINT('',#42024);
#11787=VERTEX_POINT('',#42035);
#11788=VERTEX_POINT('',#42046);
#11789=VERTEX_POINT('',#42057);
#11790=VERTEX_POINT('',#42068);
#11791=VERTEX_POINT('',#42079);
#11792=VERTEX_POINT('',#42090);
#11793=VERTEX_POINT('',#42096);
#11794=VERTEX_POINT('',#42103);
#11795=VERTEX_POINT('',#42105);
#11796=VERTEX_POINT('',#42109);
#11797=VERTEX_POINT('',#42113);
#11798=VERTEX_POINT('',#42117);
#11799=VERTEX_POINT('',#42121);
#11800=VERTEX_POINT('',#42125);
#11801=VERTEX_POINT('',#42129);
#11802=VERTEX_POINT('',#42133);
#11803=VERTEX_POINT('',#42137);
#11804=VERTEX_POINT('',#42155);
#11805=VERTEX_POINT('',#42156);
#11806=VERTEX_POINT('',#42158);
#11807=VERTEX_POINT('',#42160);
#11808=VERTEX_POINT('',#42164);
#11809=VERTEX_POINT('',#42166);
#11810=VERTEX_POINT('',#42168);
#11811=VERTEX_POINT('',#42172);
#11812=VERTEX_POINT('',#42174);
#11813=VERTEX_POINT('',#42178);
#11814=VERTEX_POINT('',#42182);
#11815=VERTEX_POINT('',#42184);
#11816=VERTEX_POINT('',#42186);
#11817=VERTEX_POINT('',#42190);
#11818=VERTEX_POINT('',#42191);
#11819=VERTEX_POINT('',#42193);
#11820=VERTEX_POINT('',#42195);
#11821=VERTEX_POINT('',#42197);
#11822=VERTEX_POINT('',#42201);
#11823=VERTEX_POINT('',#42203);
#11824=VERTEX_POINT('',#42207);
#11825=VERTEX_POINT('',#42209);
#11826=VERTEX_POINT('',#42211);
#11827=VERTEX_POINT('',#42215);
#11828=VERTEX_POINT('',#42217);
#11829=VERTEX_POINT('',#42219);
#11830=VERTEX_POINT('',#42221);
#11831=VERTEX_POINT('',#42225);
#11832=VERTEX_POINT('',#42229);
#11833=VERTEX_POINT('',#42233);
#11834=VERTEX_POINT('',#42237);
#11835=VERTEX_POINT('',#42239);
#11836=VERTEX_POINT('',#42241);
#11837=VERTEX_POINT('',#42245);
#11838=VERTEX_POINT('',#42246);
#11839=VERTEX_POINT('',#42248);
#11840=VERTEX_POINT('',#42250);
#11841=VERTEX_POINT('',#42252);
#11842=VERTEX_POINT('',#42254);
#11843=VERTEX_POINT('',#42258);
#11844=VERTEX_POINT('',#42260);
#11845=VERTEX_POINT('',#42262);
#11846=VERTEX_POINT('',#42266);
#11847=VERTEX_POINT('',#42268);
#11848=VERTEX_POINT('',#42270);
#11849=VERTEX_POINT('',#42275);
#11850=VERTEX_POINT('',#42277);
#11851=VERTEX_POINT('',#42281);
#11852=VERTEX_POINT('',#42282);
#11853=VERTEX_POINT('',#42284);
#11854=VERTEX_POINT('',#42286);
#11855=VERTEX_POINT('',#42288);
#11856=VERTEX_POINT('',#42292);
#11857=VERTEX_POINT('',#42294);
#11858=VERTEX_POINT('',#42296);
#11859=VERTEX_POINT('',#42300);
#11860=VERTEX_POINT('',#42303);
#11861=VERTEX_POINT('',#42307);
#11862=VERTEX_POINT('',#42309);
#11863=VERTEX_POINT('',#42311);
#11864=VERTEX_POINT('',#42315);
#11865=VERTEX_POINT('',#42317);
#11866=VERTEX_POINT('',#42319);
#11867=VERTEX_POINT('',#42323);
#11868=VERTEX_POINT('',#42327);
#11869=VERTEX_POINT('',#42329);
#11870=VERTEX_POINT('',#42333);
#11871=VERTEX_POINT('',#42335);
#11872=VERTEX_POINT('',#42340);
#11873=VERTEX_POINT('',#42344);
#11874=VERTEX_POINT('',#42346);
#11875=VERTEX_POINT('',#42348);
#11876=VERTEX_POINT('',#42352);
#11877=VERTEX_POINT('',#42354);
#11878=VERTEX_POINT('',#42356);
#11879=VERTEX_POINT('',#42358);
#11880=VERTEX_POINT('',#42360);
#11881=VERTEX_POINT('',#42364);
#11882=VERTEX_POINT('',#42366);
#11883=VERTEX_POINT('',#42370);
#11884=VERTEX_POINT('',#42372);
#11885=VERTEX_POINT('',#42376);
#11886=VERTEX_POINT('',#42380);
#11887=VERTEX_POINT('',#42384);
#11888=VERTEX_POINT('',#42386);
#11889=VERTEX_POINT('',#42388);
#11890=VERTEX_POINT('',#42390);
#11891=VERTEX_POINT('',#42392);
#11892=VERTEX_POINT('',#42394);
#11893=VERTEX_POINT('',#42396);
#11894=VERTEX_POINT('',#42400);
#11895=VERTEX_POINT('',#42402);
#11896=VERTEX_POINT('',#42406);
#11897=VERTEX_POINT('',#42410);
#11898=VERTEX_POINT('',#42411);
#11899=VERTEX_POINT('',#42414);
#11900=VERTEX_POINT('',#42418);
#11901=VERTEX_POINT('',#42419);
#11902=VERTEX_POINT('',#42424);
#11903=VERTEX_POINT('',#42428);
#11904=VERTEX_POINT('',#42430);
#11905=VERTEX_POINT('',#42432);
#11906=VERTEX_POINT('',#42439);
#11907=VERTEX_POINT('',#42441);
#11908=VERTEX_POINT('',#42443);
#11909=VERTEX_POINT('',#42445);
#11910=VERTEX_POINT('',#42447);
#11911=VERTEX_POINT('',#42449);
#11912=VERTEX_POINT('',#42451);
#11913=VERTEX_POINT('',#42453);
#11914=VERTEX_POINT('',#42455);
#11915=VERTEX_POINT('',#42457);
#11916=VERTEX_POINT('',#42459);
#11917=VERTEX_POINT('',#42463);
#11918=VERTEX_POINT('',#42464);
#11919=VERTEX_POINT('',#42466);
#11920=VERTEX_POINT('',#42471);
#11921=VERTEX_POINT('',#42473);
#11922=VERTEX_POINT('',#42475);
#11923=VERTEX_POINT('',#42477);
#11924=VERTEX_POINT('',#42481);
#11925=VERTEX_POINT('',#42483);
#11926=VERTEX_POINT('',#42487);
#11927=VERTEX_POINT('',#42489);
#11928=VERTEX_POINT('',#42491);
#11929=VERTEX_POINT('',#42495);
#11930=VERTEX_POINT('',#42497);
#11931=VERTEX_POINT('',#42501);
#11932=VERTEX_POINT('',#42503);
#11933=VERTEX_POINT('',#42507);
#11934=VERTEX_POINT('',#42509);
#11935=VERTEX_POINT('',#42511);
#11936=VERTEX_POINT('',#42515);
#11937=VERTEX_POINT('',#42516);
#11938=VERTEX_POINT('',#42521);
#11939=VERTEX_POINT('',#42524);
#11940=VERTEX_POINT('',#42526);
#11941=VERTEX_POINT('',#42528);
#11942=VERTEX_POINT('',#42530);
#11943=VERTEX_POINT('',#42534);
#11944=VERTEX_POINT('',#42541);
#11945=VERTEX_POINT('',#42543);
#11946=VERTEX_POINT('',#42547);
#11947=VERTEX_POINT('',#42555);
#11948=VERTEX_POINT('',#42560);
#11949=VERTEX_POINT('',#42564);
#11950=VERTEX_POINT('',#42568);
#11951=VERTEX_POINT('',#42570);
#11952=VERTEX_POINT('',#42572);
#11953=VERTEX_POINT('',#42574);
#11954=VERTEX_POINT('',#42590);
#11955=VERTEX_POINT('',#42594);
#11956=VERTEX_POINT('',#42596);
#11957=VERTEX_POINT('',#42600);
#11958=VERTEX_POINT('',#42602);
#11959=VERTEX_POINT('',#42604);
#11960=VERTEX_POINT('',#42606);
#11961=VERTEX_POINT('',#42611);
#11962=VERTEX_POINT('',#42613);
#11963=VERTEX_POINT('',#42617);
#11964=VERTEX_POINT('',#42620);
#11965=VERTEX_POINT('',#42622);
#11966=VERTEX_POINT('',#42625);
#11967=VERTEX_POINT('',#42626);
#11968=VERTEX_POINT('',#42628);
#11969=VERTEX_POINT('',#42630);
#11970=VERTEX_POINT('',#42632);
#11971=VERTEX_POINT('',#42637);
#11972=VERTEX_POINT('',#42641);
#11973=VERTEX_POINT('',#42643);
#11974=VERTEX_POINT('',#42648);
#11975=VERTEX_POINT('',#42650);
#11976=VERTEX_POINT('',#42660);
#11977=VERTEX_POINT('',#42665);
#11978=VERTEX_POINT('',#42669);
#11979=VERTEX_POINT('',#42671);
#11980=VERTEX_POINT('',#42677);
#11981=VERTEX_POINT('',#42681);
#11982=VERTEX_POINT('',#42683);
#11983=VERTEX_POINT('',#42687);
#11984=VERTEX_POINT('',#42693);
#11985=VERTEX_POINT('',#42699);
#11986=VERTEX_POINT('',#42703);
#11987=VERTEX_POINT('',#42705);
#11988=VERTEX_POINT('',#42710);
#11989=VERTEX_POINT('',#42712);
#11990=VERTEX_POINT('',#42718);
#11991=VERTEX_POINT('',#42720);
#11992=VERTEX_POINT('',#42724);
#11993=VERTEX_POINT('',#42728);
#11994=VERTEX_POINT('',#42732);
#11995=VERTEX_POINT('',#42734);
#11996=VERTEX_POINT('',#42743);
#11997=VERTEX_POINT('',#42744);
#11998=VERTEX_POINT('',#42747);
#11999=VERTEX_POINT('',#42749);
#12000=VERTEX_POINT('',#42753);
#12001=VERTEX_POINT('',#42755);
#12002=VERTEX_POINT('',#42759);
#12003=VERTEX_POINT('',#42763);
#12004=VERTEX_POINT('',#42768);
#12005=VERTEX_POINT('',#42772);
#12006=VERTEX_POINT('',#42776);
#12007=VERTEX_POINT('',#42780);
#12008=VERTEX_POINT('',#42783);
#12009=VERTEX_POINT('',#42787);
#12010=VERTEX_POINT('',#42793);
#12011=VERTEX_POINT('',#42805);
#12012=VERTEX_POINT('',#42806);
#12013=VERTEX_POINT('',#42808);
#12014=VERTEX_POINT('',#42810);
#12015=VERTEX_POINT('',#42814);
#12016=VERTEX_POINT('',#42816);
#12017=VERTEX_POINT('',#42820);
#12018=VERTEX_POINT('',#42821);
#12019=VERTEX_POINT('',#42823);
#12020=VERTEX_POINT('',#42825);
#12021=VERTEX_POINT('',#42827);
#12022=VERTEX_POINT('',#42829);
#12023=VERTEX_POINT('',#42833);
#12024=VERTEX_POINT('',#42835);
#12025=VERTEX_POINT('',#42839);
#12026=VERTEX_POINT('',#42841);
#12027=VERTEX_POINT('',#42843);
#12028=VERTEX_POINT('',#42847);
#12029=VERTEX_POINT('',#42849);
#12030=VERTEX_POINT('',#42851);
#12031=VERTEX_POINT('',#42855);
#12032=VERTEX_POINT('',#42856);
#12033=VERTEX_POINT('',#42858);
#12034=VERTEX_POINT('',#42860);
#12035=VERTEX_POINT('',#42867);
#12036=VERTEX_POINT('',#42868);
#12037=VERTEX_POINT('',#42870);
#12038=VERTEX_POINT('',#42872);
#12039=VERTEX_POINT('',#42876);
#12040=VERTEX_POINT('',#42878);
#12041=VERTEX_POINT('',#42882);
#12042=VERTEX_POINT('',#42883);
#12043=VERTEX_POINT('',#42885);
#12044=VERTEX_POINT('',#42887);
#12045=VERTEX_POINT('',#42889);
#12046=VERTEX_POINT('',#42891);
#12047=VERTEX_POINT('',#42895);
#12048=VERTEX_POINT('',#42897);
#12049=VERTEX_POINT('',#42899);
#12050=VERTEX_POINT('',#42901);
#12051=VERTEX_POINT('',#42905);
#12052=VERTEX_POINT('',#42909);
#12053=VERTEX_POINT('',#42911);
#12054=VERTEX_POINT('',#42913);
#12055=VERTEX_POINT('',#42917);
#12056=VERTEX_POINT('',#42919);
#12057=VERTEX_POINT('',#42923);
#12058=VERTEX_POINT('',#42925);
#12059=VERTEX_POINT('',#42929);
#12060=VERTEX_POINT('',#42933);
#12061=VERTEX_POINT('',#42935);
#12062=VERTEX_POINT('',#42939);
#12063=VERTEX_POINT('',#42941);
#12064=VERTEX_POINT('',#42945);
#12065=VERTEX_POINT('',#42947);
#12066=VERTEX_POINT('',#42951);
#12067=VERTEX_POINT('',#42955);
#12068=VERTEX_POINT('',#42959);
#12069=VERTEX_POINT('',#42960);
#12070=VERTEX_POINT('',#42962);
#12071=VERTEX_POINT('',#42964);
#12072=VERTEX_POINT('',#42971);
#12073=VERTEX_POINT('',#42975);
#12074=VERTEX_POINT('',#42979);
#12075=VERTEX_POINT('',#42980);
#12076=VERTEX_POINT('',#42982);
#12077=VERTEX_POINT('',#42987);
#12078=VERTEX_POINT('',#42991);
#12079=VERTEX_POINT('',#42997);
#12080=VERTEX_POINT('',#43001);
#12081=VERTEX_POINT('',#43008);
#12082=VERTEX_POINT('',#43013);
#12083=VERTEX_POINT('',#43015);
#12084=VERTEX_POINT('',#43017);
#12085=VERTEX_POINT('',#43019);
#12086=VERTEX_POINT('',#43021);
#12087=VERTEX_POINT('',#43023);
#12088=VERTEX_POINT('',#43025);
#12089=VERTEX_POINT('',#43027);
#12090=VERTEX_POINT('',#43029);
#12091=VERTEX_POINT('',#43031);
#12092=VERTEX_POINT('',#43033);
#12093=VERTEX_POINT('',#43037);
#12094=VERTEX_POINT('',#43039);
#12095=VERTEX_POINT('',#43041);
#12096=VERTEX_POINT('',#43045);
#12097=VERTEX_POINT('',#43050);
#12098=VERTEX_POINT('',#43054);
#12099=VERTEX_POINT('',#43058);
#12100=VERTEX_POINT('',#43062);
#12101=VERTEX_POINT('',#43063);
#12102=VERTEX_POINT('',#43065);
#12103=VERTEX_POINT('',#43070);
#12104=VERTEX_POINT('',#43074);
#12105=VERTEX_POINT('',#43076);
#12106=VERTEX_POINT('',#43080);
#12107=VERTEX_POINT('',#43081);
#12108=VERTEX_POINT('',#43084);
#12109=VERTEX_POINT('',#43090);
#12110=VERTEX_POINT('',#43091);
#12111=VERTEX_POINT('',#43099);
#12112=VERTEX_POINT('',#43104);
#12113=VERTEX_POINT('',#43106);
#12114=VERTEX_POINT('',#43110);
#12115=VERTEX_POINT('',#43112);
#12116=VERTEX_POINT('',#43114);
#12117=VERTEX_POINT('',#43119);
#12118=VERTEX_POINT('',#43120);
#12119=VERTEX_POINT('',#43122);
#12120=VERTEX_POINT('',#43124);
#12121=VERTEX_POINT('',#43128);
#12122=VERTEX_POINT('',#43130);
#12123=VERTEX_POINT('',#43134);
#12124=VERTEX_POINT('',#43136);
#12125=VERTEX_POINT('',#43138);
#12126=VERTEX_POINT('',#43142);
#12127=VERTEX_POINT('',#43143);
#12128=VERTEX_POINT('',#43145);
#12129=VERTEX_POINT('',#43148);
#12130=VERTEX_POINT('',#43152);
#12131=VERTEX_POINT('',#43154);
#12132=VERTEX_POINT('',#43160);
#12133=VERTEX_POINT('',#43161);
#12134=VERTEX_POINT('',#43163);
#12135=VERTEX_POINT('',#43165);
#12136=VERTEX_POINT('',#43173);
#12137=VERTEX_POINT('',#43179);
#12138=VERTEX_POINT('',#43181);
#12139=VERTEX_POINT('',#43183);
#12140=VERTEX_POINT('',#43185);
#12141=VERTEX_POINT('',#43187);
#12142=VERTEX_POINT('',#43189);
#12143=VERTEX_POINT('',#43197);
#12144=VERTEX_POINT('',#43198);
#12145=VERTEX_POINT('',#43203);
#12146=VERTEX_POINT('',#43207);
#12147=VERTEX_POINT('',#43208);
#12148=VERTEX_POINT('',#43214);
#12149=VERTEX_POINT('',#43220);
#12150=VERTEX_POINT('',#43222);
#12151=VERTEX_POINT('',#43229);
#12152=VERTEX_POINT('',#43231);
#12153=VERTEX_POINT('',#43233);
#12154=VERTEX_POINT('',#43241);
#12155=VERTEX_POINT('',#43245);
#12156=VERTEX_POINT('',#43248);
#12157=VERTEX_POINT('',#43249);
#12158=VERTEX_POINT('',#43251);
#12159=VERTEX_POINT('',#43253);
#12160=VERTEX_POINT('',#43257);
#12161=VERTEX_POINT('',#43259);
#12162=VERTEX_POINT('',#43265);
#12163=VERTEX_POINT('',#43272);
#12164=VERTEX_POINT('',#43273);
#12165=VERTEX_POINT('',#43275);
#12166=VERTEX_POINT('',#43277);
#12167=VERTEX_POINT('',#43281);
#12168=VERTEX_POINT('',#43283);
#12169=VERTEX_POINT('',#43287);
#12170=VERTEX_POINT('',#43291);
#12171=VERTEX_POINT('',#43297);
#12172=VERTEX_POINT('',#43299);
#12173=VERTEX_POINT('',#43303);
#12174=VERTEX_POINT('',#43310);
#12175=VERTEX_POINT('',#43320);
#12176=VERTEX_POINT('',#43322);
#12177=VERTEX_POINT('',#43326);
#12178=VERTEX_POINT('',#43330);
#12179=VERTEX_POINT('',#43336);
#12180=VERTEX_POINT('',#43338);
#12181=VERTEX_POINT('',#43342);
#12182=VERTEX_POINT('',#43349);
#12183=VERTEX_POINT('',#43366);
#12184=VERTEX_POINT('',#43367);
#12185=VERTEX_POINT('',#43369);
#12186=VERTEX_POINT('',#43371);
#12187=VERTEX_POINT('',#43373);
#12188=VERTEX_POINT('',#43375);
#12189=VERTEX_POINT('',#43379);
#12190=VERTEX_POINT('',#43381);
#12191=VERTEX_POINT('',#43383);
#12192=VERTEX_POINT('',#43385);
#12193=VERTEX_POINT('',#43389);
#12194=VERTEX_POINT('',#43393);
#12195=VERTEX_POINT('',#43395);
#12196=VERTEX_POINT('',#43397);
#12197=VERTEX_POINT('',#43401);
#12198=VERTEX_POINT('',#43403);
#12199=VERTEX_POINT('',#43407);
#12200=VERTEX_POINT('',#43408);
#12201=VERTEX_POINT('',#43410);
#12202=VERTEX_POINT('',#43412);
#12203=VERTEX_POINT('',#43414);
#12204=VERTEX_POINT('',#43416);
#12205=VERTEX_POINT('',#43420);
#12206=VERTEX_POINT('',#43422);
#12207=VERTEX_POINT('',#43424);
#12208=VERTEX_POINT('',#43426);
#12209=VERTEX_POINT('',#43430);
#12210=VERTEX_POINT('',#43432);
#12211=VERTEX_POINT('',#43436);
#12212=VERTEX_POINT('',#43439);
#12213=VERTEX_POINT('',#43441);
#12214=VERTEX_POINT('',#43444);
#12215=VERTEX_POINT('',#43445);
#12216=VERTEX_POINT('',#43447);
#12217=VERTEX_POINT('',#43449);
#12218=VERTEX_POINT('',#43451);
#12219=VERTEX_POINT('',#43453);
#12220=VERTEX_POINT('',#43457);
#12221=VERTEX_POINT('',#43460);
#12222=VERTEX_POINT('',#43464);
#12223=VERTEX_POINT('',#43467);
#12224=VERTEX_POINT('',#43469);
#12225=VERTEX_POINT('',#43472);
#12226=VERTEX_POINT('',#43474);
#12227=VERTEX_POINT('',#43476);
#12228=VERTEX_POINT('',#43480);
#12229=VERTEX_POINT('',#43485);
#12230=VERTEX_POINT('',#43489);
#12231=VERTEX_POINT('',#43493);
#12232=VERTEX_POINT('',#43499);
#12233=VERTEX_POINT('',#43503);
#12234=VERTEX_POINT('',#43509);
#12235=VERTEX_POINT('',#43531);
#12236=VERTEX_POINT('',#43532);
#12237=VERTEX_POINT('',#43534);
#12238=VERTEX_POINT('',#43536);
#12239=VERTEX_POINT('',#43540);
#12240=VERTEX_POINT('',#43541);
#12241=VERTEX_POINT('',#43546);
#12242=VERTEX_POINT('',#43547);
#12243=VERTEX_POINT('',#43552);
#12244=VERTEX_POINT('',#43553);
#12245=VERTEX_POINT('',#43558);
#12246=VERTEX_POINT('',#43559);
#12247=VERTEX_POINT('',#43564);
#12248=VERTEX_POINT('',#43565);
#12249=VERTEX_POINT('',#43570);
#12250=VERTEX_POINT('',#43571);
#12251=VERTEX_POINT('',#43579);
#12252=VERTEX_POINT('',#43581);
#12253=VERTEX_POINT('',#43585);
#12254=VERTEX_POINT('',#43589);
#12255=VERTEX_POINT('',#43593);
#12256=VERTEX_POINT('',#43597);
#12257=VERTEX_POINT('',#43599);
#12258=VERTEX_POINT('',#43601);
#12259=VERTEX_POINT('',#43604);
#12260=VERTEX_POINT('',#43605);
#12261=VERTEX_POINT('',#43607);
#12262=VERTEX_POINT('',#43609);
#12263=VERTEX_POINT('',#43613);
#12264=VERTEX_POINT('',#43615);
#12265=VERTEX_POINT('',#43619);
#12266=VERTEX_POINT('',#43621);
#12267=VERTEX_POINT('',#43625);
#12268=VERTEX_POINT('',#43627);
#12269=VERTEX_POINT('',#43631);
#12270=VERTEX_POINT('',#43635);
#12271=VERTEX_POINT('',#43639);
#12272=VERTEX_POINT('',#43640);
#12273=VERTEX_POINT('',#43645);
#12274=VERTEX_POINT('',#43646);
#12275=VERTEX_POINT('',#43651);
#12276=VERTEX_POINT('',#43652);
#12277=VERTEX_POINT('',#43657);
#12278=VERTEX_POINT('',#43664);
#12279=VERTEX_POINT('',#43666);
#12280=VERTEX_POINT('',#43670);
#12281=VERTEX_POINT('',#43674);
#12282=VERTEX_POINT('',#43678);
#12283=VERTEX_POINT('',#43681);
#12284=VERTEX_POINT('',#43688);
#12285=VERTEX_POINT('',#43689);
#12286=VERTEX_POINT('',#43691);
#12287=VERTEX_POINT('',#43693);
#12288=VERTEX_POINT('',#43697);
#12289=VERTEX_POINT('',#43698);
#12290=VERTEX_POINT('',#43703);
#12291=VERTEX_POINT('',#43704);
#12292=VERTEX_POINT('',#43709);
#12293=VERTEX_POINT('',#43710);
#12294=VERTEX_POINT('',#43715);
#12295=VERTEX_POINT('',#43716);
#12296=VERTEX_POINT('',#43721);
#12297=VERTEX_POINT('',#43723);
#12298=VERTEX_POINT('',#43727);
#12299=VERTEX_POINT('',#43731);
#12300=VERTEX_POINT('',#43732);
#12301=VERTEX_POINT('',#43734);
#12302=VERTEX_POINT('',#43736);
#12303=VERTEX_POINT('',#43740);
#12304=VERTEX_POINT('',#43741);
#12305=VERTEX_POINT('',#43746);
#12306=VERTEX_POINT('',#43747);
#12307=VERTEX_POINT('',#43752);
#12308=VERTEX_POINT('',#43753);
#12309=VERTEX_POINT('',#43758);
#12310=VERTEX_POINT('',#43759);
#12311=VERTEX_POINT('',#43765);
#12312=VERTEX_POINT('',#43768);
#12313=VERTEX_POINT('',#43769);
#12314=VERTEX_POINT('',#43771);
#12315=VERTEX_POINT('',#43773);
#12316=VERTEX_POINT('',#43777);
#12317=VERTEX_POINT('',#43778);
#12318=VERTEX_POINT('',#43783);
#12319=VERTEX_POINT('',#43784);
#12320=VERTEX_POINT('',#43789);
#12321=VERTEX_POINT('',#43790);
#12322=VERTEX_POINT('',#43795);
#12323=VERTEX_POINT('',#43796);
#12324=VERTEX_POINT('',#43802);
#12325=VERTEX_POINT('',#43805);
#12326=VERTEX_POINT('',#43806);
#12327=VERTEX_POINT('',#43808);
#12328=VERTEX_POINT('',#43810);
#12329=VERTEX_POINT('',#43814);
#12330=VERTEX_POINT('',#43815);
#12331=VERTEX_POINT('',#43820);
#12332=VERTEX_POINT('',#43821);
#12333=VERTEX_POINT('',#43826);
#12334=VERTEX_POINT('',#43827);
#12335=VERTEX_POINT('',#43832);
#12336=VERTEX_POINT('',#43833);
#12337=VERTEX_POINT('',#43838);
#12338=VERTEX_POINT('',#43849);
#12339=VERTEX_POINT('',#43853);
#12340=VERTEX_POINT('',#43857);
#12341=VERTEX_POINT('',#43859);
#12342=VERTEX_POINT('',#43863);
#12343=VERTEX_POINT('',#43868);
#12344=VERTEX_POINT('',#43872);
#12345=VERTEX_POINT('',#43876);
#12346=VERTEX_POINT('',#43880);
#12347=VERTEX_POINT('',#43884);
#12348=VERTEX_POINT('',#43887);
#12349=VERTEX_POINT('',#43899);
#12350=VERTEX_POINT('',#43909);
#12351=VERTEX_POINT('',#43917);
#12352=VERTEX_POINT('',#43922);
#12353=VERTEX_POINT('',#43928);
#12354=VERTEX_POINT('',#43930);
#12355=VERTEX_POINT('',#43934);
#12356=VERTEX_POINT('',#43938);
#12357=VERTEX_POINT('',#43946);
#12358=VERTEX_POINT('',#43947);
#12359=VERTEX_POINT('',#43952);
#12360=VERTEX_POINT('',#43956);
#12361=VERTEX_POINT('',#43959);
#12362=VERTEX_POINT('',#43963);
#12363=VERTEX_POINT('',#43969);
#12364=VERTEX_POINT('',#43971);
#12365=VERTEX_POINT('',#43975);
#12366=VERTEX_POINT('',#43979);
#12367=VERTEX_POINT('',#43980);
#12368=VERTEX_POINT('',#43985);
#12369=VERTEX_POINT('',#43986);
#12370=VERTEX_POINT('',#43991);
#12371=VERTEX_POINT('',#43992);
#12372=VERTEX_POINT('',#43997);
#12373=VERTEX_POINT('',#44002);
#12374=VERTEX_POINT('',#44020);
#12375=VERTEX_POINT('',#44021);
#12376=VERTEX_POINT('',#44023);
#12377=VERTEX_POINT('',#44040);
#12378=VERTEX_POINT('',#44053);
#12379=VERTEX_POINT('',#44054);
#12380=VERTEX_POINT('',#44143);
#12381=VERTEX_POINT('',#44144);
#12382=VERTEX_POINT('',#44233);
#12383=VERTEX_POINT('',#44234);
#12384=VERTEX_POINT('',#44323);
#12385=VERTEX_POINT('',#44324);
#12386=VERTEX_POINT('',#44326);
#12387=VERTEX_POINT('',#44412);
#12388=VERTEX_POINT('',#44413);
#12389=VERTEX_POINT('',#44415);
#12390=VERTEX_POINT('',#44428);
#12391=VERTEX_POINT('',#44440);
#12392=VERTEX_POINT('',#44441);
#12393=VERTEX_POINT('',#44478);
#12394=VERTEX_POINT('',#44479);
#12395=VERTEX_POINT('',#44516);
#12396=VERTEX_POINT('',#44517);
#12397=VERTEX_POINT('',#44554);
#12398=VERTEX_POINT('',#44555);
#12399=VERTEX_POINT('',#44557);
#12400=VERTEX_POINT('',#44559);
#12401=VERTEX_POINT('',#44565);
#12402=VERTEX_POINT('',#44569);
#12403=VERTEX_POINT('',#44575);
#12404=VERTEX_POINT('',#44576);
#12405=VERTEX_POINT('',#44578);
#12406=VERTEX_POINT('',#44580);
#12407=VERTEX_POINT('',#44586);
#12408=VERTEX_POINT('',#44590);
#12409=VERTEX_POINT('',#44596);
#12410=VERTEX_POINT('',#44597);
#12411=VERTEX_POINT('',#44599);
#12412=VERTEX_POINT('',#44601);
#12413=VERTEX_POINT('',#44607);
#12414=VERTEX_POINT('',#44611);
#12415=VERTEX_POINT('',#44617);
#12416=VERTEX_POINT('',#44618);
#12417=VERTEX_POINT('',#44620);
#12418=VERTEX_POINT('',#44622);
#12419=VERTEX_POINT('',#44628);
#12420=VERTEX_POINT('',#44632);
#12421=VERTEX_POINT('',#44638);
#12422=VERTEX_POINT('',#44639);
#12423=VERTEX_POINT('',#44641);
#12424=VERTEX_POINT('',#44643);
#12425=VERTEX_POINT('',#44649);
#12426=VERTEX_POINT('',#44653);
#12427=VERTEX_POINT('',#44659);
#12428=VERTEX_POINT('',#44660);
#12429=VERTEX_POINT('',#44662);
#12430=VERTEX_POINT('',#44664);
#12431=VERTEX_POINT('',#44670);
#12432=VERTEX_POINT('',#44674);
#12433=VERTEX_POINT('',#44678);
#12434=VERTEX_POINT('',#44682);
#12435=VERTEX_POINT('',#44683);
#12436=VERTEX_POINT('',#44685);
#12437=VERTEX_POINT('',#44687);
#12438=VERTEX_POINT('',#44693);
#12439=VERTEX_POINT('',#44697);
#12440=VERTEX_POINT('',#44703);
#12441=VERTEX_POINT('',#44704);
#12442=VERTEX_POINT('',#44706);
#12443=VERTEX_POINT('',#44708);
#12444=VERTEX_POINT('',#44714);
#12445=VERTEX_POINT('',#44718);
#12446=VERTEX_POINT('',#44724);
#12447=VERTEX_POINT('',#44725);
#12448=VERTEX_POINT('',#44727);
#12449=VERTEX_POINT('',#44729);
#12450=VERTEX_POINT('',#44735);
#12451=VERTEX_POINT('',#44739);
#12452=VERTEX_POINT('',#44745);
#12453=VERTEX_POINT('',#44746);
#12454=VERTEX_POINT('',#44748);
#12455=VERTEX_POINT('',#44750);
#12456=VERTEX_POINT('',#44756);
#12457=VERTEX_POINT('',#44760);
#12458=VERTEX_POINT('',#44766);
#12459=VERTEX_POINT('',#44767);
#12460=VERTEX_POINT('',#44769);
#12461=VERTEX_POINT('',#44771);
#12462=VERTEX_POINT('',#44777);
#12463=VERTEX_POINT('',#44781);
#12464=VERTEX_POINT('',#44787);
#12465=VERTEX_POINT('',#44788);
#12466=VERTEX_POINT('',#44790);
#12467=VERTEX_POINT('',#44792);
#12468=VERTEX_POINT('',#44798);
#12469=VERTEX_POINT('',#44802);
#12470=VERTEX_POINT('',#44808);
#12471=VERTEX_POINT('',#44809);
#12472=VERTEX_POINT('',#44811);
#12473=VERTEX_POINT('',#44813);
#12474=VERTEX_POINT('',#44819);
#12475=VERTEX_POINT('',#44823);
#12476=VERTEX_POINT('',#44829);
#12477=VERTEX_POINT('',#44830);
#12478=VERTEX_POINT('',#44832);
#12479=VERTEX_POINT('',#44834);
#12480=VERTEX_POINT('',#44840);
#12481=VERTEX_POINT('',#44844);
#12482=VERTEX_POINT('',#44850);
#12483=VERTEX_POINT('',#44851);
#12484=VERTEX_POINT('',#44853);
#12485=VERTEX_POINT('',#44855);
#12486=VERTEX_POINT('',#44861);
#12487=VERTEX_POINT('',#44865);
#12488=VERTEX_POINT('',#44871);
#12489=VERTEX_POINT('',#44872);
#12490=VERTEX_POINT('',#44874);
#12491=VERTEX_POINT('',#44876);
#12492=VERTEX_POINT('',#44882);
#12493=VERTEX_POINT('',#44886);
#12494=VERTEX_POINT('',#44892);
#12495=VERTEX_POINT('',#44893);
#12496=VERTEX_POINT('',#44895);
#12497=VERTEX_POINT('',#44897);
#12498=VERTEX_POINT('',#44903);
#12499=VERTEX_POINT('',#44907);
#12500=VERTEX_POINT('',#44913);
#12501=VERTEX_POINT('',#44914);
#12502=VERTEX_POINT('',#44916);
#12503=VERTEX_POINT('',#44918);
#12504=VERTEX_POINT('',#44924);
#12505=VERTEX_POINT('',#44928);
#12506=VERTEX_POINT('',#44934);
#12507=VERTEX_POINT('',#44935);
#12508=VERTEX_POINT('',#44937);
#12509=VERTEX_POINT('',#44939);
#12510=VERTEX_POINT('',#44945);
#12511=VERTEX_POINT('',#44949);
#12512=VERTEX_POINT('',#44955);
#12513=VERTEX_POINT('',#44956);
#12514=VERTEX_POINT('',#44958);
#12515=VERTEX_POINT('',#44960);
#12516=VERTEX_POINT('',#44966);
#12517=VERTEX_POINT('',#44970);
#12518=VERTEX_POINT('',#44976);
#12519=VERTEX_POINT('',#44977);
#12520=VERTEX_POINT('',#44979);
#12521=VERTEX_POINT('',#44981);
#12522=VERTEX_POINT('',#44987);
#12523=VERTEX_POINT('',#44991);
#12524=VERTEX_POINT('',#44997);
#12525=VERTEX_POINT('',#44998);
#12526=VERTEX_POINT('',#45000);
#12527=VERTEX_POINT('',#45002);
#12528=VERTEX_POINT('',#45008);
#12529=VERTEX_POINT('',#45012);
#12530=VERTEX_POINT('',#45018);
#12531=VERTEX_POINT('',#45019);
#12532=VERTEX_POINT('',#45021);
#12533=VERTEX_POINT('',#45023);
#12534=VERTEX_POINT('',#45029);
#12535=VERTEX_POINT('',#45033);
#12536=VERTEX_POINT('',#45039);
#12537=VERTEX_POINT('',#45040);
#12538=VERTEX_POINT('',#45042);
#12539=VERTEX_POINT('',#45044);
#12540=VERTEX_POINT('',#45050);
#12541=VERTEX_POINT('',#45054);
#12542=VERTEX_POINT('',#45060);
#12543=VERTEX_POINT('',#45385);
#12544=VERTEX_POINT('',#45484);
#12545=VERTEX_POINT('',#45592);
#12546=VERTEX_POINT('',#46043);
#12547=VERTEX_POINT('',#46046);
#12548=VERTEX_POINT('',#46050);
#12549=VERTEX_POINT('',#46054);
#12550=VERTEX_POINT('',#46059);
#12551=VERTEX_POINT('',#46068);
#12552=VERTEX_POINT('',#46069);
#12553=VERTEX_POINT('',#46071);
#12554=VERTEX_POINT('',#46082);
#12555=VERTEX_POINT('',#46095);
#12556=VERTEX_POINT('',#46096);
#12557=VERTEX_POINT('',#46143);
#12558=VERTEX_POINT('',#46144);
#12559=VERTEX_POINT('',#46191);
#12560=VERTEX_POINT('',#46192);
#12561=VERTEX_POINT('',#46245);
#12562=VERTEX_POINT('',#46246);
#12563=VERTEX_POINT('',#46293);
#12564=VERTEX_POINT('',#46294);
#12565=VERTEX_POINT('',#46341);
#12566=VERTEX_POINT('',#46342);
#12567=VERTEX_POINT('',#46395);
#12568=VERTEX_POINT('',#46396);
#12569=VERTEX_POINT('',#46443);
#12570=VERTEX_POINT('',#46444);
#12571=VERTEX_POINT('',#46491);
#12572=VERTEX_POINT('',#46492);
#12573=VERTEX_POINT('',#46545);
#12574=VERTEX_POINT('',#46546);
#12575=VERTEX_POINT('',#46593);
#12576=VERTEX_POINT('',#46594);
#12577=VERTEX_POINT('',#46641);
#12578=VERTEX_POINT('',#46642);
#12579=VERTEX_POINT('',#46689);
#12580=VERTEX_POINT('',#46690);
#12581=VERTEX_POINT('',#46737);
#12582=VERTEX_POINT('',#46738);
#12583=VERTEX_POINT('',#46785);
#12584=VERTEX_POINT('',#46786);
#12585=VERTEX_POINT('',#46788);
#12586=VERTEX_POINT('',#46794);
#12587=VERTEX_POINT('',#46801);
#12588=VERTEX_POINT('',#46802);
#12589=VERTEX_POINT('',#46826);
#12590=VERTEX_POINT('',#46827);
#12591=VERTEX_POINT('',#46850);
#12592=VERTEX_POINT('',#46851);
#12593=VERTEX_POINT('',#46876);
#12594=VERTEX_POINT('',#46877);
#12595=VERTEX_POINT('',#46900);
#12596=VERTEX_POINT('',#46901);
#12597=VERTEX_POINT('',#46924);
#12598=VERTEX_POINT('',#46925);
#12599=VERTEX_POINT('',#46949);
#12600=VERTEX_POINT('',#46950);
#12601=VERTEX_POINT('',#46974);
#12602=VERTEX_POINT('',#46975);
#12603=VERTEX_POINT('',#46998);
#12604=VERTEX_POINT('',#46999);
#12605=VERTEX_POINT('',#47023);
#12606=VERTEX_POINT('',#47024);
#12607=VERTEX_POINT('',#47048);
#12608=VERTEX_POINT('',#47049);
#12609=VERTEX_POINT('',#47072);
#12610=VERTEX_POINT('',#47073);
#12611=VERTEX_POINT('',#47097);
#12612=VERTEX_POINT('',#47098);
#12613=VERTEX_POINT('',#47122);
#12614=VERTEX_POINT('',#47123);
#12615=VERTEX_POINT('',#47146);
#12616=VERTEX_POINT('',#47147);
#12617=VERTEX_POINT('',#47151);
#12618=VERTEX_POINT('',#47153);
#12619=VERTEX_POINT('',#47157);
#12620=VERTEX_POINT('',#47161);
#12621=VERTEX_POINT('',#47167);
#12622=VERTEX_POINT('',#47168);
#12623=VERTEX_POINT('',#47172);
#12624=VERTEX_POINT('',#47174);
#12625=VERTEX_POINT('',#47178);
#12626=VERTEX_POINT('',#47182);
#12627=VERTEX_POINT('',#47188);
#12628=VERTEX_POINT('',#47189);
#12629=VERTEX_POINT('',#47193);
#12630=VERTEX_POINT('',#47195);
#12631=VERTEX_POINT('',#47199);
#12632=VERTEX_POINT('',#47203);
#12633=VERTEX_POINT('',#47209);
#12634=VERTEX_POINT('',#47210);
#12635=VERTEX_POINT('',#47214);
#12636=VERTEX_POINT('',#47216);
#12637=VERTEX_POINT('',#47220);
#12638=VERTEX_POINT('',#47224);
#12639=VERTEX_POINT('',#47230);
#12640=VERTEX_POINT('',#47231);
#12641=VERTEX_POINT('',#47235);
#12642=VERTEX_POINT('',#47237);
#12643=VERTEX_POINT('',#47241);
#12644=VERTEX_POINT('',#47245);
#12645=VERTEX_POINT('',#47251);
#12646=VERTEX_POINT('',#47252);
#12647=VERTEX_POINT('',#47256);
#12648=VERTEX_POINT('',#47258);
#12649=VERTEX_POINT('',#47262);
#12650=VERTEX_POINT('',#47266);
#12651=VERTEX_POINT('',#47272);
#12652=VERTEX_POINT('',#47273);
#12653=VERTEX_POINT('',#47277);
#12654=VERTEX_POINT('',#47279);
#12655=VERTEX_POINT('',#47283);
#12656=VERTEX_POINT('',#47287);
#12657=VERTEX_POINT('',#47293);
#12658=VERTEX_POINT('',#47294);
#12659=VERTEX_POINT('',#47298);
#12660=VERTEX_POINT('',#47300);
#12661=VERTEX_POINT('',#47304);
#12662=VERTEX_POINT('',#47308);
#12663=VERTEX_POINT('',#47314);
#12664=VERTEX_POINT('',#47315);
#12665=VERTEX_POINT('',#47319);
#12666=VERTEX_POINT('',#47321);
#12667=VERTEX_POINT('',#47325);
#12668=VERTEX_POINT('',#47329);
#12669=VERTEX_POINT('',#47335);
#12670=VERTEX_POINT('',#47336);
#12671=VERTEX_POINT('',#47340);
#12672=VERTEX_POINT('',#47342);
#12673=VERTEX_POINT('',#47346);
#12674=VERTEX_POINT('',#47350);
#12675=VERTEX_POINT('',#47356);
#12676=VERTEX_POINT('',#47357);
#12677=VERTEX_POINT('',#47361);
#12678=VERTEX_POINT('',#47363);
#12679=VERTEX_POINT('',#47367);
#12680=VERTEX_POINT('',#47371);
#12681=VERTEX_POINT('',#47377);
#12682=VERTEX_POINT('',#47378);
#12683=VERTEX_POINT('',#47382);
#12684=VERTEX_POINT('',#47384);
#12685=VERTEX_POINT('',#47388);
#12686=VERTEX_POINT('',#47392);
#12687=VERTEX_POINT('',#47398);
#12688=VERTEX_POINT('',#47399);
#12689=VERTEX_POINT('',#47403);
#12690=VERTEX_POINT('',#47405);
#12691=VERTEX_POINT('',#47409);
#12692=VERTEX_POINT('',#47413);
#12693=VERTEX_POINT('',#47419);
#12694=VERTEX_POINT('',#47420);
#12695=VERTEX_POINT('',#47424);
#12696=VERTEX_POINT('',#47426);
#12697=VERTEX_POINT('',#47430);
#12698=VERTEX_POINT('',#47432);
#12699=VERTEX_POINT('',#47436);
#12700=VERTEX_POINT('',#47442);
#12701=VERTEX_POINT('',#47443);
#12702=VERTEX_POINT('',#47447);
#12703=VERTEX_POINT('',#47449);
#12704=VERTEX_POINT('',#47453);
#12705=VERTEX_POINT('',#47457);
#12706=VERTEX_POINT('',#47463);
#12707=VERTEX_POINT('',#47464);
#12708=VERTEX_POINT('',#47468);
#12709=VERTEX_POINT('',#47470);
#12710=VERTEX_POINT('',#47474);
#12711=VERTEX_POINT('',#47478);
#12712=VERTEX_POINT('',#47484);
#12713=VERTEX_POINT('',#47485);
#12714=VERTEX_POINT('',#47489);
#12715=VERTEX_POINT('',#47491);
#12716=VERTEX_POINT('',#47495);
#12717=VERTEX_POINT('',#47499);
#12718=VERTEX_POINT('',#47505);
#12719=VERTEX_POINT('',#47506);
#12720=VERTEX_POINT('',#47510);
#12721=VERTEX_POINT('',#47512);
#12722=VERTEX_POINT('',#47516);
#12723=VERTEX_POINT('',#47520);
#12724=VERTEX_POINT('',#47533);
#12725=VERTEX_POINT('',#47951);
#12726=VERTEX_POINT('',#48032);
#12727=VERTEX_POINT('',#48107);
#12728=VERTEX_POINT('',#48110);
#12729=VERTEX_POINT('',#48590);
#12730=VERTEX_POINT('',#48672);
#12731=VERTEX_POINT('',#48679);
#12732=VERTEX_POINT('',#48684);
#12733=VERTEX_POINT('',#48690);
#12734=VERTEX_POINT('',#48692);
#12735=VERTEX_POINT('',#48697);
#12736=VERTEX_POINT('',#48698);
#12737=VERTEX_POINT('',#48700);
#12738=VERTEX_POINT('',#48702);
#12739=VERTEX_POINT('',#48704);
#12740=VERTEX_POINT('',#48706);
#12741=VERTEX_POINT('',#48709);
#12742=VERTEX_POINT('',#48712);
#12743=VERTEX_POINT('',#48713);
#12744=VERTEX_POINT('',#48718);
#12745=VERTEX_POINT('',#48722);
#12746=VERTEX_POINT('',#48726);
#12747=VERTEX_POINT('',#48730);
#12748=VERTEX_POINT('',#48737);
#12749=VERTEX_POINT('',#48738);
#12750=VERTEX_POINT('',#48742);
#12751=VERTEX_POINT('',#48743);
#12752=VERTEX_POINT('',#48745);
#12753=VERTEX_POINT('',#48787);
#12754=VERTEX_POINT('',#48788);
#12755=VERTEX_POINT('',#48790);
#12756=VERTEX_POINT('',#48792);
#12757=VERTEX_POINT('',#48796);
#12758=VERTEX_POINT('',#48798);
#12759=VERTEX_POINT('',#48802);
#12760=VERTEX_POINT('',#48804);
#12761=VERTEX_POINT('',#48808);
#12762=VERTEX_POINT('',#48810);
#12763=VERTEX_POINT('',#48814);
#12764=VERTEX_POINT('',#48816);
#12765=VERTEX_POINT('',#48820);
#12766=VERTEX_POINT('',#48822);
#12767=VERTEX_POINT('',#48830);
#12768=VERTEX_POINT('',#48831);
#12769=VERTEX_POINT('',#48833);
#12770=VERTEX_POINT('',#48835);
#12771=VERTEX_POINT('',#48839);
#12772=VERTEX_POINT('',#48841);
#12773=VERTEX_POINT('',#48845);
#12774=VERTEX_POINT('',#48847);
#12775=VERTEX_POINT('',#48855);
#12776=VERTEX_POINT('',#48856);
#12777=VERTEX_POINT('',#48858);
#12778=VERTEX_POINT('',#48860);
#12779=VERTEX_POINT('',#48864);
#12780=VERTEX_POINT('',#48866);
#12781=VERTEX_POINT('',#48870);
#12782=VERTEX_POINT('',#48872);
#12783=VERTEX_POINT('',#48880);
#12784=VERTEX_POINT('',#48881);
#12785=VERTEX_POINT('',#48883);
#12786=VERTEX_POINT('',#48885);
#12787=VERTEX_POINT('',#48889);
#12788=VERTEX_POINT('',#48891);
#12789=VERTEX_POINT('',#48895);
#12790=VERTEX_POINT('',#48897);
#12791=VERTEX_POINT('',#48905);
#12792=VERTEX_POINT('',#48906);
#12793=VERTEX_POINT('',#48908);
#12794=VERTEX_POINT('',#48910);
#12795=VERTEX_POINT('',#48914);
#12796=VERTEX_POINT('',#48916);
#12797=VERTEX_POINT('',#48920);
#12798=VERTEX_POINT('',#48922);
#12799=VERTEX_POINT('',#48930);
#12800=VERTEX_POINT('',#48931);
#12801=VERTEX_POINT('',#48933);
#12802=VERTEX_POINT('',#48935);
#12803=VERTEX_POINT('',#48939);
#12804=VERTEX_POINT('',#48941);
#12805=VERTEX_POINT('',#48945);
#12806=VERTEX_POINT('',#48947);
#12807=VERTEX_POINT('',#48955);
#12808=VERTEX_POINT('',#48956);
#12809=VERTEX_POINT('',#48958);
#12810=VERTEX_POINT('',#48960);
#12811=VERTEX_POINT('',#48964);
#12812=VERTEX_POINT('',#48966);
#12813=VERTEX_POINT('',#48970);
#12814=VERTEX_POINT('',#48972);
#12815=VERTEX_POINT('',#48980);
#12816=VERTEX_POINT('',#48981);
#12817=VERTEX_POINT('',#48983);
#12818=VERTEX_POINT('',#48985);
#12819=VERTEX_POINT('',#48989);
#12820=VERTEX_POINT('',#48991);
#12821=VERTEX_POINT('',#48995);
#12822=VERTEX_POINT('',#48997);
#12823=VERTEX_POINT('',#49005);
#12824=VERTEX_POINT('',#49006);
#12825=VERTEX_POINT('',#49008);
#12826=VERTEX_POINT('',#49010);
#12827=VERTEX_POINT('',#49014);
#12828=VERTEX_POINT('',#49016);
#12829=VERTEX_POINT('',#49020);
#12830=VERTEX_POINT('',#49022);
#12831=VERTEX_POINT('',#49030);
#12832=VERTEX_POINT('',#49031);
#12833=VERTEX_POINT('',#49033);
#12834=VERTEX_POINT('',#49035);
#12835=VERTEX_POINT('',#49039);
#12836=VERTEX_POINT('',#49041);
#12837=VERTEX_POINT('',#49045);
#12838=VERTEX_POINT('',#49047);
#12839=VERTEX_POINT('',#49055);
#12840=VERTEX_POINT('',#49056);
#12841=VERTEX_POINT('',#49058);
#12842=VERTEX_POINT('',#49060);
#12843=VERTEX_POINT('',#49064);
#12844=VERTEX_POINT('',#49066);
#12845=VERTEX_POINT('',#49070);
#12846=VERTEX_POINT('',#49072);
#12847=VERTEX_POINT('',#49080);
#12848=VERTEX_POINT('',#49081);
#12849=VERTEX_POINT('',#49083);
#12850=VERTEX_POINT('',#49085);
#12851=VERTEX_POINT('',#49089);
#12852=VERTEX_POINT('',#49091);
#12853=VERTEX_POINT('',#49095);
#12854=VERTEX_POINT('',#49097);
#12855=VERTEX_POINT('',#49105);
#12856=VERTEX_POINT('',#49108);
#12857=VERTEX_POINT('',#49112);
#12858=VERTEX_POINT('',#49115);
#12859=VERTEX_POINT('',#49119);
#12860=VERTEX_POINT('',#49123);
#12861=VERTEX_POINT('',#49126);
#12862=VERTEX_POINT('',#49130);
#12863=VERTEX_POINT('',#49259);
#12864=VERTEX_POINT('',#49260);
#12865=VERTEX_POINT('',#49262);
#12866=VERTEX_POINT('',#49329);
#12867=VERTEX_POINT('',#49331);
#12868=VERTEX_POINT('',#49367);
#12869=VERTEX_POINT('',#49369);
#12870=VERTEX_POINT('',#49372);
#12871=VERTEX_POINT('',#49530);
#12872=VERTEX_POINT('',#49533);
#12873=VERTEX_POINT('',#49534);
#12874=VERTEX_POINT('',#49543);
#12875=VERTEX_POINT('',#49603);
#12876=VERTEX_POINT('',#49606);
#12877=VERTEX_POINT('',#49610);
#12878=VERTEX_POINT('',#49615);
#12879=VERTEX_POINT('',#49618);
#12880=VERTEX_POINT('',#49622);
#12881=VERTEX_POINT('',#49626);
#12882=VERTEX_POINT('',#49631);
#12883=VERTEX_POINT('',#49966);
#12884=VERTEX_POINT('',#49968);
#12885=VERTEX_POINT('',#50004);
#12886=VERTEX_POINT('',#50005);
#12887=VERTEX_POINT('',#50007);
#12888=VERTEX_POINT('',#50009);
#12889=VERTEX_POINT('',#50013);
#12890=VERTEX_POINT('',#50015);
#12891=VERTEX_POINT('',#50019);
#12892=VERTEX_POINT('',#50021);
#12893=VERTEX_POINT('',#50025);
#12894=VERTEX_POINT('',#50026);
#12895=VERTEX_POINT('',#50028);
#12896=VERTEX_POINT('',#50030);
#12897=VERTEX_POINT('',#50034);
#12898=VERTEX_POINT('',#50036);
#12899=VERTEX_POINT('',#50040);
#12900=VERTEX_POINT('',#50042);
#12901=VERTEX_POINT('',#50046);
#12902=VERTEX_POINT('',#50047);
#12903=VERTEX_POINT('',#50049);
#12904=VERTEX_POINT('',#50051);
#12905=VERTEX_POINT('',#50053);
#12906=VERTEX_POINT('',#50057);
#12907=VERTEX_POINT('',#50059);
#12908=VERTEX_POINT('',#50061);
#12909=VERTEX_POINT('',#50063);
#12910=VERTEX_POINT('',#50065);
#12911=VERTEX_POINT('',#50067);
#12912=VERTEX_POINT('',#50071);
#12913=VERTEX_POINT('',#50075);
#12914=VERTEX_POINT('',#50077);
#12915=VERTEX_POINT('',#50079);
#12916=VERTEX_POINT('',#50083);
#12917=VERTEX_POINT('',#50087);
#12918=VERTEX_POINT('',#50089);
#12919=VERTEX_POINT('',#50091);
#12920=VERTEX_POINT('',#50096);
#12921=VERTEX_POINT('',#50098);
#12922=VERTEX_POINT('',#50100);
#12923=VERTEX_POINT('',#50102);
#12924=VERTEX_POINT('',#50106);
#12925=VERTEX_POINT('',#50108);
#12926=VERTEX_POINT('',#50110);
#12927=VERTEX_POINT('',#50112);
#12928=VERTEX_POINT('',#50116);
#12929=VERTEX_POINT('',#50118);
#12930=VERTEX_POINT('',#50120);
#12931=VERTEX_POINT('',#50124);
#12932=VERTEX_POINT('',#50126);
#12933=VERTEX_POINT('',#50130);
#12934=VERTEX_POINT('',#50132);
#12935=VERTEX_POINT('',#50134);
#12936=VERTEX_POINT('',#50138);
#12937=VERTEX_POINT('',#50142);
#12938=VERTEX_POINT('',#50144);
#12939=VERTEX_POINT('',#50148);
#12940=VERTEX_POINT('',#50149);
#12941=VERTEX_POINT('',#50151);
#12942=VERTEX_POINT('',#50153);
#12943=VERTEX_POINT('',#50155);
#12944=VERTEX_POINT('',#50159);
#12945=VERTEX_POINT('',#50161);
#12946=VERTEX_POINT('',#50163);
#12947=VERTEX_POINT('',#50165);
#12948=VERTEX_POINT('',#50167);
#12949=VERTEX_POINT('',#50169);
#12950=VERTEX_POINT('',#50173);
#12951=VERTEX_POINT('',#50177);
#12952=VERTEX_POINT('',#50179);
#12953=VERTEX_POINT('',#50181);
#12954=VERTEX_POINT('',#50186);
#12955=VERTEX_POINT('',#50188);
#12956=VERTEX_POINT('',#50192);
#12957=VERTEX_POINT('',#50197);
#12958=VERTEX_POINT('',#50199);
#12959=VERTEX_POINT('',#50203);
#12960=VERTEX_POINT('',#50207);
#12961=VERTEX_POINT('',#50211);
#12962=VERTEX_POINT('',#50213);
#12963=VERTEX_POINT('',#50215);
#12964=VERTEX_POINT('',#50217);
#12965=VERTEX_POINT('',#50221);
#12966=VERTEX_POINT('',#50223);
#12967=VERTEX_POINT('',#50225);
#12968=VERTEX_POINT('',#50227);
#12969=VERTEX_POINT('',#50231);
#12970=VERTEX_POINT('',#50233);
#12971=VERTEX_POINT('',#50235);
#12972=VERTEX_POINT('',#50239);
#12973=VERTEX_POINT('',#50241);
#12974=VERTEX_POINT('',#50245);
#12975=VERTEX_POINT('',#50247);
#12976=VERTEX_POINT('',#50249);
#12977=VERTEX_POINT('',#50253);
#12978=VERTEX_POINT('',#50255);
#12979=VERTEX_POINT('',#50259);
#12980=VERTEX_POINT('',#50260);
#12981=VERTEX_POINT('',#50262);
#12982=VERTEX_POINT('',#50264);
#12983=VERTEX_POINT('',#50268);
#12984=VERTEX_POINT('',#50269);
#12985=VERTEX_POINT('',#50274);
#12986=VERTEX_POINT('',#50275);
#12987=VERTEX_POINT('',#50280);
#12988=VERTEX_POINT('',#50281);
#12989=VERTEX_POINT('',#50286);
#12990=VERTEX_POINT('',#50287);
#12991=VERTEX_POINT('',#50292);
#12992=VERTEX_POINT('',#50293);
#12993=VERTEX_POINT('',#50298);
#12994=VERTEX_POINT('',#50299);
#12995=VERTEX_POINT('',#50307);
#12996=VERTEX_POINT('',#50309);
#12997=VERTEX_POINT('',#50313);
#12998=VERTEX_POINT('',#50317);
#12999=VERTEX_POINT('',#50321);
#13000=VERTEX_POINT('',#50325);
#13001=VERTEX_POINT('',#50327);
#13002=VERTEX_POINT('',#50330);
#13003=VERTEX_POINT('',#50334);
#13004=VERTEX_POINT('',#50338);
#13005=VERTEX_POINT('',#50340);
#13006=VERTEX_POINT('',#50346);
#13007=VERTEX_POINT('',#50348);
#13008=VERTEX_POINT('',#50351);
#13009=VERTEX_POINT('',#50353);
#13010=VERTEX_POINT('',#50360);
#13011=VERTEX_POINT('',#50362);
#13012=VERTEX_POINT('',#50364);
#13013=VERTEX_POINT('',#50372);
#13014=VERTEX_POINT('',#50374);
#13015=VERTEX_POINT('',#50377);
#13016=VERTEX_POINT('',#50381);
#13017=VERTEX_POINT('',#50387);
#13018=VERTEX_POINT('',#50389);
#13019=VERTEX_POINT('',#50393);
#13020=VERTEX_POINT('',#50398);
#13021=VERTEX_POINT('',#50403);
#13022=VERTEX_POINT('',#50407);
#13023=VERTEX_POINT('',#50411);
#13024=VERTEX_POINT('',#50416);
#13025=VERTEX_POINT('',#50419);
#13026=VERTEX_POINT('',#50423);
#13027=VERTEX_POINT('',#50429);
#13028=VERTEX_POINT('',#50433);
#13029=VERTEX_POINT('',#50439);
#13030=VERTEX_POINT('',#50443);
#13031=VERTEX_POINT('',#50447);
#13032=VERTEX_POINT('',#50451);
#13033=VERTEX_POINT('',#50455);
#13034=VERTEX_POINT('',#50457);
#13035=VERTEX_POINT('',#50461);
#13036=VERTEX_POINT('',#50462);
#13037=VERTEX_POINT('',#50467);
#13038=VERTEX_POINT('',#50468);
#13039=VERTEX_POINT('',#50473);
#13040=VERTEX_POINT('',#50474);
#13041=VERTEX_POINT('',#50482);
#13042=VERTEX_POINT('',#50484);
#13043=VERTEX_POINT('',#50486);
#13044=VERTEX_POINT('',#50488);
#13045=VERTEX_POINT('',#50490);
#13046=VERTEX_POINT('',#50493);
#13047=VERTEX_POINT('',#50495);
#13048=VERTEX_POINT('',#50498);
#13049=VERTEX_POINT('',#50502);
#13050=VERTEX_POINT('',#50506);
#13051=VERTEX_POINT('',#50510);
#13052=VERTEX_POINT('',#50514);
#13053=VERTEX_POINT('',#50524);
#13054=VERTEX_POINT('',#50539);
#13055=VERTEX_POINT('',#50543);
#13056=VERTEX_POINT('',#50547);
#13057=VERTEX_POINT('',#50561);
#13058=VERTEX_POINT('',#50564);
#13059=VERTEX_POINT('',#50565);
#13060=VERTEX_POINT('',#50578);
#13061=VERTEX_POINT('',#50625);
#13062=VERTEX_POINT('',#50704);
#13063=VERTEX_POINT('',#50705);
#13064=VERTEX_POINT('',#50712);
#13065=VERTEX_POINT('',#50732);
#13066=VERTEX_POINT('',#50739);
#13067=VERTEX_POINT('',#50746);
#13068=VERTEX_POINT('',#50780);
#13069=VERTEX_POINT('',#50783);
#13070=VERTEX_POINT('',#50784);
#13071=VERTEX_POINT('',#50786);
#13072=VERTEX_POINT('',#50793);
#13073=VERTEX_POINT('',#50805);
#13074=VERTEX_POINT('',#50812);
#13075=VERTEX_POINT('',#50839);
#13076=VERTEX_POINT('',#50864);
#13077=VERTEX_POINT('',#50944);
#13078=VERTEX_POINT('',#56992);
#13079=VERTEX_POINT('',#56993);
#13080=VERTEX_POINT('',#56995);
#13081=VERTEX_POINT('',#57006);
#13082=VERTEX_POINT('',#57019);
#13083=VERTEX_POINT('',#57020);
#13084=VERTEX_POINT('',#57067);
#13085=VERTEX_POINT('',#57068);
#13086=VERTEX_POINT('',#57115);
#13087=VERTEX_POINT('',#57116);
#13088=VERTEX_POINT('',#57169);
#13089=VERTEX_POINT('',#57170);
#13090=VERTEX_POINT('',#57217);
#13091=VERTEX_POINT('',#57218);
#13092=VERTEX_POINT('',#57265);
#13093=VERTEX_POINT('',#57266);
#13094=VERTEX_POINT('',#57319);
#13095=VERTEX_POINT('',#57320);
#13096=VERTEX_POINT('',#57367);
#13097=VERTEX_POINT('',#57368);
#13098=VERTEX_POINT('',#57415);
#13099=VERTEX_POINT('',#57416);
#13100=VERTEX_POINT('',#57469);
#13101=VERTEX_POINT('',#57470);
#13102=VERTEX_POINT('',#57517);
#13103=VERTEX_POINT('',#57518);
#13104=VERTEX_POINT('',#57520);
#13105=VERTEX_POINT('',#57526);
#13106=VERTEX_POINT('',#57533);
#13107=VERTEX_POINT('',#57534);
#13108=VERTEX_POINT('',#57558);
#13109=VERTEX_POINT('',#57559);
#13110=VERTEX_POINT('',#57583);
#13111=VERTEX_POINT('',#57584);
#13112=VERTEX_POINT('',#57608);
#13113=VERTEX_POINT('',#57609);
#13114=VERTEX_POINT('',#57632);
#13115=VERTEX_POINT('',#57633);
#13116=VERTEX_POINT('',#57657);
#13117=VERTEX_POINT('',#57658);
#13118=VERTEX_POINT('',#57682);
#13119=VERTEX_POINT('',#57683);
#13120=VERTEX_POINT('',#57706);
#13121=VERTEX_POINT('',#57707);
#13122=VERTEX_POINT('',#57731);
#13123=VERTEX_POINT('',#57732);
#13124=VERTEX_POINT('',#57756);
#13125=VERTEX_POINT('',#57757);
#13126=VERTEX_POINT('',#57780);
#13127=VERTEX_POINT('',#57781);
#13128=VERTEX_POINT('',#57783);
#13129=VERTEX_POINT('',#57790);
#13130=VERTEX_POINT('',#57803);
#13131=VERTEX_POINT('',#57818);
#13132=VERTEX_POINT('',#57831);
#13133=VERTEX_POINT('',#57840);
#13134=VERTEX_POINT('',#57847);
#13135=VERTEX_POINT('',#57860);
#13136=VERTEX_POINT('',#57875);
#13137=VERTEX_POINT('',#57895);
#13138=VERTEX_POINT('',#57906);
#13139=VERTEX_POINT('',#57908);
#13140=VERTEX_POINT('',#57976);
#13141=VERTEX_POINT('',#58046);
#13142=VERTEX_POINT('',#58355);
#13143=VERTEX_POINT('',#58449);
#13144=VERTEX_POINT('',#58845);
#13145=VERTEX_POINT('',#58849);
#13146=VERTEX_POINT('',#58856);
#13147=VERTEX_POINT('',#58857);
#13148=VERTEX_POINT('',#58859);
#13149=VERTEX_POINT('',#58861);
#13150=VERTEX_POINT('',#58863);
#13151=VERTEX_POINT('',#58865);
#13152=VERTEX_POINT('',#58869);
#13153=VERTEX_POINT('',#58871);
#13154=VERTEX_POINT('',#58875);
#13155=VERTEX_POINT('',#58877);
#13156=VERTEX_POINT('',#58879);
#13157=VERTEX_POINT('',#58883);
#13158=VERTEX_POINT('',#58885);
#13159=VERTEX_POINT('',#58887);
#13160=VERTEX_POINT('',#58891);
#13161=VERTEX_POINT('',#58893);
#13162=VERTEX_POINT('',#58895);
#13163=VERTEX_POINT('',#58897);
#13164=VERTEX_POINT('',#58899);
#13165=VERTEX_POINT('',#58901);
#13166=VERTEX_POINT('',#58903);
#13167=VERTEX_POINT('',#58907);
#13168=VERTEX_POINT('',#58911);
#13169=VERTEX_POINT('',#58913);
#13170=VERTEX_POINT('',#58915);
#13171=VERTEX_POINT('',#58919);
#13172=VERTEX_POINT('',#58921);
#13173=VERTEX_POINT('',#58925);
#13174=VERTEX_POINT('',#58927);
#13175=VERTEX_POINT('',#58931);
#13176=VERTEX_POINT('',#58932);
#13177=VERTEX_POINT('',#58934);
#13178=VERTEX_POINT('',#58936);
#13179=VERTEX_POINT('',#58938);
#13180=VERTEX_POINT('',#58940);
#13181=VERTEX_POINT('',#58944);
#13182=VERTEX_POINT('',#58946);
#13183=VERTEX_POINT('',#58951);
#13184=VERTEX_POINT('',#58957);
#13185=VERTEX_POINT('',#58961);
#13186=VERTEX_POINT('',#58963);
#13187=VERTEX_POINT('',#58965);
#13188=VERTEX_POINT('',#58969);
#13189=VERTEX_POINT('',#58971);
#13190=VERTEX_POINT('',#58975);
#13191=VERTEX_POINT('',#58979);
#13192=VERTEX_POINT('',#58986);
#13193=VERTEX_POINT('',#58987);
#13194=VERTEX_POINT('',#58990);
#13195=VERTEX_POINT('',#58994);
#13196=VERTEX_POINT('',#58996);
#13197=VERTEX_POINT('',#59001);
#13198=VERTEX_POINT('',#59006);
#13199=VERTEX_POINT('',#59008);
#13200=VERTEX_POINT('',#59012);
#13201=VERTEX_POINT('',#59014);
#13202=VERTEX_POINT('',#59018);
#13203=VERTEX_POINT('',#59020);
#13204=VERTEX_POINT('',#59024);
#13205=VERTEX_POINT('',#59025);
#13206=VERTEX_POINT('',#59032);
#13207=VERTEX_POINT('',#59039);
#13208=VERTEX_POINT('',#59040);
#13209=VERTEX_POINT('',#59045);
#13210=VERTEX_POINT('',#59051);
#13211=VERTEX_POINT('',#59055);
#13212=VERTEX_POINT('',#59057);
#13213=VERTEX_POINT('',#59079);
#13214=VERTEX_POINT('',#59080);
#13215=VERTEX_POINT('',#59082);
#13216=VERTEX_POINT('',#59093);
#13217=VERTEX_POINT('',#59106);
#13218=VERTEX_POINT('',#59107);
#13219=VERTEX_POINT('',#59172);
#13220=VERTEX_POINT('',#59173);
#13221=VERTEX_POINT('',#59232);
#13222=VERTEX_POINT('',#59233);
#13223=VERTEX_POINT('',#59292);
#13224=VERTEX_POINT('',#59293);
#13225=VERTEX_POINT('',#59355);
#13226=VERTEX_POINT('',#59356);
#13227=VERTEX_POINT('',#59415);
#13228=VERTEX_POINT('',#59416);
#13229=VERTEX_POINT('',#59475);
#13230=VERTEX_POINT('',#59476);
#13231=VERTEX_POINT('',#59538);
#13232=VERTEX_POINT('',#59539);
#13233=VERTEX_POINT('',#59598);
#13234=VERTEX_POINT('',#59599);
#13235=VERTEX_POINT('',#59664);
#13236=VERTEX_POINT('',#59665);
#13237=VERTEX_POINT('',#59733);
#13238=VERTEX_POINT('',#59734);
#13239=VERTEX_POINT('',#59799);
#13240=VERTEX_POINT('',#59800);
#13241=VERTEX_POINT('',#59859);
#13242=VERTEX_POINT('',#59860);
#13243=VERTEX_POINT('',#59922);
#13244=VERTEX_POINT('',#59923);
#13245=VERTEX_POINT('',#59988);
#13246=VERTEX_POINT('',#59989);
#13247=VERTEX_POINT('',#60048);
#13248=VERTEX_POINT('',#60049);
#13249=VERTEX_POINT('',#60102);
#13250=VERTEX_POINT('',#60103);
#13251=VERTEX_POINT('',#60156);
#13252=VERTEX_POINT('',#60157);
#13253=VERTEX_POINT('',#60216);
#13254=VERTEX_POINT('',#60217);
#13255=VERTEX_POINT('',#60282);
#13256=VERTEX_POINT('',#60283);
#13257=VERTEX_POINT('',#60348);
#13258=VERTEX_POINT('',#60349);
#13259=VERTEX_POINT('',#60417);
#13260=VERTEX_POINT('',#60418);
#13261=VERTEX_POINT('',#60477);
#13262=VERTEX_POINT('',#60478);
#13263=VERTEX_POINT('',#60540);
#13264=VERTEX_POINT('',#60541);
#13265=VERTEX_POINT('',#60606);
#13266=VERTEX_POINT('',#60607);
#13267=VERTEX_POINT('',#60672);
#13268=VERTEX_POINT('',#60673);
#13269=VERTEX_POINT('',#60726);
#13270=VERTEX_POINT('',#60727);
#13271=VERTEX_POINT('',#60780);
#13272=VERTEX_POINT('',#60781);
#13273=VERTEX_POINT('',#60843);
#13274=VERTEX_POINT('',#60844);
#13275=VERTEX_POINT('',#60909);
#13276=VERTEX_POINT('',#60910);
#13277=VERTEX_POINT('',#60960);
#13278=VERTEX_POINT('',#60961);
#13279=VERTEX_POINT('',#61023);
#13280=VERTEX_POINT('',#61024);
#13281=VERTEX_POINT('',#61077);
#13282=VERTEX_POINT('',#61078);
#13283=VERTEX_POINT('',#61140);
#13284=VERTEX_POINT('',#61141);
#13285=VERTEX_POINT('',#61209);
#13286=VERTEX_POINT('',#61210);
#13287=VERTEX_POINT('',#61272);
#13288=VERTEX_POINT('',#61273);
#13289=VERTEX_POINT('',#61326);
#13290=VERTEX_POINT('',#61327);
#13291=VERTEX_POINT('',#61386);
#13292=VERTEX_POINT('',#61387);
#13293=VERTEX_POINT('',#61446);
#13294=VERTEX_POINT('',#61447);
#13295=VERTEX_POINT('',#61506);
#13296=VERTEX_POINT('',#61507);
#13297=VERTEX_POINT('',#61569);
#13298=VERTEX_POINT('',#61570);
#13299=VERTEX_POINT('',#61623);
#13300=VERTEX_POINT('',#61624);
#13301=VERTEX_POINT('',#61677);
#13302=VERTEX_POINT('',#61678);
#13303=VERTEX_POINT('',#61743);
#13304=VERTEX_POINT('',#61744);
#13305=VERTEX_POINT('',#61812);
#13306=VERTEX_POINT('',#61813);
#13307=VERTEX_POINT('',#61875);
#13308=VERTEX_POINT('',#61876);
#13309=VERTEX_POINT('',#61929);
#13310=VERTEX_POINT('',#61930);
#13311=VERTEX_POINT('',#61995);
#13312=VERTEX_POINT('',#61996);
#13313=VERTEX_POINT('',#62061);
#13314=VERTEX_POINT('',#62062);
#13315=VERTEX_POINT('',#62121);
#13316=VERTEX_POINT('',#62122);
#13317=VERTEX_POINT('',#62181);
#13318=VERTEX_POINT('',#62182);
#13319=VERTEX_POINT('',#62235);
#13320=VERTEX_POINT('',#62236);
#13321=VERTEX_POINT('',#62292);
#13322=VERTEX_POINT('',#62293);
#13323=VERTEX_POINT('',#62358);
#13324=VERTEX_POINT('',#62359);
#13325=VERTEX_POINT('',#62427);
#13326=VERTEX_POINT('',#62428);
#13327=VERTEX_POINT('',#62490);
#13328=VERTEX_POINT('',#62491);
#13329=VERTEX_POINT('',#62544);
#13330=VERTEX_POINT('',#62545);
#13331=VERTEX_POINT('',#62610);
#13332=VERTEX_POINT('',#62611);
#13333=VERTEX_POINT('',#62676);
#13334=VERTEX_POINT('',#62677);
#13335=VERTEX_POINT('',#62679);
#13336=VERTEX_POINT('',#62735);
#13337=VERTEX_POINT('',#62736);
#13338=VERTEX_POINT('',#62738);
#13339=VERTEX_POINT('',#62755);
#13340=VERTEX_POINT('',#62766);
#13341=VERTEX_POINT('',#62767);
#13342=VERTEX_POINT('',#62796);
#13343=VERTEX_POINT('',#62797);
#13344=VERTEX_POINT('',#62826);
#13345=VERTEX_POINT('',#62827);
#13346=VERTEX_POINT('',#62871);
#13347=VERTEX_POINT('',#62872);
#13348=VERTEX_POINT('',#62916);
#13349=VERTEX_POINT('',#62917);
#13350=VERTEX_POINT('',#62946);
#13351=VERTEX_POINT('',#62947);
#13352=VERTEX_POINT('',#62976);
#13353=VERTEX_POINT('',#62977);
#13354=VERTEX_POINT('',#63005);
#13355=VERTEX_POINT('',#63006);
#13356=VERTEX_POINT('',#63047);
#13357=VERTEX_POINT('',#63048);
#13358=VERTEX_POINT('',#63077);
#13359=VERTEX_POINT('',#63078);
#13360=VERTEX_POINT('',#63119);
#13361=VERTEX_POINT('',#63120);
#13362=VERTEX_POINT('',#63149);
#13363=VERTEX_POINT('',#63150);
#13364=VERTEX_POINT('',#63179);
#13365=VERTEX_POINT('',#63180);
#13366=VERTEX_POINT('',#63221);
#13367=VERTEX_POINT('',#63222);
#13368=VERTEX_POINT('',#63263);
#13369=VERTEX_POINT('',#63264);
#13370=VERTEX_POINT('',#63293);
#13371=VERTEX_POINT('',#63294);
#13372=VERTEX_POINT('',#63323);
#13373=VERTEX_POINT('',#63324);
#13374=VERTEX_POINT('',#63365);
#13375=VERTEX_POINT('',#63366);
#13376=VERTEX_POINT('',#63419);
#13377=VERTEX_POINT('',#63420);
#13378=VERTEX_POINT('',#63449);
#13379=VERTEX_POINT('',#63450);
#13380=VERTEX_POINT('',#63491);
#13381=VERTEX_POINT('',#63492);
#13382=VERTEX_POINT('',#63520);
#13383=VERTEX_POINT('',#63521);
#13384=VERTEX_POINT('',#63550);
#13385=VERTEX_POINT('',#63551);
#13386=VERTEX_POINT('',#63593);
#13387=VERTEX_POINT('',#63594);
#13388=VERTEX_POINT('',#63635);
#13389=VERTEX_POINT('',#63636);
#13390=VERTEX_POINT('',#63665);
#13391=VERTEX_POINT('',#63666);
#13392=VERTEX_POINT('',#63694);
#13393=VERTEX_POINT('',#63695);
#13394=VERTEX_POINT('',#63736);
#13395=VERTEX_POINT('',#63737);
#13396=VERTEX_POINT('',#63793);
#13397=VERTEX_POINT('',#63794);
#13398=VERTEX_POINT('',#63822);
#13399=VERTEX_POINT('',#63823);
#13400=VERTEX_POINT('',#63849);
#13401=VERTEX_POINT('',#63850);
#13402=VERTEX_POINT('',#63878);
#13403=VERTEX_POINT('',#63879);
#13404=VERTEX_POINT('',#63923);
#13405=VERTEX_POINT('',#63924);
#13406=VERTEX_POINT('',#63966);
#13407=VERTEX_POINT('',#63967);
#13408=VERTEX_POINT('',#64011);
#13409=VERTEX_POINT('',#64012);
#13410=VERTEX_POINT('',#64041);
#13411=VERTEX_POINT('',#64042);
#13412=VERTEX_POINT('',#64071);
#13413=VERTEX_POINT('',#64072);
#13414=VERTEX_POINT('',#64100);
#13415=VERTEX_POINT('',#64101);
#13416=VERTEX_POINT('',#64146);
#13417=VERTEX_POINT('',#64147);
#13418=VERTEX_POINT('',#64176);
#13419=VERTEX_POINT('',#64177);
#13420=VERTEX_POINT('',#64206);
#13421=VERTEX_POINT('',#64207);
#13422=VERTEX_POINT('',#64235);
#13423=VERTEX_POINT('',#64236);
#13424=VERTEX_POINT('',#64277);
#13425=VERTEX_POINT('',#64278);
#13426=VERTEX_POINT('',#64320);
#13427=VERTEX_POINT('',#64321);
#13428=VERTEX_POINT('',#64362);
#13429=VERTEX_POINT('',#64363);
#13430=VERTEX_POINT('',#64392);
#13431=VERTEX_POINT('',#64393);
#13432=VERTEX_POINT('',#64422);
#13433=VERTEX_POINT('',#64423);
#13434=VERTEX_POINT('',#64451);
#13435=VERTEX_POINT('',#64452);
#13436=VERTEX_POINT('',#64493);
#13437=VERTEX_POINT('',#64494);
#13438=VERTEX_POINT('',#64524);
#13439=VERTEX_POINT('',#64525);
#13440=VERTEX_POINT('',#64554);
#13441=VERTEX_POINT('',#64555);
#13442=VERTEX_POINT('',#64596);
#13443=VERTEX_POINT('',#64597);
#13444=VERTEX_POINT('',#64638);
#13445=VERTEX_POINT('',#64639);
#13446=VERTEX_POINT('',#64669);
#13447=VERTEX_POINT('',#64670);
#13448=VERTEX_POINT('',#64711);
#13449=VERTEX_POINT('',#64712);
#13450=VERTEX_POINT('',#64741);
#13451=VERTEX_POINT('',#64742);
#13452=VERTEX_POINT('',#64770);
#13453=VERTEX_POINT('',#64771);
#13454=VERTEX_POINT('',#64800);
#13455=VERTEX_POINT('',#64801);
#13456=VERTEX_POINT('',#64847);
#13457=VERTEX_POINT('',#64848);
#13458=VERTEX_POINT('',#64852);
#13459=VERTEX_POINT('',#64854);
#13460=VERTEX_POINT('',#64865);
#13461=VERTEX_POINT('',#64869);
#13462=VERTEX_POINT('',#64880);
#13463=VERTEX_POINT('',#64884);
#13464=VERTEX_POINT('',#64895);
#13465=VERTEX_POINT('',#64899);
#13466=VERTEX_POINT('',#64910);
#13467=VERTEX_POINT('',#64914);
#13468=VERTEX_POINT('',#64925);
#13469=VERTEX_POINT('',#64929);
#13470=VERTEX_POINT('',#64940);
#13471=VERTEX_POINT('',#64944);
#13472=VERTEX_POINT('',#64955);
#13473=VERTEX_POINT('',#64959);
#13474=VERTEX_POINT('',#64982);
#13475=VERTEX_POINT('',#64983);
#13476=VERTEX_POINT('',#64987);
#13477=VERTEX_POINT('',#64989);
#13478=VERTEX_POINT('',#65000);
#13479=VERTEX_POINT('',#65004);
#13480=VERTEX_POINT('',#65015);
#13481=VERTEX_POINT('',#65019);
#13482=VERTEX_POINT('',#65030);
#13483=VERTEX_POINT('',#65034);
#13484=VERTEX_POINT('',#65045);
#13485=VERTEX_POINT('',#65049);
#13486=VERTEX_POINT('',#65060);
#13487=VERTEX_POINT('',#65064);
#13488=VERTEX_POINT('',#65075);
#13489=VERTEX_POINT('',#65079);
#13490=VERTEX_POINT('',#65102);
#13491=VERTEX_POINT('',#65103);
#13492=VERTEX_POINT('',#65107);
#13493=VERTEX_POINT('',#65109);
#13494=VERTEX_POINT('',#65120);
#13495=VERTEX_POINT('',#65124);
#13496=VERTEX_POINT('',#65135);
#13497=VERTEX_POINT('',#65139);
#13498=VERTEX_POINT('',#65150);
#13499=VERTEX_POINT('',#65154);
#13500=VERTEX_POINT('',#65165);
#13501=VERTEX_POINT('',#65169);
#13502=VERTEX_POINT('',#65180);
#13503=VERTEX_POINT('',#65184);
#13504=VERTEX_POINT('',#65195);
#13505=VERTEX_POINT('',#65199);
#13506=VERTEX_POINT('',#65210);
#13507=VERTEX_POINT('',#65214);
#13508=VERTEX_POINT('',#65225);
#13509=VERTEX_POINT('',#65229);
#13510=VERTEX_POINT('',#65240);
#13511=VERTEX_POINT('',#65244);
#13512=VERTEX_POINT('',#65255);
#13513=VERTEX_POINT('',#65259);
#13514=VERTEX_POINT('',#65270);
#13515=VERTEX_POINT('',#65274);
#13516=VERTEX_POINT('',#65285);
#13517=VERTEX_POINT('',#65289);
#13518=VERTEX_POINT('',#65300);
#13519=VERTEX_POINT('',#65304);
#13520=VERTEX_POINT('',#65315);
#13521=VERTEX_POINT('',#65319);
#13522=VERTEX_POINT('',#65338);
#13523=VERTEX_POINT('',#65339);
#13524=VERTEX_POINT('',#65341);
#13525=VERTEX_POINT('',#65343);
#13526=VERTEX_POINT('',#65347);
#13527=VERTEX_POINT('',#65349);
#13528=VERTEX_POINT('',#65353);
#13529=VERTEX_POINT('',#65355);
#13530=VERTEX_POINT('',#65368);
#13531=VERTEX_POINT('',#65369);
#13532=VERTEX_POINT('',#65373);
#13533=VERTEX_POINT('',#65375);
#13534=VERTEX_POINT('',#65386);
#13535=VERTEX_POINT('',#65390);
#13536=VERTEX_POINT('',#65401);
#13537=VERTEX_POINT('',#65405);
#13538=VERTEX_POINT('',#65416);
#13539=VERTEX_POINT('',#65420);
#13540=VERTEX_POINT('',#65431);
#13541=VERTEX_POINT('',#65435);
#13542=VERTEX_POINT('',#65446);
#13543=VERTEX_POINT('',#65450);
#13544=VERTEX_POINT('',#65461);
#13545=VERTEX_POINT('',#65465);
#13546=VERTEX_POINT('',#65476);
#13547=VERTEX_POINT('',#65480);
#13548=VERTEX_POINT('',#65503);
#13549=VERTEX_POINT('',#65504);
#13550=VERTEX_POINT('',#65508);
#13551=VERTEX_POINT('',#65510);
#13552=VERTEX_POINT('',#65521);
#13553=VERTEX_POINT('',#65525);
#13554=VERTEX_POINT('',#65536);
#13555=VERTEX_POINT('',#65540);
#13556=VERTEX_POINT('',#65551);
#13557=VERTEX_POINT('',#65555);
#13558=VERTEX_POINT('',#65566);
#13559=VERTEX_POINT('',#65570);
#13560=VERTEX_POINT('',#65581);
#13561=VERTEX_POINT('',#65585);
#13562=VERTEX_POINT('',#65596);
#13563=VERTEX_POINT('',#65600);
#13564=VERTEX_POINT('',#65623);
#13565=VERTEX_POINT('',#65624);
#13566=VERTEX_POINT('',#65628);
#13567=VERTEX_POINT('',#65630);
#13568=VERTEX_POINT('',#65641);
#13569=VERTEX_POINT('',#65645);
#13570=VERTEX_POINT('',#65656);
#13571=VERTEX_POINT('',#65660);
#13572=VERTEX_POINT('',#65671);
#13573=VERTEX_POINT('',#65675);
#13574=VERTEX_POINT('',#65686);
#13575=VERTEX_POINT('',#65690);
#13576=VERTEX_POINT('',#65701);
#13577=VERTEX_POINT('',#65705);
#13578=VERTEX_POINT('',#65716);
#13579=VERTEX_POINT('',#65720);
#13580=VERTEX_POINT('',#65731);
#13581=VERTEX_POINT('',#65735);
#13582=VERTEX_POINT('',#65746);
#13583=VERTEX_POINT('',#65750);
#13584=VERTEX_POINT('',#65761);
#13585=VERTEX_POINT('',#65765);
#13586=VERTEX_POINT('',#65776);
#13587=VERTEX_POINT('',#65780);
#13588=VERTEX_POINT('',#65791);
#13589=VERTEX_POINT('',#65795);
#13590=VERTEX_POINT('',#65806);
#13591=VERTEX_POINT('',#65810);
#13592=VERTEX_POINT('',#65821);
#13593=VERTEX_POINT('',#65825);
#13594=VERTEX_POINT('',#65836);
#13595=VERTEX_POINT('',#65840);
#13596=VERTEX_POINT('',#65936);
#13597=VERTEX_POINT('',#65938);
#13598=VERTEX_POINT('',#68172);
#13599=VERTEX_POINT('',#68258);
#13600=VERTEX_POINT('',#68261);
#13601=VERTEX_POINT('',#70503);
#13602=VERTEX_POINT('',#70508);
#13603=VERTEX_POINT('',#70509);
#13604=VERTEX_POINT('',#70511);
#13605=VERTEX_POINT('',#70513);
#13606=VERTEX_POINT('',#70515);
#13607=VERTEX_POINT('',#70517);
#13608=VERTEX_POINT('',#70522);
#13609=VERTEX_POINT('',#70523);
#13610=VERTEX_POINT('',#70527);
#13611=VERTEX_POINT('',#70531);
#13612=VERTEX_POINT('',#70535);
#13613=VERTEX_POINT('',#70539);
#13614=VERTEX_POINT('',#70543);
#13615=VERTEX_POINT('',#70546);
#13616=VERTEX_POINT('',#70567);
#13617=VERTEX_POINT('',#70573);
#13618=VERTEX_POINT('',#70575);
#13619=VERTEX_POINT('',#70579);
#13620=VERTEX_POINT('',#70583);
#13621=VERTEX_POINT('',#70586);
#13622=VERTEX_POINT('',#70590);
#13623=VERTEX_POINT('',#70593);
#13624=VERTEX_POINT('',#70595);
#13625=VERTEX_POINT('',#70599);
#13626=VERTEX_POINT('',#70603);
#13627=VERTEX_POINT('',#70607);
#13628=VERTEX_POINT('',#70611);
#13629=VERTEX_POINT('',#70615);
#13630=VERTEX_POINT('',#70623);
#13631=VERTEX_POINT('',#70625);
#13632=VERTEX_POINT('',#70631);
#13633=VERTEX_POINT('',#70637);
#13634=VERTEX_POINT('',#70643);
#13635=VERTEX_POINT('',#70647);
#13636=VERTEX_POINT('',#70652);
#13637=VERTEX_POINT('',#70666);
#13638=VERTEX_POINT('',#70668);
#13639=VERTEX_POINT('',#70672);
#13640=VERTEX_POINT('',#70675);
#13641=VERTEX_POINT('',#70679);
#13642=VERTEX_POINT('',#70683);
#13643=VERTEX_POINT('',#70689);
#13644=VERTEX_POINT('',#70691);
#13645=VERTEX_POINT('',#70693);
#13646=VERTEX_POINT('',#70697);
#13647=VERTEX_POINT('',#70699);
#13648=VERTEX_POINT('',#70704);
#13649=VERTEX_POINT('',#70706);
#13650=VERTEX_POINT('',#70710);
#13651=VERTEX_POINT('',#70714);
#13652=VERTEX_POINT('',#70716);
#13653=VERTEX_POINT('',#70720);
#13654=VERTEX_POINT('',#70724);
#13655=VERTEX_POINT('',#70725);
#13656=VERTEX_POINT('',#70727);
#13657=VERTEX_POINT('',#70729);
#13658=VERTEX_POINT('',#70733);
#13659=VERTEX_POINT('',#70737);
#13660=VERTEX_POINT('',#70738);
#13661=VERTEX_POINT('',#70740);
#13662=VERTEX_POINT('',#70742);
#13663=VERTEX_POINT('',#70746);
#13664=VERTEX_POINT('',#70747);
#13665=VERTEX_POINT('',#70750);
#13666=VERTEX_POINT('',#70754);
#13667=VERTEX_POINT('',#70758);
#13668=VERTEX_POINT('',#70761);
#13669=VERTEX_POINT('',#70764);
#13670=VERTEX_POINT('',#70768);
#13671=VERTEX_POINT('',#70771);
#13672=VERTEX_POINT('',#70775);
#13673=VERTEX_POINT('',#70778);
#13674=VERTEX_POINT('',#70782);
#13675=VERTEX_POINT('',#70785);
#13676=VERTEX_POINT('',#70789);
#13677=VERTEX_POINT('',#70792);
#13678=VERTEX_POINT('',#70797);
#13679=VERTEX_POINT('',#70799);
#13680=VERTEX_POINT('',#70801);
#13681=VERTEX_POINT('',#70803);
#13682=VERTEX_POINT('',#70806);
#13683=VERTEX_POINT('',#70810);
#13684=VERTEX_POINT('',#70814);
#13685=VERTEX_POINT('',#70818);
#13686=VERTEX_POINT('',#70822);
#13687=VERTEX_POINT('',#70827);
#13688=VERTEX_POINT('',#70831);
#13689=VERTEX_POINT('',#70837);
#13690=VERTEX_POINT('',#70843);
#13691=VERTEX_POINT('',#70853);
#13692=VERTEX_POINT('',#70855);
#13693=VERTEX_POINT('',#70859);
#13694=VERTEX_POINT('',#70860);
#13695=VERTEX_POINT('',#70862);
#13696=VERTEX_POINT('',#70864);
#13697=VERTEX_POINT('',#70867);
#13698=VERTEX_POINT('',#70869);
#13699=VERTEX_POINT('',#70871);
#13700=VERTEX_POINT('',#70873);
#13701=VERTEX_POINT('',#70875);
#13702=VERTEX_POINT('',#70877);
#13703=VERTEX_POINT('',#70879);
#13704=VERTEX_POINT('',#70881);
#13705=VERTEX_POINT('',#70883);
#13706=VERTEX_POINT('',#70885);
#13707=VERTEX_POINT('',#70888);
#13708=VERTEX_POINT('',#70892);
#13709=VERTEX_POINT('',#70896);
#13710=VERTEX_POINT('',#70900);
#13711=VERTEX_POINT('',#70904);
#13712=VERTEX_POINT('',#70908);
#13713=VERTEX_POINT('',#70912);
#13714=VERTEX_POINT('',#70916);
#13715=VERTEX_POINT('',#70920);
#13716=VERTEX_POINT('',#70924);
#13717=VERTEX_POINT('',#70928);
#13718=VERTEX_POINT('',#70932);
#13719=VERTEX_POINT('',#70936);
#13720=VERTEX_POINT('',#70940);
#13721=VERTEX_POINT('',#70942);
#13722=VERTEX_POINT('',#70946);
#13723=VERTEX_POINT('',#70947);
#13724=VERTEX_POINT('',#70949);
#13725=VERTEX_POINT('',#70951);
#13726=VERTEX_POINT('',#70954);
#13727=VERTEX_POINT('',#70956);
#13728=VERTEX_POINT('',#70958);
#13729=VERTEX_POINT('',#70960);
#13730=VERTEX_POINT('',#70962);
#13731=VERTEX_POINT('',#70964);
#13732=VERTEX_POINT('',#70966);
#13733=VERTEX_POINT('',#70968);
#13734=VERTEX_POINT('',#70970);
#13735=VERTEX_POINT('',#70972);
#13736=VERTEX_POINT('',#70975);
#13737=VERTEX_POINT('',#70979);
#13738=VERTEX_POINT('',#70983);
#13739=VERTEX_POINT('',#70987);
#13740=VERTEX_POINT('',#70991);
#13741=VERTEX_POINT('',#70995);
#13742=VERTEX_POINT('',#70999);
#13743=VERTEX_POINT('',#71003);
#13744=VERTEX_POINT('',#71007);
#13745=VERTEX_POINT('',#71011);
#13746=VERTEX_POINT('',#71013);
#13747=VERTEX_POINT('',#71017);
#13748=VERTEX_POINT('',#71018);
#13749=VERTEX_POINT('',#71023);
#13750=VERTEX_POINT('',#71024);
#13751=VERTEX_POINT('',#71029);
#13752=VERTEX_POINT('',#71034);
#13753=VERTEX_POINT('',#71038);
#13754=VERTEX_POINT('',#71039);
#13755=VERTEX_POINT('',#71044);
#13756=VERTEX_POINT('',#71045);
#13757=VERTEX_POINT('',#71053);
#13758=VERTEX_POINT('',#71057);
#13759=VERTEX_POINT('',#71063);
#13760=VERTEX_POINT('',#71064);
#13761=VERTEX_POINT('',#71066);
#13762=VERTEX_POINT('',#71068);
#13763=VERTEX_POINT('',#71070);
#13764=VERTEX_POINT('',#71072);
#13765=VERTEX_POINT('',#71074);
#13766=VERTEX_POINT('',#71076);
#13767=VERTEX_POINT('',#71080);
#13768=VERTEX_POINT('',#71084);
#13769=VERTEX_POINT('',#71088);
#13770=VERTEX_POINT('',#71092);
#13771=VERTEX_POINT('',#71096);
#13772=VERTEX_POINT('',#71100);
#13773=VERTEX_POINT('',#71104);
#13774=VERTEX_POINT('',#71108);
#13775=VERTEX_POINT('',#71112);
#13776=VERTEX_POINT('',#71116);
#13777=VERTEX_POINT('',#71120);
#13778=VERTEX_POINT('',#71124);
#13779=VERTEX_POINT('',#71128);
#13780=VERTEX_POINT('',#71132);
#13781=VERTEX_POINT('',#71136);
#13782=VERTEX_POINT('',#71140);
#13783=VERTEX_POINT('',#71144);
#13784=VERTEX_POINT('',#71148);
#13785=VERTEX_POINT('',#71152);
#13786=VERTEX_POINT('',#71156);
#13787=VERTEX_POINT('',#71157);
#13788=VERTEX_POINT('',#71159);
#13789=VERTEX_POINT('',#71161);
#13790=VERTEX_POINT('',#71164);
#13791=VERTEX_POINT('',#71166);
#13792=VERTEX_POINT('',#71168);
#13793=VERTEX_POINT('',#71170);
#13794=VERTEX_POINT('',#71172);
#13795=VERTEX_POINT('',#71174);
#13796=VERTEX_POINT('',#71176);
#13797=VERTEX_POINT('',#71178);
#13798=VERTEX_POINT('',#71180);
#13799=VERTEX_POINT('',#71182);
#13800=VERTEX_POINT('',#71193);
#13801=VERTEX_POINT('',#71197);
#13802=VERTEX_POINT('',#71201);
#13803=VERTEX_POINT('',#71205);
#13804=VERTEX_POINT('',#71206);
#13805=VERTEX_POINT('',#71208);
#13806=VERTEX_POINT('',#71210);
#13807=VERTEX_POINT('',#71213);
#13808=VERTEX_POINT('',#71215);
#13809=VERTEX_POINT('',#71217);
#13810=VERTEX_POINT('',#71219);
#13811=VERTEX_POINT('',#71221);
#13812=VERTEX_POINT('',#71223);
#13813=VERTEX_POINT('',#71225);
#13814=VERTEX_POINT('',#71227);
#13815=VERTEX_POINT('',#71229);
#13816=VERTEX_POINT('',#71231);
#13817=VERTEX_POINT('',#71245);
#13818=VERTEX_POINT('',#71249);
#13819=VERTEX_POINT('',#71258);
#13820=VERTEX_POINT('',#71262);
#13821=VERTEX_POINT('',#71268);
#13822=VERTEX_POINT('',#71272);
#13823=VERTEX_POINT('',#71302);
#13824=VERTEX_POINT('',#71303);
#13825=VERTEX_POINT('',#71306);
#13826=VERTEX_POINT('',#71310);
#13827=VERTEX_POINT('',#71312);
#13828=VERTEX_POINT('',#71316);
#13829=VERTEX_POINT('',#71321);
#13830=VERTEX_POINT('',#71325);
#13831=VERTEX_POINT('',#71329);
#13832=VERTEX_POINT('',#71333);
#13833=VERTEX_POINT('',#71341);
#13834=VERTEX_POINT('',#71342);
#13835=VERTEX_POINT('',#71344);
#13836=VERTEX_POINT('',#71346);
#13837=VERTEX_POINT('',#71348);
#13838=VERTEX_POINT('',#71350);
#13839=VERTEX_POINT('',#71352);
#13840=VERTEX_POINT('',#71354);
#13841=VERTEX_POINT('',#71358);
#13842=VERTEX_POINT('',#71363);
#13843=EDGE_CURVE('',#11278,#11279,#6302,.T.);
#13844=EDGE_CURVE('',#11279,#11280,#6303,.T.);
#13845=EDGE_CURVE('',#11280,#11281,#6304,.T.);
#13846=EDGE_CURVE('',#11281,#11282,#6305,.T.);
#13847=EDGE_CURVE('',#11282,#11278,#6306,.T.);
#13848=EDGE_CURVE('',#11280,#11283,#6307,.T.);
#13849=EDGE_CURVE('',#11284,#11283,#6308,.T.);
#13850=EDGE_CURVE('',#11285,#11284,#6309,.T.);
#13851=EDGE_CURVE('',#11285,#11286,#6310,.T.);
#13852=EDGE_CURVE('',#11281,#11286,#6311,.T.);
#13853=EDGE_CURVE('',#11287,#11279,#6312,.T.);
#13854=EDGE_CURVE('',#11283,#11287,#6313,.T.);
#13855=EDGE_CURVE('',#11278,#11288,#6314,.T.);
#13856=EDGE_CURVE('',#11288,#11287,#6315,.T.);
#13857=EDGE_CURVE('',#11288,#11289,#6316,.T.);
#13858=EDGE_CURVE('',#11289,#11284,#6317,.T.);
#13859=EDGE_CURVE('',#11289,#11290,#6318,.T.);
#13860=EDGE_CURVE('',#11291,#11290,#6319,.T.);
#13861=EDGE_CURVE('',#11292,#11291,#6320,.T.);
#13862=EDGE_CURVE('',#11292,#11285,#6321,.T.);
#13863=EDGE_CURVE('',#11293,#11288,#6322,.T.);
#13864=EDGE_CURVE('',#11294,#11293,#6323,.T.);
#13865=EDGE_CURVE('',#11295,#11294,#6324,.T.);
#13866=EDGE_CURVE('',#11296,#11295,#6325,.T.);
#13867=EDGE_CURVE('',#11297,#11296,#6326,.T.);
#13868=EDGE_CURVE('',#11290,#11297,#6327,.T.);
#13869=EDGE_CURVE('',#11298,#11299,#6328,.T.);
#13870=EDGE_CURVE('',#11299,#11300,#6329,.T.);
#13871=EDGE_CURVE('',#11300,#11301,#6330,.T.);
#13872=EDGE_CURVE('',#11301,#11302,#6331,.T.);
#13873=EDGE_CURVE('',#11302,#11298,#6332,.T.);
#13874=EDGE_CURVE('',#11303,#11302,#6333,.T.);
#13875=EDGE_CURVE('',#11304,#11303,#6334,.T.);
#13876=EDGE_CURVE('',#11298,#11304,#6335,.T.);
#13877=EDGE_CURVE('',#11305,#11301,#6336,.T.);
#13878=EDGE_CURVE('',#11305,#11292,#6337,.T.);
#13879=EDGE_CURVE('',#11303,#11291,#6338,.T.);
#13880=EDGE_CURVE('',#11286,#11305,#6339,.T.);
#13881=EDGE_CURVE('',#11300,#11282,#6340,.T.);
#13882=EDGE_CURVE('',#11304,#11297,#6341,.T.);
#13883=EDGE_CURVE('',#11297,#11299,#6342,.T.);
#13884=EDGE_CURVE('',#11306,#11296,#6343,.T.);
#13885=EDGE_CURVE('',#11306,#11299,#6344,.T.);
#13886=EDGE_CURVE('',#11307,#11307,#2045,.T.);
#13887=EDGE_CURVE('',#11307,#11308,#6345,.T.);
#13888=EDGE_CURVE('',#11308,#11308,#2046,.T.);
#13889=EDGE_CURVE('',#11309,#11310,#6346,.T.);
#13890=EDGE_CURVE('',#11311,#11309,#6347,.T.);
#13891=EDGE_CURVE('',#11312,#11311,#6348,.T.);
#13892=EDGE_CURVE('',#11310,#11312,#6349,.T.);
#13893=EDGE_CURVE('',#11313,#11313,#2047,.T.);
#13894=EDGE_CURVE('',#11314,#11314,#2048,.T.);
#13895=EDGE_CURVE('',#11315,#11315,#2049,.T.);
#13896=EDGE_CURVE('',#11308,#11316,#6350,.T.);
#13897=EDGE_CURVE('',#11316,#11316,#2050,.T.);
#13898=EDGE_CURVE('',#11313,#11317,#6351,.T.);
#13899=EDGE_CURVE('',#11317,#11317,#2051,.T.);
#13900=EDGE_CURVE('',#11317,#11318,#6352,.T.);
#13901=EDGE_CURVE('',#11318,#11318,#2052,.T.);
#13902=EDGE_CURVE('',#11315,#11319,#6353,.T.);
#13903=EDGE_CURVE('',#11319,#11319,#2053,.T.);
#13904=EDGE_CURVE('',#11319,#11320,#6354,.T.);
#13905=EDGE_CURVE('',#11320,#11320,#2054,.T.);
#13906=EDGE_CURVE('',#11314,#11321,#6355,.T.);
#13907=EDGE_CURVE('',#11321,#11321,#2055,.T.);
#13908=EDGE_CURVE('',#11321,#11322,#6356,.T.);
#13909=EDGE_CURVE('',#11322,#11322,#2056,.T.);
#13910=EDGE_CURVE('',#11323,#11323,#2057,.T.);
#13911=EDGE_CURVE('',#11323,#11322,#6357,.T.);
#13912=EDGE_CURVE('',#11324,#11325,#6358,.T.);
#13913=EDGE_CURVE('',#11326,#11324,#6359,.T.);
#13914=EDGE_CURVE('',#11327,#11326,#6360,.T.);
#13915=EDGE_CURVE('',#11325,#11327,#6361,.T.);
#13916=EDGE_CURVE('',#11328,#11328,#2058,.T.);
#13917=EDGE_CURVE('',#11329,#11329,#2059,.T.);
#13918=EDGE_CURVE('',#11330,#11330,#2060,.T.);
#13919=EDGE_CURVE('',#11328,#11320,#6362,.T.);
#13920=EDGE_CURVE('',#11330,#11318,#6363,.T.);
#13921=EDGE_CURVE('',#11329,#11316,#6364,.T.);
#13922=EDGE_CURVE('',#11331,#11331,#2061,.T.);
#13923=EDGE_CURVE('',#11331,#11332,#6365,.T.);
#13924=EDGE_CURVE('',#11332,#11332,#2062,.T.);
#13925=EDGE_CURVE('',#11333,#11334,#6366,.T.);
#13926=EDGE_CURVE('',#11335,#11333,#6367,.T.);
#13927=EDGE_CURVE('',#11336,#11335,#6368,.T.);
#13928=EDGE_CURVE('',#11334,#11336,#6369,.T.);
#13929=EDGE_CURVE('',#11337,#11337,#2063,.T.);
#13930=EDGE_CURVE('',#11338,#11338,#2064,.T.);
#13931=EDGE_CURVE('',#11339,#11339,#2065,.T.);
#13932=EDGE_CURVE('',#11340,#11340,#2066,.T.);
#13933=EDGE_CURVE('',#11340,#11332,#6370,.T.);
#13934=EDGE_CURVE('',#11337,#11341,#6371,.T.);
#13935=EDGE_CURVE('',#11341,#11341,#2067,.T.);
#13936=EDGE_CURVE('',#11342,#11342,#2068,.T.);
#13937=EDGE_CURVE('',#11342,#11341,#6372,.T.);
#13938=EDGE_CURVE('',#11339,#11343,#6373,.T.);
#13939=EDGE_CURVE('',#11343,#11343,#2069,.T.);
#13940=EDGE_CURVE('',#11344,#11344,#2070,.T.);
#13941=EDGE_CURVE('',#11344,#11343,#6374,.T.);
#13942=EDGE_CURVE('',#11338,#11345,#6375,.T.);
#13943=EDGE_CURVE('',#11345,#11345,#2071,.T.);
#13944=EDGE_CURVE('',#11346,#11346,#2072,.T.);
#13945=EDGE_CURVE('',#11346,#11345,#6376,.T.);
#13946=EDGE_CURVE('',#11347,#11348,#6377,.T.);
#13947=EDGE_CURVE('',#11348,#11349,#2073,.T.);
#13948=EDGE_CURVE('',#11349,#11350,#2074,.T.);
#13949=EDGE_CURVE('',#11350,#11351,#6378,.T.);
#13950=EDGE_CURVE('',#11351,#11347,#2075,.T.);
#13951=EDGE_CURVE('',#11352,#11353,#6379,.T.);
#13952=EDGE_CURVE('',#11353,#11354,#551,.T.);
#13953=EDGE_CURVE('',#11354,#11355,#6380,.T.);
#13954=EDGE_CURVE('',#11355,#11352,#552,.T.);
#13955=EDGE_CURVE('',#11354,#11351,#553,.T.);
#13956=EDGE_CURVE('',#11350,#11355,#554,.T.);
#13957=EDGE_CURVE('',#11347,#11353,#555,.T.);
#13958=EDGE_CURVE('',#11352,#11348,#556,.T.);
#13959=EDGE_CURVE('',#11347,#11356,#6381,.T.);
#13960=EDGE_CURVE('',#11357,#11356,#2076,.T.);
#13961=EDGE_CURVE('',#11357,#11358,#6382,.T.);
#13962=EDGE_CURVE('',#11359,#11358,#2077,.T.);
#13963=EDGE_CURVE('',#11359,#11360,#6383,.T.);
#13964=EDGE_CURVE('',#11361,#11360,#557,.T.);
#13965=EDGE_CURVE('',#11362,#11361,#558,.T.);
#13966=EDGE_CURVE('',#11363,#11362,#559,.T.);
#13967=EDGE_CURVE('',#11363,#11351,#6384,.T.);
#13968=EDGE_CURVE('',#11349,#11364,#6385,.T.);
#13969=EDGE_CURVE('',#11365,#11364,#2078,.T.);
#13970=EDGE_CURVE('',#11366,#11365,#560,.T.);
#13971=EDGE_CURVE('',#11367,#11366,#561,.T.);
#13972=EDGE_CURVE('',#11368,#11367,#562,.T.);
#13973=EDGE_CURVE('',#11364,#11368,#2079,.T.);
#13974=EDGE_CURVE('',#11369,#11369,#2080,.T.);
#13975=EDGE_CURVE('',#11369,#11346,#6386,.T.);
#13976=EDGE_CURVE('',#11370,#11371,#6387,.T.);
#13977=EDGE_CURVE('',#11372,#11370,#6388,.T.);
#13978=EDGE_CURVE('',#11373,#11372,#6389,.T.);
#13979=EDGE_CURVE('',#11371,#11373,#6390,.T.);
#13980=EDGE_CURVE('',#11374,#11374,#2081,.T.);
#13981=EDGE_CURVE('',#11375,#11375,#2082,.T.);
#13982=EDGE_CURVE('',#11376,#11376,#2083,.T.);
#13983=EDGE_CURVE('',#11374,#11344,#6391,.T.);
#13984=EDGE_CURVE('',#11376,#11342,#6392,.T.);
#13985=EDGE_CURVE('',#11375,#11340,#6393,.T.);
#13986=EDGE_CURVE('',#11377,#11378,#6394,.T.);
#13987=EDGE_CURVE('',#11378,#11379,#2084,.T.);
#13988=EDGE_CURVE('',#11379,#11380,#6395,.T.);
#13989=EDGE_CURVE('',#11380,#11377,#2085,.T.);
#13990=EDGE_CURVE('',#11377,#11381,#6396,.T.);
#13991=EDGE_CURVE('',#11381,#11356,#6397,.T.);
#13992=EDGE_CURVE('',#11356,#11378,#6398,.T.);
#13993=EDGE_CURVE('',#11382,#11357,#6399,.T.);
#13994=EDGE_CURVE('',#11381,#11382,#2086,.T.);
#13995=EDGE_CURVE('',#11382,#11383,#6400,.T.);
#13996=EDGE_CURVE('',#11383,#11384,#6401,.T.);
#13997=EDGE_CURVE('',#11384,#11357,#6402,.T.);
#13998=EDGE_CURVE('',#11385,#11325,#6403,.T.);
#13999=EDGE_CURVE('',#11325,#11384,#2087,.T.);
#14000=EDGE_CURVE('',#11383,#11385,#2088,.T.);
#14001=EDGE_CURVE('',#11385,#11386,#6404,.T.);
#14002=EDGE_CURVE('',#11386,#11324,#6405,.T.);
#14003=EDGE_CURVE('',#11387,#11388,#6406,.T.);
#14004=EDGE_CURVE('',#11388,#11324,#2089,.T.);
#14005=EDGE_CURVE('',#11386,#11387,#2090,.T.);
#14006=EDGE_CURVE('',#11387,#11380,#6407,.T.);
#14007=EDGE_CURVE('',#11379,#11388,#6408,.T.);
#14008=EDGE_CURVE('',#11388,#11295,#6409,.T.);
#14009=EDGE_CURVE('',#11295,#11389,#6410,.T.);
#14010=EDGE_CURVE('',#11389,#11390,#6411,.T.);
#14011=EDGE_CURVE('',#11326,#11390,#2091,.T.);
#14012=EDGE_CURVE('',#11296,#11379,#6412,.T.);
#14013=EDGE_CURVE('',#11378,#11391,#6413,.T.);
#14014=EDGE_CURVE('',#11392,#11391,#563,.T.);
#14015=EDGE_CURVE('',#11393,#11392,#564,.T.);
#14016=EDGE_CURVE('',#11394,#11393,#565,.T.);
#14017=EDGE_CURVE('',#11394,#11395,#6414,.T.);
#14018=EDGE_CURVE('',#11396,#11395,#566,.T.);
#14019=EDGE_CURVE('',#11397,#11396,#567,.T.);
#14020=EDGE_CURVE('',#11398,#11397,#568,.T.);
#14021=EDGE_CURVE('',#11398,#11399,#6415,.T.);
#14022=EDGE_CURVE('',#11400,#11399,#2092,.T.);
#14023=EDGE_CURVE('',#11400,#11306,#6416,.T.);
#14024=EDGE_CURVE('',#11401,#11402,#6417,.T.);
#14025=EDGE_CURVE('',#11403,#11401,#2093,.T.);
#14026=EDGE_CURVE('',#11404,#11403,#6418,.T.);
#14027=EDGE_CURVE('',#11405,#11404,#2094,.T.);
#14028=EDGE_CURVE('',#11406,#11405,#6419,.T.);
#14029=EDGE_CURVE('',#11407,#11406,#2095,.T.);
#14030=EDGE_CURVE('',#11408,#11407,#6420,.T.);
#14031=EDGE_CURVE('',#11402,#11408,#2096,.T.);
#14032=EDGE_CURVE('',#11409,#11400,#6421,.T.);
#14033=EDGE_CURVE('',#11399,#11410,#6422,.T.);
#14034=EDGE_CURVE('',#11410,#11409,#2097,.T.);
#14035=EDGE_CURVE('',#11409,#11411,#6423,.T.);
#14036=EDGE_CURVE('',#11411,#11390,#6424,.T.);
#14037=EDGE_CURVE('',#11390,#11400,#6425,.T.);
#14038=EDGE_CURVE('',#11412,#11326,#6426,.T.);
#14039=EDGE_CURVE('',#11411,#11412,#2098,.T.);
#14040=EDGE_CURVE('',#11412,#11413,#6427,.T.);
#14041=EDGE_CURVE('',#11413,#11327,#6428,.T.);
#14042=EDGE_CURVE('',#11414,#11415,#6429,.T.);
#14043=EDGE_CURVE('',#11415,#11327,#2099,.T.);
#14044=EDGE_CURVE('',#11413,#11414,#2100,.T.);
#14045=EDGE_CURVE('',#11414,#11416,#6430,.T.);
#14046=EDGE_CURVE('',#11416,#11358,#6431,.T.);
#14047=EDGE_CURVE('',#11358,#11415,#6432,.T.);
#14048=EDGE_CURVE('',#11417,#11359,#6433,.T.);
#14049=EDGE_CURVE('',#11416,#11417,#2101,.T.);
#14050=EDGE_CURVE('',#11417,#11410,#6434,.T.);
#14051=EDGE_CURVE('',#11399,#11359,#6435,.T.);
#14052=EDGE_CURVE('',#11415,#11384,#6436,.T.);
#14053=EDGE_CURVE('',#11360,#11363,#2102,.T.);
#14054=EDGE_CURVE('',#11395,#11398,#2103,.T.);
#14055=EDGE_CURVE('',#11391,#11394,#2104,.T.);
#14056=EDGE_CURVE('',#11418,#11419,#569,.T.);
#14057=EDGE_CURVE('',#11419,#11420,#570,.T.);
#14058=EDGE_CURVE('',#11420,#11421,#571,.T.);
#14059=EDGE_CURVE('',#11421,#11422,#572,.T.);
#14060=EDGE_CURVE('',#11422,#11423,#573,.T.);
#14061=EDGE_CURVE('',#11423,#11424,#574,.T.);
#14062=EDGE_CURVE('',#11424,#11425,#575,.T.);
#14063=EDGE_CURVE('',#11425,#11426,#576,.T.);
#14064=EDGE_CURVE('',#11426,#11427,#577,.T.);
#14065=EDGE_CURVE('',#11427,#11418,#578,.T.);
#14066=EDGE_CURVE('',#11428,#11429,#6437,.T.);
#14067=EDGE_CURVE('',#11429,#11430,#6438,.T.);
#14068=EDGE_CURVE('',#11430,#11431,#6439,.T.);
#14069=EDGE_CURVE('',#11431,#11432,#6440,.T.);
#14070=EDGE_CURVE('',#11432,#11433,#6441,.T.);
#14071=EDGE_CURVE('',#11433,#11434,#6442,.T.);
#14072=EDGE_CURVE('',#11434,#11435,#6443,.T.);
#14073=EDGE_CURVE('',#11435,#11428,#6444,.T.);
#14074=EDGE_CURVE('',#11436,#11437,#579,.T.);
#14075=EDGE_CURVE('',#11437,#11438,#580,.T.);
#14076=EDGE_CURVE('',#11438,#11439,#581,.T.);
#14077=EDGE_CURVE('',#11439,#11440,#582,.T.);
#14078=EDGE_CURVE('',#11440,#11441,#583,.T.);
#14079=EDGE_CURVE('',#11441,#11442,#584,.T.);
#14080=EDGE_CURVE('',#11442,#11443,#585,.T.);
#14081=EDGE_CURVE('',#11443,#11444,#586,.T.);
#14082=EDGE_CURVE('',#11444,#11445,#587,.T.);
#14083=EDGE_CURVE('',#11445,#11446,#588,.T.);
#14084=EDGE_CURVE('',#11446,#11447,#589,.T.);
#14085=EDGE_CURVE('',#11447,#11448,#590,.T.);
#14086=EDGE_CURVE('',#11448,#11436,#591,.T.);
#14087=EDGE_CURVE('',#11449,#11450,#6445,.T.);
#14088=EDGE_CURVE('',#11450,#11451,#6446,.T.);
#14089=EDGE_CURVE('',#11451,#11452,#6447,.T.);
#14090=EDGE_CURVE('',#11452,#11453,#592,.T.);
#14091=EDGE_CURVE('',#11453,#11454,#593,.T.);
#14092=EDGE_CURVE('',#11454,#11455,#594,.T.);
#14093=EDGE_CURVE('',#11455,#11456,#595,.T.);
#14094=EDGE_CURVE('',#11456,#11457,#596,.T.);
#14095=EDGE_CURVE('',#11457,#11458,#597,.T.);
#14096=EDGE_CURVE('',#11458,#11459,#598,.T.);
#14097=EDGE_CURVE('',#11459,#11460,#599,.T.);
#14098=EDGE_CURVE('',#11460,#11461,#6448,.T.);
#14099=EDGE_CURVE('',#11461,#11462,#600,.T.);
#14100=EDGE_CURVE('',#11462,#11463,#601,.T.);
#14101=EDGE_CURVE('',#11463,#11464,#602,.T.);
#14102=EDGE_CURVE('',#11464,#11465,#603,.T.);
#14103=EDGE_CURVE('',#11465,#11466,#604,.T.);
#14104=EDGE_CURVE('',#11466,#11467,#605,.T.);
#14105=EDGE_CURVE('',#11467,#11468,#606,.T.);
#14106=EDGE_CURVE('',#11468,#11469,#607,.T.);
#14107=EDGE_CURVE('',#11469,#11470,#608,.T.);
#14108=EDGE_CURVE('',#11470,#11449,#609,.T.);
#14109=EDGE_CURVE('',#11471,#11472,#6449,.T.);
#14110=EDGE_CURVE('',#11472,#11473,#6450,.T.);
#14111=EDGE_CURVE('',#11473,#11474,#6451,.T.);
#14112=EDGE_CURVE('',#11474,#11475,#6452,.T.);
#14113=EDGE_CURVE('',#11475,#11476,#6453,.T.);
#14114=EDGE_CURVE('',#11476,#11477,#6454,.T.);
#14115=EDGE_CURVE('',#11477,#11478,#6455,.T.);
#14116=EDGE_CURVE('',#11478,#11479,#6456,.T.);
#14117=EDGE_CURVE('',#11479,#11480,#6457,.T.);
#14118=EDGE_CURVE('',#11480,#11471,#6458,.T.);
#14119=EDGE_CURVE('',#11481,#11482,#6459,.T.);
#14120=EDGE_CURVE('',#11483,#11481,#2105,.T.);
#14121=EDGE_CURVE('',#11484,#11483,#6460,.T.);
#14122=EDGE_CURVE('',#11485,#11484,#2106,.T.);
#14123=EDGE_CURVE('',#11486,#11485,#6461,.T.);
#14124=EDGE_CURVE('',#11487,#11486,#2107,.T.);
#14125=EDGE_CURVE('',#11488,#11487,#6462,.T.);
#14126=EDGE_CURVE('',#11482,#11488,#2108,.T.);
#14127=EDGE_CURVE('',#11398,#11489,#6463,.T.);
#14128=EDGE_CURVE('',#11489,#11490,#2109,.T.);
#14129=EDGE_CURVE('',#11490,#11491,#2110,.T.);
#14130=EDGE_CURVE('',#11491,#11395,#6464,.T.);
#14131=EDGE_CURVE('',#11492,#11397,#6465,.T.);
#14132=EDGE_CURVE('',#11396,#11493,#6466,.T.);
#14133=EDGE_CURVE('',#11493,#11492,#610,.T.);
#14134=EDGE_CURVE('',#11491,#11493,#611,.T.);
#14135=EDGE_CURVE('',#11492,#11489,#612,.T.);
#14136=EDGE_CURVE('',#11490,#11494,#6467,.T.);
#14137=EDGE_CURVE('',#11495,#11494,#2111,.T.);
#14138=EDGE_CURVE('',#11496,#11495,#613,.T.);
#14139=EDGE_CURVE('',#11497,#11496,#614,.T.);
#14140=EDGE_CURVE('',#11498,#11497,#615,.T.);
#14141=EDGE_CURVE('',#11494,#11498,#2112,.T.);
#14142=EDGE_CURVE('',#11363,#11499,#6468,.T.);
#14143=EDGE_CURVE('',#11499,#11500,#2113,.T.);
#14144=EDGE_CURVE('',#11500,#11501,#2114,.T.);
#14145=EDGE_CURVE('',#11501,#11360,#6469,.T.);
#14146=EDGE_CURVE('',#11502,#11362,#6470,.T.);
#14147=EDGE_CURVE('',#11361,#11503,#6471,.T.);
#14148=EDGE_CURVE('',#11503,#11502,#616,.T.);
#14149=EDGE_CURVE('',#11501,#11503,#617,.T.);
#14150=EDGE_CURVE('',#11502,#11499,#618,.T.);
#14151=EDGE_CURVE('',#11500,#11504,#6472,.T.);
#14152=EDGE_CURVE('',#11505,#11504,#2115,.T.);
#14153=EDGE_CURVE('',#11506,#11505,#619,.T.);
#14154=EDGE_CURVE('',#11507,#11506,#620,.T.);
#14155=EDGE_CURVE('',#11508,#11507,#621,.T.);
#14156=EDGE_CURVE('',#11504,#11508,#2116,.T.);
#14157=EDGE_CURVE('',#11482,#11509,#6473,.T.);
#14158=EDGE_CURVE('',#11509,#11510,#6474,.T.);
#14159=EDGE_CURVE('',#11510,#11481,#6475,.T.);
#14160=EDGE_CURVE('',#11488,#11511,#6476,.T.);
#14161=EDGE_CURVE('',#11511,#11509,#2117,.T.);
#14162=EDGE_CURVE('',#11487,#11512,#6477,.T.);
#14163=EDGE_CURVE('',#11512,#11511,#6478,.T.);
#14164=EDGE_CURVE('',#11486,#11310,#6479,.T.);
#14165=EDGE_CURVE('',#11310,#11512,#2118,.T.);
#14166=EDGE_CURVE('',#11485,#11309,#6480,.T.);
#14167=EDGE_CURVE('',#11484,#11513,#6481,.T.);
#14168=EDGE_CURVE('',#11513,#11309,#2119,.T.);
#14169=EDGE_CURVE('',#11483,#11514,#6482,.T.);
#14170=EDGE_CURVE('',#11514,#11513,#6483,.T.);
#14171=EDGE_CURVE('',#11510,#11514,#2120,.T.);
#14172=EDGE_CURVE('',#11513,#11515,#6484,.T.);
#14173=EDGE_CURVE('',#11311,#11515,#2121,.T.);
#14174=EDGE_CURVE('',#11516,#11514,#6485,.T.);
#14175=EDGE_CURVE('',#11515,#11516,#6486,.T.);
#14176=EDGE_CURVE('',#11510,#11517,#6487,.T.);
#14177=EDGE_CURVE('',#11518,#11517,#622,.T.);
#14178=EDGE_CURVE('',#11519,#11518,#623,.T.);
#14179=EDGE_CURVE('',#11520,#11519,#624,.T.);
#14180=EDGE_CURVE('',#11521,#11520,#625,.T.);
#14181=EDGE_CURVE('',#11522,#11521,#626,.T.);
#14182=EDGE_CURVE('',#11523,#11522,#627,.T.);
#14183=EDGE_CURVE('',#11523,#11524,#6488,.T.);
#14184=EDGE_CURVE('',#11525,#11524,#628,.T.);
#14185=EDGE_CURVE('',#11526,#11525,#629,.T.);
#14186=EDGE_CURVE('',#11527,#11526,#630,.T.);
#14187=EDGE_CURVE('',#11528,#11527,#631,.T.);
#14188=EDGE_CURVE('',#11529,#11528,#632,.T.);
#14189=EDGE_CURVE('',#11530,#11529,#633,.T.);
#14190=EDGE_CURVE('',#11530,#11531,#6489,.T.);
#14191=EDGE_CURVE('',#11516,#11531,#2122,.T.);
#14192=EDGE_CURVE('',#11532,#11509,#6490,.T.);
#14193=EDGE_CURVE('',#11533,#11532,#2123,.T.);
#14194=EDGE_CURVE('',#11534,#11533,#6491,.T.);
#14195=EDGE_CURVE('',#11535,#11534,#2124,.T.);
#14196=EDGE_CURVE('',#11536,#11535,#6492,.T.);
#14197=EDGE_CURVE('',#11531,#11536,#6493,.T.);
#14198=EDGE_CURVE('',#11524,#11530,#2125,.T.);
#14199=EDGE_CURVE('',#11517,#11523,#2126,.T.);
#14200=EDGE_CURVE('',#11518,#11497,#6494,.T.);
#14201=EDGE_CURVE('',#11521,#11496,#6495,.T.);
#14202=EDGE_CURVE('',#11523,#11495,#6496,.T.);
#14203=EDGE_CURVE('',#11498,#11517,#6497,.T.);
#14204=EDGE_CURVE('',#11536,#11401,#6498,.T.);
#14205=EDGE_CURVE('',#11402,#11531,#6499,.T.);
#14206=EDGE_CURVE('',#11536,#11537,#2127,.T.);
#14207=EDGE_CURVE('',#11537,#11403,#6500,.T.);
#14208=EDGE_CURVE('',#11538,#11404,#6501,.T.);
#14209=EDGE_CURVE('',#11537,#11538,#6502,.T.);
#14210=EDGE_CURVE('',#11538,#11312,#2128,.T.);
#14211=EDGE_CURVE('',#11312,#11405,#6503,.T.);
#14212=EDGE_CURVE('',#11311,#11406,#6504,.T.);
#14213=EDGE_CURVE('',#11515,#11407,#6505,.T.);
#14214=EDGE_CURVE('',#11516,#11408,#6506,.T.);
#14215=EDGE_CURVE('',#11538,#11512,#6507,.T.);
#14216=EDGE_CURVE('',#11511,#11537,#6508,.T.);
#14217=EDGE_CURVE('',#11539,#11535,#634,.T.);
#14218=EDGE_CURVE('',#11540,#11539,#635,.T.);
#14219=EDGE_CURVE('',#11541,#11540,#636,.T.);
#14220=EDGE_CURVE('',#11542,#11541,#637,.T.);
#14221=EDGE_CURVE('',#11543,#11542,#638,.T.);
#14222=EDGE_CURVE('',#11534,#11543,#639,.T.);
#14223=EDGE_CURVE('',#11544,#11533,#640,.T.);
#14224=EDGE_CURVE('',#11545,#11544,#641,.T.);
#14225=EDGE_CURVE('',#11546,#11545,#642,.T.);
#14226=EDGE_CURVE('',#11547,#11546,#643,.T.);
#14227=EDGE_CURVE('',#11548,#11547,#644,.T.);
#14228=EDGE_CURVE('',#11532,#11548,#645,.T.);
#14229=EDGE_CURVE('',#11539,#11367,#6509,.T.);
#14230=EDGE_CURVE('',#11542,#11366,#6510,.T.);
#14231=EDGE_CURVE('',#11534,#11365,#6511,.T.);
#14232=EDGE_CURVE('',#11368,#11535,#6512,.T.);
#14233=EDGE_CURVE('',#11544,#11507,#6513,.T.);
#14234=EDGE_CURVE('',#11547,#11506,#6514,.T.);
#14235=EDGE_CURVE('',#11532,#11505,#6515,.T.);
#14236=EDGE_CURVE('',#11508,#11533,#6516,.T.);
#14237=EDGE_CURVE('',#11394,#11549,#6517,.T.);
#14238=EDGE_CURVE('',#11549,#11550,#2129,.T.);
#14239=EDGE_CURVE('',#11550,#11551,#2130,.T.);
#14240=EDGE_CURVE('',#11551,#11391,#6518,.T.);
#14241=EDGE_CURVE('',#11552,#11393,#6519,.T.);
#14242=EDGE_CURVE('',#11392,#11553,#6520,.T.);
#14243=EDGE_CURVE('',#11553,#11552,#646,.T.);
#14244=EDGE_CURVE('',#11551,#11553,#647,.T.);
#14245=EDGE_CURVE('',#11552,#11549,#648,.T.);
#14246=EDGE_CURVE('',#11550,#11554,#6521,.T.);
#14247=EDGE_CURVE('',#11555,#11554,#2131,.T.);
#14248=EDGE_CURVE('',#11556,#11555,#649,.T.);
#14249=EDGE_CURVE('',#11557,#11556,#650,.T.);
#14250=EDGE_CURVE('',#11558,#11557,#651,.T.);
#14251=EDGE_CURVE('',#11554,#11558,#2132,.T.);
#14252=EDGE_CURVE('',#11525,#11557,#6522,.T.);
#14253=EDGE_CURVE('',#11528,#11556,#6523,.T.);
#14254=EDGE_CURVE('',#11530,#11555,#6524,.T.);
#14255=EDGE_CURVE('',#11558,#11524,#6525,.T.);
#14256=EDGE_CURVE('',#11559,#11560,#6526,.T.);
#14257=EDGE_CURVE('',#11560,#11561,#2133,.T.);
#14258=EDGE_CURVE('',#11561,#11562,#6527,.T.);
#14259=EDGE_CURVE('',#11562,#11559,#2134,.T.);
#14260=EDGE_CURVE('',#11563,#11564,#6528,.T.);
#14261=EDGE_CURVE('',#11564,#11560,#6529,.T.);
#14262=EDGE_CURVE('',#11559,#11563,#6530,.T.);
#14263=EDGE_CURVE('',#11565,#11566,#6531,.T.);
#14264=EDGE_CURVE('',#11566,#11564,#2135,.T.);
#14265=EDGE_CURVE('',#11563,#11565,#2136,.T.);
#14266=EDGE_CURVE('',#11567,#11568,#6532,.T.);
#14267=EDGE_CURVE('',#11568,#11566,#6533,.T.);
#14268=EDGE_CURVE('',#11565,#11567,#6534,.T.);
#14269=EDGE_CURVE('',#11569,#11371,#6535,.T.);
#14270=EDGE_CURVE('',#11371,#11568,#2137,.T.);
#14271=EDGE_CURVE('',#11567,#11569,#2138,.T.);
#14272=EDGE_CURVE('',#11570,#11370,#6536,.T.);
#14273=EDGE_CURVE('',#11569,#11570,#6537,.T.);
#14274=EDGE_CURVE('',#11571,#11572,#6538,.T.);
#14275=EDGE_CURVE('',#11572,#11370,#2139,.T.);
#14276=EDGE_CURVE('',#11570,#11571,#2140,.T.);
#14277=EDGE_CURVE('',#11561,#11572,#6539,.T.);
#14278=EDGE_CURVE('',#11571,#11562,#6540,.T.);
#14279=EDGE_CURVE('',#11572,#11573,#6541,.T.);
#14280=EDGE_CURVE('',#11573,#11294,#6542,.T.);
#14281=EDGE_CURVE('',#11294,#11574,#6543,.T.);
#14282=EDGE_CURVE('',#11372,#11574,#2141,.T.);
#14283=EDGE_CURVE('',#11575,#11561,#6544,.T.);
#14284=EDGE_CURVE('',#11575,#11573,#6545,.T.);
#14285=EDGE_CURVE('',#11560,#11576,#6546,.T.);
#14286=EDGE_CURVE('',#11577,#11576,#652,.T.);
#14287=EDGE_CURVE('',#11578,#11577,#653,.T.);
#14288=EDGE_CURVE('',#11579,#11578,#654,.T.);
#14289=EDGE_CURVE('',#11579,#11580,#6547,.T.);
#14290=EDGE_CURVE('',#11581,#11580,#655,.T.);
#14291=EDGE_CURVE('',#11582,#11581,#656,.T.);
#14292=EDGE_CURVE('',#11583,#11582,#657,.T.);
#14293=EDGE_CURVE('',#11583,#11584,#6548,.T.);
#14294=EDGE_CURVE('',#11585,#11584,#2142,.T.);
#14295=EDGE_CURVE('',#11585,#11293,#6549,.T.);
#14296=EDGE_CURVE('',#11293,#11575,#6550,.T.);
#14297=EDGE_CURVE('',#11586,#11587,#6551,.T.);
#14298=EDGE_CURVE('',#11588,#11586,#2143,.T.);
#14299=EDGE_CURVE('',#11589,#11588,#6552,.T.);
#14300=EDGE_CURVE('',#11590,#11589,#2144,.T.);
#14301=EDGE_CURVE('',#11591,#11590,#6553,.T.);
#14302=EDGE_CURVE('',#11592,#11591,#2145,.T.);
#14303=EDGE_CURVE('',#11593,#11592,#6554,.T.);
#14304=EDGE_CURVE('',#11587,#11593,#2146,.T.);
#14305=EDGE_CURVE('',#11594,#11585,#6555,.T.);
#14306=EDGE_CURVE('',#11584,#11595,#6556,.T.);
#14307=EDGE_CURVE('',#11595,#11594,#2147,.T.);
#14308=EDGE_CURVE('',#11594,#11596,#6557,.T.);
#14309=EDGE_CURVE('',#11596,#11574,#6558,.T.);
#14310=EDGE_CURVE('',#11574,#11585,#6559,.T.);
#14311=EDGE_CURVE('',#11597,#11372,#6560,.T.);
#14312=EDGE_CURVE('',#11596,#11597,#2148,.T.);
#14313=EDGE_CURVE('',#11597,#11598,#6561,.T.);
#14314=EDGE_CURVE('',#11598,#11373,#6562,.T.);
#14315=EDGE_CURVE('',#11599,#11600,#6563,.T.);
#14316=EDGE_CURVE('',#11600,#11373,#2149,.T.);
#14317=EDGE_CURVE('',#11598,#11599,#2150,.T.);
#14318=EDGE_CURVE('',#11599,#11601,#6564,.T.);
#14319=EDGE_CURVE('',#11601,#11602,#6565,.T.);
#14320=EDGE_CURVE('',#11602,#11600,#6566,.T.);
#14321=EDGE_CURVE('',#11603,#11604,#6567,.T.);
#14322=EDGE_CURVE('',#11604,#11602,#2151,.T.);
#14323=EDGE_CURVE('',#11601,#11603,#2152,.T.);
#14324=EDGE_CURVE('',#11603,#11595,#6568,.T.);
#14325=EDGE_CURVE('',#11584,#11604,#6569,.T.);
#14326=EDGE_CURVE('',#11600,#11568,#6570,.T.);
#14327=EDGE_CURVE('',#11566,#11602,#6571,.T.);
#14328=EDGE_CURVE('',#11604,#11605,#6572,.T.);
#14329=EDGE_CURVE('',#11606,#11605,#658,.T.);
#14330=EDGE_CURVE('',#11607,#11606,#659,.T.);
#14331=EDGE_CURVE('',#11608,#11607,#660,.T.);
#14332=EDGE_CURVE('',#11608,#11609,#6573,.T.);
#14333=EDGE_CURVE('',#11610,#11609,#661,.T.);
#14334=EDGE_CURVE('',#11611,#11610,#662,.T.);
#14335=EDGE_CURVE('',#11612,#11611,#663,.T.);
#14336=EDGE_CURVE('',#11612,#11564,#6574,.T.);
#14337=EDGE_CURVE('',#11609,#11612,#2153,.T.);
#14338=EDGE_CURVE('',#11605,#11608,#2154,.T.);
#14339=EDGE_CURVE('',#11580,#11583,#2155,.T.);
#14340=EDGE_CURVE('',#11576,#11579,#2156,.T.);
#14341=EDGE_CURVE('',#11613,#11614,#6575,.T.);
#14342=EDGE_CURVE('',#11615,#11613,#2157,.T.);
#14343=EDGE_CURVE('',#11616,#11615,#6576,.T.);
#14344=EDGE_CURVE('',#11617,#11616,#2158,.T.);
#14345=EDGE_CURVE('',#11618,#11617,#6577,.T.);
#14346=EDGE_CURVE('',#11619,#11618,#2159,.T.);
#14347=EDGE_CURVE('',#11620,#11619,#6578,.T.);
#14348=EDGE_CURVE('',#11614,#11620,#2160,.T.);
#14349=EDGE_CURVE('',#11621,#11607,#6579,.T.);
#14350=EDGE_CURVE('',#11606,#11622,#6580,.T.);
#14351=EDGE_CURVE('',#11622,#11621,#664,.T.);
#14352=EDGE_CURVE('',#11608,#11623,#6581,.T.);
#14353=EDGE_CURVE('',#11623,#11624,#2161,.T.);
#14354=EDGE_CURVE('',#11624,#11625,#2162,.T.);
#14355=EDGE_CURVE('',#11625,#11605,#6582,.T.);
#14356=EDGE_CURVE('',#11621,#11623,#665,.T.);
#14357=EDGE_CURVE('',#11625,#11622,#666,.T.);
#14358=EDGE_CURVE('',#11624,#11626,#6583,.T.);
#14359=EDGE_CURVE('',#11627,#11626,#2163,.T.);
#14360=EDGE_CURVE('',#11628,#11627,#667,.T.);
#14361=EDGE_CURVE('',#11629,#11628,#668,.T.);
#14362=EDGE_CURVE('',#11630,#11629,#669,.T.);
#14363=EDGE_CURVE('',#11626,#11630,#2164,.T.);
#14364=EDGE_CURVE('',#11631,#11613,#6584,.T.);
#14365=EDGE_CURVE('',#11614,#11632,#6585,.T.);
#14366=EDGE_CURVE('',#11632,#11631,#6586,.T.);
#14367=EDGE_CURVE('',#11631,#11633,#2165,.T.);
#14368=EDGE_CURVE('',#11633,#11615,#6587,.T.);
#14369=EDGE_CURVE('',#11634,#11616,#6588,.T.);
#14370=EDGE_CURVE('',#11633,#11634,#6589,.T.);
#14371=EDGE_CURVE('',#11634,#11333,#2166,.T.);
#14372=EDGE_CURVE('',#11333,#11617,#6590,.T.);
#14373=EDGE_CURVE('',#11334,#11618,#6591,.T.);
#14374=EDGE_CURVE('',#11334,#11635,#2167,.T.);
#14375=EDGE_CURVE('',#11635,#11619,#6592,.T.);
#14376=EDGE_CURVE('',#11636,#11620,#6593,.T.);
#14377=EDGE_CURVE('',#11635,#11636,#6594,.T.);
#14378=EDGE_CURVE('',#11636,#11632,#2168,.T.);
#14379=EDGE_CURVE('',#11634,#11637,#6595,.T.);
#14380=EDGE_CURVE('',#11335,#11637,#2169,.T.);
#14381=EDGE_CURVE('',#11638,#11633,#6596,.T.);
#14382=EDGE_CURVE('',#11637,#11638,#6597,.T.);
#14383=EDGE_CURVE('',#11631,#11639,#6598,.T.);
#14384=EDGE_CURVE('',#11640,#11639,#670,.T.);
#14385=EDGE_CURVE('',#11641,#11640,#671,.T.);
#14386=EDGE_CURVE('',#11642,#11641,#672,.T.);
#14387=EDGE_CURVE('',#11643,#11642,#673,.T.);
#14388=EDGE_CURVE('',#11644,#11643,#674,.T.);
#14389=EDGE_CURVE('',#11644,#11645,#6599,.T.);
#14390=EDGE_CURVE('',#11646,#11645,#675,.T.);
#14391=EDGE_CURVE('',#11647,#11646,#676,.T.);
#14392=EDGE_CURVE('',#11648,#11647,#677,.T.);
#14393=EDGE_CURVE('',#11649,#11648,#678,.T.);
#14394=EDGE_CURVE('',#11650,#11649,#679,.T.);
#14395=EDGE_CURVE('',#11651,#11650,#680,.T.);
#14396=EDGE_CURVE('',#11651,#11652,#6600,.T.);
#14397=EDGE_CURVE('',#11638,#11652,#2170,.T.);
#14398=EDGE_CURVE('',#11653,#11632,#6601,.T.);
#14399=EDGE_CURVE('',#11654,#11653,#2171,.T.);
#14400=EDGE_CURVE('',#11655,#11654,#6602,.T.);
#14401=EDGE_CURVE('',#11656,#11655,#2172,.T.);
#14402=EDGE_CURVE('',#11657,#11656,#6603,.T.);
#14403=EDGE_CURVE('',#11652,#11657,#6604,.T.);
#14404=EDGE_CURVE('',#11645,#11651,#2173,.T.);
#14405=EDGE_CURVE('',#11639,#11644,#2174,.T.);
#14406=EDGE_CURVE('',#11587,#11652,#6605,.T.);
#14407=EDGE_CURVE('',#11657,#11586,#6606,.T.);
#14408=EDGE_CURVE('',#11593,#11638,#6607,.T.);
#14409=EDGE_CURVE('',#11592,#11637,#6608,.T.);
#14410=EDGE_CURVE('',#11591,#11335,#6609,.T.);
#14411=EDGE_CURVE('',#11590,#11336,#6610,.T.);
#14412=EDGE_CURVE('',#11589,#11658,#6611,.T.);
#14413=EDGE_CURVE('',#11658,#11336,#2175,.T.);
#14414=EDGE_CURVE('',#11588,#11659,#6612,.T.);
#14415=EDGE_CURVE('',#11659,#11658,#6613,.T.);
#14416=EDGE_CURVE('',#11657,#11659,#2176,.T.);
#14417=EDGE_CURVE('',#11658,#11635,#6614,.T.);
#14418=EDGE_CURVE('',#11636,#11659,#6615,.T.);
#14419=EDGE_CURVE('',#11660,#11656,#681,.T.);
#14420=EDGE_CURVE('',#11661,#11660,#682,.T.);
#14421=EDGE_CURVE('',#11662,#11661,#683,.T.);
#14422=EDGE_CURVE('',#11663,#11662,#684,.T.);
#14423=EDGE_CURVE('',#11655,#11663,#685,.T.);
#14424=EDGE_CURVE('',#11664,#11654,#686,.T.);
#14425=EDGE_CURVE('',#11665,#11664,#687,.T.);
#14426=EDGE_CURVE('',#11666,#11665,#688,.T.);
#14427=EDGE_CURVE('',#11667,#11666,#689,.T.);
#14428=EDGE_CURVE('',#11668,#11667,#690,.T.);
#14429=EDGE_CURVE('',#11653,#11668,#691,.T.);
#14430=EDGE_CURVE('',#11664,#11629,#6616,.T.);
#14431=EDGE_CURVE('',#11667,#11628,#6617,.T.);
#14432=EDGE_CURVE('',#11653,#11627,#6618,.T.);
#14433=EDGE_CURVE('',#11630,#11654,#6619,.T.);
#14434=EDGE_CURVE('',#11579,#11669,#6620,.T.);
#14435=EDGE_CURVE('',#11669,#11670,#2177,.T.);
#14436=EDGE_CURVE('',#11670,#11671,#2178,.T.);
#14437=EDGE_CURVE('',#11671,#11576,#6621,.T.);
#14438=EDGE_CURVE('',#11672,#11578,#6622,.T.);
#14439=EDGE_CURVE('',#11577,#11673,#6623,.T.);
#14440=EDGE_CURVE('',#11673,#11672,#692,.T.);
#14441=EDGE_CURVE('',#11671,#11673,#693,.T.);
#14442=EDGE_CURVE('',#11672,#11669,#694,.T.);
#14443=EDGE_CURVE('',#11670,#11674,#6624,.T.);
#14444=EDGE_CURVE('',#11675,#11674,#2179,.T.);
#14445=EDGE_CURVE('',#11676,#11675,#695,.T.);
#14446=EDGE_CURVE('',#11677,#11676,#696,.T.);
#14447=EDGE_CURVE('',#11678,#11677,#697,.T.);
#14448=EDGE_CURVE('',#11674,#11678,#2180,.T.);
#14449=EDGE_CURVE('',#11646,#11677,#6625,.T.);
#14450=EDGE_CURVE('',#11649,#11676,#6626,.T.);
#14451=EDGE_CURVE('',#11651,#11675,#6627,.T.);
#14452=EDGE_CURVE('',#11678,#11645,#6628,.T.);
#14453=EDGE_CURVE('',#11679,#11611,#6629,.T.);
#14454=EDGE_CURVE('',#11610,#11680,#6630,.T.);
#14455=EDGE_CURVE('',#11680,#11679,#698,.T.);
#14456=EDGE_CURVE('',#11612,#11681,#6631,.T.);
#14457=EDGE_CURVE('',#11681,#11682,#2181,.T.);
#14458=EDGE_CURVE('',#11682,#11683,#2182,.T.);
#14459=EDGE_CURVE('',#11683,#11609,#6632,.T.);
#14460=EDGE_CURVE('',#11679,#11681,#699,.T.);
#14461=EDGE_CURVE('',#11683,#11680,#700,.T.);
#14462=EDGE_CURVE('',#11682,#11684,#6633,.T.);
#14463=EDGE_CURVE('',#11685,#11684,#2183,.T.);
#14464=EDGE_CURVE('',#11686,#11685,#701,.T.);
#14465=EDGE_CURVE('',#11687,#11686,#702,.T.);
#14466=EDGE_CURVE('',#11688,#11687,#703,.T.);
#14467=EDGE_CURVE('',#11684,#11688,#2184,.T.);
#14468=EDGE_CURVE('',#11660,#11687,#6634,.T.);
#14469=EDGE_CURVE('',#11663,#11686,#6635,.T.);
#14470=EDGE_CURVE('',#11655,#11685,#6636,.T.);
#14471=EDGE_CURVE('',#11688,#11656,#6637,.T.);
#14472=EDGE_CURVE('',#11583,#11689,#6638,.T.);
#14473=EDGE_CURVE('',#11689,#11690,#2185,.T.);
#14474=EDGE_CURVE('',#11690,#11691,#2186,.T.);
#14475=EDGE_CURVE('',#11691,#11580,#6639,.T.);
#14476=EDGE_CURVE('',#11692,#11582,#6640,.T.);
#14477=EDGE_CURVE('',#11581,#11693,#6641,.T.);
#14478=EDGE_CURVE('',#11693,#11692,#704,.T.);
#14479=EDGE_CURVE('',#11691,#11693,#705,.T.);
#14480=EDGE_CURVE('',#11692,#11689,#706,.T.);
#14481=EDGE_CURVE('',#11690,#11694,#6642,.T.);
#14482=EDGE_CURVE('',#11695,#11694,#2187,.T.);
#14483=EDGE_CURVE('',#11696,#11695,#707,.T.);
#14484=EDGE_CURVE('',#11697,#11696,#708,.T.);
#14485=EDGE_CURVE('',#11698,#11697,#709,.T.);
#14486=EDGE_CURVE('',#11694,#11698,#2188,.T.);
#14487=EDGE_CURVE('',#11640,#11697,#6643,.T.);
#14488=EDGE_CURVE('',#11643,#11696,#6644,.T.);
#14489=EDGE_CURVE('',#11644,#11695,#6645,.T.);
#14490=EDGE_CURVE('',#11698,#11639,#6646,.T.);
#14491=EDGE_CURVE('',#11699,#11699,#2189,.T.);
#14492=EDGE_CURVE('',#11699,#11700,#6647,.T.);
#14493=EDGE_CURVE('',#11700,#11700,#2190,.T.);
#14494=EDGE_CURVE('',#11700,#11701,#6648,.T.);
#14495=EDGE_CURVE('',#11701,#11701,#2191,.T.);
#14496=EDGE_CURVE('',#11702,#11702,#2192,.T.);
#14497=EDGE_CURVE('',#11703,#11703,#2193,.T.);
#14498=EDGE_CURVE('',#11703,#11701,#6649,.T.);
#14499=EDGE_CURVE('',#11573,#11389,#6650,.T.);
#14500=EDGE_CURVE('',#11704,#11704,#2194,.T.);
#14501=EDGE_CURVE('',#11702,#11705,#6651,.T.);
#14502=EDGE_CURVE('',#11705,#11705,#2195,.T.);
#14503=EDGE_CURVE('',#11705,#11706,#6652,.T.);
#14504=EDGE_CURVE('',#11706,#11706,#2196,.T.);
#14505=EDGE_CURVE('',#11704,#11706,#6653,.T.);
#14506=EDGE_CURVE('',#11707,#11708,#710,.T.);
#14507=EDGE_CURVE('',#11707,#11709,#6654,.T.);
#14508=EDGE_CURVE('',#11709,#11710,#711,.T.);
#14509=EDGE_CURVE('',#11708,#11710,#6655,.T.);
#14510=EDGE_CURVE('',#11711,#11707,#712,.T.);
#14511=EDGE_CURVE('',#11711,#11712,#6656,.T.);
#14512=EDGE_CURVE('',#11712,#11709,#713,.T.);
#14513=EDGE_CURVE('',#11713,#11711,#714,.T.);
#14514=EDGE_CURVE('',#11713,#11714,#6657,.T.);
#14515=EDGE_CURVE('',#11714,#11712,#715,.T.);
#14516=EDGE_CURVE('',#11715,#11713,#716,.T.);
#14517=EDGE_CURVE('',#11715,#11716,#6658,.T.);
#14518=EDGE_CURVE('',#11716,#11714,#717,.T.);
#14519=EDGE_CURVE('',#11717,#11715,#718,.T.);
#14520=EDGE_CURVE('',#11717,#11718,#6659,.T.);
#14521=EDGE_CURVE('',#11718,#11716,#719,.T.);
#14522=EDGE_CURVE('',#11719,#11717,#720,.T.);
#14523=EDGE_CURVE('',#11719,#11720,#6660,.T.);
#14524=EDGE_CURVE('',#11720,#11718,#721,.T.);
#14525=EDGE_CURVE('',#11721,#11719,#722,.T.);
#14526=EDGE_CURVE('',#11721,#11722,#6661,.T.);
#14527=EDGE_CURVE('',#11722,#11720,#723,.T.);
#14528=EDGE_CURVE('',#11708,#11721,#724,.T.);
#14529=EDGE_CURVE('',#11710,#11722,#725,.T.);
#14530=EDGE_CURVE('',#11418,#11723,#6662,.T.);
#14531=EDGE_CURVE('',#11723,#11724,#726,.T.);
#14532=EDGE_CURVE('',#11419,#11724,#6663,.T.);
#14533=EDGE_CURVE('',#11427,#11725,#6664,.T.);
#14534=EDGE_CURVE('',#11725,#11723,#727,.T.);
#14535=EDGE_CURVE('',#11426,#11726,#6665,.T.);
#14536=EDGE_CURVE('',#11726,#11725,#728,.T.);
#14537=EDGE_CURVE('',#11425,#11727,#6666,.T.);
#14538=EDGE_CURVE('',#11727,#11726,#729,.T.);
#14539=EDGE_CURVE('',#11424,#11728,#6667,.T.);
#14540=EDGE_CURVE('',#11728,#11727,#730,.T.);
#14541=EDGE_CURVE('',#11423,#11729,#6668,.T.);
#14542=EDGE_CURVE('',#11729,#11728,#731,.T.);
#14543=EDGE_CURVE('',#11422,#11730,#6669,.T.);
#14544=EDGE_CURVE('',#11730,#11729,#732,.T.);
#14545=EDGE_CURVE('',#11421,#11731,#6670,.T.);
#14546=EDGE_CURVE('',#11731,#11730,#733,.T.);
#14547=EDGE_CURVE('',#11420,#11732,#6671,.T.);
#14548=EDGE_CURVE('',#11732,#11731,#734,.T.);
#14549=EDGE_CURVE('',#11724,#11732,#735,.T.);
#14550=EDGE_CURVE('',#11428,#11733,#6672,.T.);
#14551=EDGE_CURVE('',#11733,#11734,#6673,.T.);
#14552=EDGE_CURVE('',#11429,#11734,#6674,.T.);
#14553=EDGE_CURVE('',#11435,#11735,#6675,.T.);
#14554=EDGE_CURVE('',#11735,#11733,#6676,.T.);
#14555=EDGE_CURVE('',#11434,#11736,#6677,.T.);
#14556=EDGE_CURVE('',#11736,#11735,#6678,.T.);
#14557=EDGE_CURVE('',#11433,#11737,#6679,.T.);
#14558=EDGE_CURVE('',#11737,#11736,#6680,.T.);
#14559=EDGE_CURVE('',#11432,#11738,#6681,.T.);
#14560=EDGE_CURVE('',#11738,#11737,#6682,.T.);
#14561=EDGE_CURVE('',#11431,#11739,#6683,.T.);
#14562=EDGE_CURVE('',#11739,#11738,#6684,.T.);
#14563=EDGE_CURVE('',#11430,#11740,#6685,.T.);
#14564=EDGE_CURVE('',#11740,#11739,#6686,.T.);
#14565=EDGE_CURVE('',#11734,#11740,#6687,.T.);
#14566=EDGE_CURVE('',#11741,#11742,#736,.T.);
#14567=EDGE_CURVE('',#11741,#11743,#6688,.T.);
#14568=EDGE_CURVE('',#11743,#11744,#737,.T.);
#14569=EDGE_CURVE('',#11742,#11744,#6689,.T.);
#14570=EDGE_CURVE('',#11745,#11741,#738,.T.);
#14571=EDGE_CURVE('',#11745,#11746,#6690,.T.);
#14572=EDGE_CURVE('',#11746,#11743,#739,.T.);
#14573=EDGE_CURVE('',#11747,#11745,#740,.T.);
#14574=EDGE_CURVE('',#11747,#11748,#6691,.T.);
#14575=EDGE_CURVE('',#11748,#11746,#741,.T.);
#14576=EDGE_CURVE('',#11749,#11747,#742,.T.);
#14577=EDGE_CURVE('',#11749,#11750,#6692,.T.);
#14578=EDGE_CURVE('',#11750,#11748,#743,.T.);
#14579=EDGE_CURVE('',#11751,#11749,#744,.T.);
#14580=EDGE_CURVE('',#11751,#11752,#6693,.T.);
#14581=EDGE_CURVE('',#11752,#11750,#745,.T.);
#14582=EDGE_CURVE('',#11753,#11751,#746,.T.);
#14583=EDGE_CURVE('',#11753,#11754,#6694,.T.);
#14584=EDGE_CURVE('',#11754,#11752,#747,.T.);
#14585=EDGE_CURVE('',#11755,#11753,#748,.T.);
#14586=EDGE_CURVE('',#11755,#11756,#6695,.T.);
#14587=EDGE_CURVE('',#11756,#11754,#749,.T.);
#14588=EDGE_CURVE('',#11757,#11755,#750,.T.);
#14589=EDGE_CURVE('',#11757,#11758,#6696,.T.);
#14590=EDGE_CURVE('',#11758,#11756,#751,.T.);
#14591=EDGE_CURVE('',#11742,#11757,#752,.T.);
#14592=EDGE_CURVE('',#11744,#11758,#753,.T.);
#14593=EDGE_CURVE('',#11436,#11759,#6697,.T.);
#14594=EDGE_CURVE('',#11759,#11760,#754,.T.);
#14595=EDGE_CURVE('',#11437,#11760,#6698,.T.);
#14596=EDGE_CURVE('',#11448,#11761,#6699,.T.);
#14597=EDGE_CURVE('',#11761,#11759,#755,.T.);
#14598=EDGE_CURVE('',#11447,#11762,#6700,.T.);
#14599=EDGE_CURVE('',#11762,#11761,#756,.T.);
#14600=EDGE_CURVE('',#11446,#11763,#6701,.T.);
#14601=EDGE_CURVE('',#11763,#11762,#757,.T.);
#14602=EDGE_CURVE('',#11445,#11764,#6702,.T.);
#14603=EDGE_CURVE('',#11764,#11763,#758,.T.);
#14604=EDGE_CURVE('',#11444,#11765,#6703,.T.);
#14605=EDGE_CURVE('',#11765,#11764,#759,.T.);
#14606=EDGE_CURVE('',#11443,#11766,#6704,.T.);
#14607=EDGE_CURVE('',#11766,#11765,#760,.T.);
#14608=EDGE_CURVE('',#11442,#11767,#6705,.T.);
#14609=EDGE_CURVE('',#11767,#11766,#761,.T.);
#14610=EDGE_CURVE('',#11441,#11768,#6706,.T.);
#14611=EDGE_CURVE('',#11768,#11767,#762,.T.);
#14612=EDGE_CURVE('',#11440,#11769,#6707,.T.);
#14613=EDGE_CURVE('',#11769,#11768,#763,.T.);
#14614=EDGE_CURVE('',#11439,#11770,#6708,.T.);
#14615=EDGE_CURVE('',#11770,#11769,#764,.T.);
#14616=EDGE_CURVE('',#11438,#11771,#6709,.T.);
#14617=EDGE_CURVE('',#11771,#11770,#765,.T.);
#14618=EDGE_CURVE('',#11760,#11771,#766,.T.);
#14619=EDGE_CURVE('',#11449,#11772,#6710,.T.);
#14620=EDGE_CURVE('',#11772,#11773,#6711,.T.);
#14621=EDGE_CURVE('',#11450,#11773,#6712,.T.);
#14622=EDGE_CURVE('',#11470,#11774,#6713,.T.);
#14623=EDGE_CURVE('',#11774,#11772,#767,.T.);
#14624=EDGE_CURVE('',#11469,#11775,#6714,.T.);
#14625=EDGE_CURVE('',#11775,#11774,#768,.T.);
#14626=EDGE_CURVE('',#11468,#11776,#6715,.T.);
#14627=EDGE_CURVE('',#11776,#11775,#769,.T.);
#14628=EDGE_CURVE('',#11467,#11777,#6716,.T.);
#14629=EDGE_CURVE('',#11777,#11776,#770,.T.);
#14630=EDGE_CURVE('',#11466,#11778,#6717,.T.);
#14631=EDGE_CURVE('',#11778,#11777,#771,.T.);
#14632=EDGE_CURVE('',#11465,#11779,#6718,.T.);
#14633=EDGE_CURVE('',#11779,#11778,#772,.T.);
#14634=EDGE_CURVE('',#11464,#11780,#6719,.T.);
#14635=EDGE_CURVE('',#11780,#11779,#773,.T.);
#14636=EDGE_CURVE('',#11463,#11781,#6720,.T.);
#14637=EDGE_CURVE('',#11781,#11780,#774,.T.);
#14638=EDGE_CURVE('',#11462,#11782,#6721,.T.);
#14639=EDGE_CURVE('',#11782,#11781,#775,.T.);
#14640=EDGE_CURVE('',#11461,#11783,#6722,.T.);
#14641=EDGE_CURVE('',#11783,#11782,#776,.T.);
#14642=EDGE_CURVE('',#11460,#11784,#6723,.T.);
#14643=EDGE_CURVE('',#11784,#11783,#6724,.T.);
#14644=EDGE_CURVE('',#11459,#11785,#6725,.T.);
#14645=EDGE_CURVE('',#11785,#11784,#777,.T.);
#14646=EDGE_CURVE('',#11458,#11786,#6726,.T.);
#14647=EDGE_CURVE('',#11786,#11785,#778,.T.);
#14648=EDGE_CURVE('',#11457,#11787,#6727,.T.);
#14649=EDGE_CURVE('',#11787,#11786,#779,.T.);
#14650=EDGE_CURVE('',#11456,#11788,#6728,.T.);
#14651=EDGE_CURVE('',#11788,#11787,#780,.T.);
#14652=EDGE_CURVE('',#11455,#11789,#6729,.T.);
#14653=EDGE_CURVE('',#11789,#11788,#781,.T.);
#14654=EDGE_CURVE('',#11454,#11790,#6730,.T.);
#14655=EDGE_CURVE('',#11790,#11789,#782,.T.);
#14656=EDGE_CURVE('',#11453,#11791,#6731,.T.);
#14657=EDGE_CURVE('',#11791,#11790,#783,.T.);
#14658=EDGE_CURVE('',#11452,#11792,#6732,.T.);
#14659=EDGE_CURVE('',#11792,#11791,#784,.T.);
#14660=EDGE_CURVE('',#11451,#11793,#6733,.T.);
#14661=EDGE_CURVE('',#11793,#11792,#6734,.T.);
#14662=EDGE_CURVE('',#11773,#11793,#6735,.T.);
#14663=EDGE_CURVE('',#11471,#11794,#6736,.T.);
#14664=EDGE_CURVE('',#11794,#11795,#6737,.T.);
#14665=EDGE_CURVE('',#11472,#11795,#6738,.T.);
#14666=EDGE_CURVE('',#11480,#11796,#6739,.T.);
#14667=EDGE_CURVE('',#11796,#11794,#6740,.T.);
#14668=EDGE_CURVE('',#11479,#11797,#6741,.T.);
#14669=EDGE_CURVE('',#11797,#11796,#6742,.T.);
#14670=EDGE_CURVE('',#11478,#11798,#6743,.T.);
#14671=EDGE_CURVE('',#11798,#11797,#6744,.T.);
#14672=EDGE_CURVE('',#11477,#11799,#6745,.T.);
#14673=EDGE_CURVE('',#11799,#11798,#6746,.T.);
#14674=EDGE_CURVE('',#11476,#11800,#6747,.T.);
#14675=EDGE_CURVE('',#11800,#11799,#6748,.T.);
#14676=EDGE_CURVE('',#11475,#11801,#6749,.T.);
#14677=EDGE_CURVE('',#11801,#11800,#6750,.T.);
#14678=EDGE_CURVE('',#11474,#11802,#6751,.T.);
#14679=EDGE_CURVE('',#11802,#11801,#6752,.T.);
#14680=EDGE_CURVE('',#11473,#11803,#6753,.T.);
#14681=EDGE_CURVE('',#11803,#11802,#6754,.T.);
#14682=EDGE_CURVE('',#11795,#11803,#6755,.T.);
#14683=EDGE_CURVE('',#11278,#11575,#6756,.T.);
#14684=EDGE_CURVE('',#11389,#11306,#6757,.T.);
#14685=EDGE_CURVE('',#11804,#11805,#6758,.T.);
#14686=EDGE_CURVE('',#11805,#11806,#6759,.F.);
#14687=EDGE_CURVE('',#11806,#11807,#6760,.T.);
#14688=EDGE_CURVE('',#11807,#11804,#6761,.T.);
#14689=EDGE_CURVE('',#11807,#11808,#6762,.T.);
#14690=EDGE_CURVE('',#11808,#11809,#6763,.T.);
#14691=EDGE_CURVE('',#11809,#11810,#6764,.T.);
#14692=EDGE_CURVE('',#11810,#11804,#6765,.T.);
#14693=EDGE_CURVE('',#11804,#11811,#6766,.T.);
#14694=EDGE_CURVE('',#11812,#11811,#6767,.T.);
#14695=EDGE_CURVE('',#11805,#11812,#6768,.T.);
#14696=EDGE_CURVE('',#11813,#11810,#6769,.T.);
#14697=EDGE_CURVE('',#11811,#11813,#6770,.T.);
#14698=EDGE_CURVE('',#11809,#11814,#6771,.T.);
#14699=EDGE_CURVE('',#11814,#11815,#6772,.T.);
#14700=EDGE_CURVE('',#11815,#11816,#6773,.T.);
#14701=EDGE_CURVE('',#11813,#11816,#6774,.T.);
#14702=EDGE_CURVE('',#11817,#11818,#6775,.T.);
#14703=EDGE_CURVE('',#11818,#11819,#6776,.T.);
#14704=EDGE_CURVE('',#11819,#11820,#6777,.T.);
#14705=EDGE_CURVE('',#11820,#11821,#6778,.T.);
#14706=EDGE_CURVE('',#11821,#11817,#6779,.T.);
#14707=EDGE_CURVE('',#11822,#11817,#6780,.T.);
#14708=EDGE_CURVE('',#11821,#11823,#6781,.T.);
#14709=EDGE_CURVE('',#11823,#11822,#6782,.T.);
#14710=EDGE_CURVE('',#11823,#11824,#6783,.T.);
#14711=EDGE_CURVE('',#11824,#11825,#6784,.T.);
#14712=EDGE_CURVE('',#11825,#11826,#6785,.T.);
#14713=EDGE_CURVE('',#11826,#11822,#6786,.T.);
#14714=EDGE_CURVE('',#11818,#11827,#6787,.T.);
#14715=EDGE_CURVE('',#11827,#11828,#6788,.T.);
#14716=EDGE_CURVE('',#11828,#11829,#6789,.T.);
#14717=EDGE_CURVE('',#11829,#11830,#6790,.T.);
#14718=EDGE_CURVE('',#11830,#11819,#6791,.T.);
#14719=EDGE_CURVE('',#11817,#11831,#6792,.T.);
#14720=EDGE_CURVE('',#11827,#11831,#6793,.T.);
#14721=EDGE_CURVE('',#11822,#11832,#6794,.T.);
#14722=EDGE_CURVE('',#11831,#11832,#6795,.T.);
#14723=EDGE_CURVE('',#11833,#11826,#6796,.T.);
#14724=EDGE_CURVE('',#11832,#11833,#6797,.T.);
#14725=EDGE_CURVE('',#11825,#11834,#6798,.T.);
#14726=EDGE_CURVE('',#11834,#11835,#6799,.T.);
#14727=EDGE_CURVE('',#11835,#11836,#6800,.T.);
#14728=EDGE_CURVE('',#11833,#11836,#6801,.T.);
#14729=EDGE_CURVE('',#11837,#11838,#6802,.T.);
#14730=EDGE_CURVE('',#11838,#11839,#6803,.T.);
#14731=EDGE_CURVE('',#11839,#11840,#6804,.T.);
#14732=EDGE_CURVE('',#11840,#11841,#6805,.T.);
#14733=EDGE_CURVE('',#11841,#11842,#6806,.T.);
#14734=EDGE_CURVE('',#11842,#11837,#6807,.T.);
#14735=EDGE_CURVE('',#11837,#11843,#6808,.T.);
#14736=EDGE_CURVE('',#11843,#11844,#6809,.T.);
#14737=EDGE_CURVE('',#11844,#11845,#6810,.T.);
#14738=EDGE_CURVE('',#11845,#11838,#6811,.T.);
#14739=EDGE_CURVE('',#11842,#11846,#6812,.T.);
#14740=EDGE_CURVE('',#11847,#11846,#6813,.T.);
#14741=EDGE_CURVE('',#11848,#11847,#6814,.T.);
#14742=EDGE_CURVE('',#11848,#11843,#6815,.T.);
#14743=EDGE_CURVE('',#11846,#11806,#6816,.T.);
#14744=EDGE_CURVE('',#11849,#11841,#6817,.T.);
#14745=EDGE_CURVE('',#11850,#11849,#6818,.T.);
#14746=EDGE_CURVE('',#11808,#11850,#6819,.T.);
#14747=EDGE_CURVE('',#11851,#11852,#6820,.T.);
#14748=EDGE_CURVE('',#11852,#11853,#6821,.T.);
#14749=EDGE_CURVE('',#11853,#11854,#6822,.T.);
#14750=EDGE_CURVE('',#11854,#11855,#6823,.T.);
#14751=EDGE_CURVE('',#11855,#11851,#6824,.T.);
#14752=EDGE_CURVE('',#11855,#11856,#6825,.T.);
#14753=EDGE_CURVE('',#11856,#11857,#6826,.T.);
#14754=EDGE_CURVE('',#11857,#11858,#6827,.T.);
#14755=EDGE_CURVE('',#11858,#11851,#6828,.T.);
#14756=EDGE_CURVE('',#11859,#11858,#6829,.T.);
#14757=EDGE_CURVE('',#11844,#11859,#6830,.T.);
#14758=EDGE_CURVE('',#11860,#11848,#6831,.T.);
#14759=EDGE_CURVE('',#11852,#11860,#6832,.T.);
#14760=EDGE_CURVE('',#11861,#11857,#6833,.T.);
#14761=EDGE_CURVE('',#11861,#11862,#6834,.T.);
#14762=EDGE_CURVE('',#11862,#11863,#6835,.T.);
#14763=EDGE_CURVE('',#11859,#11863,#6836,.T.);
#14764=EDGE_CURVE('',#11856,#11864,#6837,.T.);
#14765=EDGE_CURVE('',#11865,#11864,#6838,.T.);
#14766=EDGE_CURVE('',#11866,#11865,#6839,.T.);
#14767=EDGE_CURVE('',#11866,#11861,#6840,.T.);
#14768=EDGE_CURVE('',#11805,#11867,#6841,.T.);
#14769=EDGE_CURVE('',#11867,#11847,#6842,.T.);
#14770=EDGE_CURVE('',#11867,#11868,#6843,.T.);
#14771=EDGE_CURVE('',#11868,#11869,#6844,.T.);
#14772=EDGE_CURVE('',#11869,#11860,#6845,.T.);
#14773=EDGE_CURVE('',#11870,#11869,#6846,.T.);
#14774=EDGE_CURVE('',#11870,#11871,#6847,.T.);
#14775=EDGE_CURVE('',#11853,#11871,#6848,.T.);
#14776=EDGE_CURVE('',#11868,#11812,#6849,.T.);
#14777=EDGE_CURVE('',#11872,#11812,#6850,.T.);
#14778=EDGE_CURVE('',#11872,#11870,#6851,.T.);
#14779=EDGE_CURVE('',#11830,#11873,#6852,.T.);
#14780=EDGE_CURVE('',#11874,#11873,#6853,.T.);
#14781=EDGE_CURVE('',#11875,#11874,#6854,.T.);
#14782=EDGE_CURVE('',#11875,#11820,#6855,.T.);
#14783=EDGE_CURVE('',#11876,#11829,#6856,.T.);
#14784=EDGE_CURVE('',#11877,#11876,#6857,.T.);
#14785=EDGE_CURVE('',#11878,#11877,#6858,.T.);
#14786=EDGE_CURVE('',#11879,#11878,#6859,.T.);
#14787=EDGE_CURVE('',#11880,#11879,#6860,.T.);
#14788=EDGE_CURVE('',#11873,#11880,#6861,.T.);
#14789=EDGE_CURVE('',#11880,#11881,#6862,.F.);
#14790=EDGE_CURVE('',#11881,#11882,#6863,.T.);
#14791=EDGE_CURVE('',#11882,#11874,#6864,.T.);
#14792=EDGE_CURVE('',#11882,#11883,#6865,.T.);
#14793=EDGE_CURVE('',#11883,#11884,#6866,.T.);
#14794=EDGE_CURVE('',#11884,#11875,#6867,.T.);
#14795=EDGE_CURVE('',#11863,#11885,#6868,.T.);
#14796=EDGE_CURVE('',#11885,#11845,#6869,.T.);
#14797=EDGE_CURVE('',#11845,#11886,#6870,.T.);
#14798=EDGE_CURVE('',#11839,#11886,#6871,.T.);
#14799=EDGE_CURVE('',#11887,#11885,#6872,.T.);
#14800=EDGE_CURVE('',#11888,#11887,#6873,.T.);
#14801=EDGE_CURVE('',#11889,#11888,#6874,.T.);
#14802=EDGE_CURVE('',#11890,#11889,#6875,.F.);
#14803=EDGE_CURVE('',#11891,#11890,#6876,.T.);
#14804=EDGE_CURVE('',#11892,#11891,#6877,.T.);
#14805=EDGE_CURVE('',#11892,#11893,#6878,.T.);
#14806=EDGE_CURVE('',#11893,#11886,#6879,.T.);
#14807=EDGE_CURVE('',#11862,#11894,#6880,.T.);
#14808=EDGE_CURVE('',#11894,#11895,#6881,.T.);
#14809=EDGE_CURVE('',#11887,#11895,#6882,.T.);
#14810=EDGE_CURVE('',#11896,#11883,#6883,.T.);
#14811=EDGE_CURVE('',#11884,#11896,#6884,.T.);
#14812=EDGE_CURVE('',#11897,#11898,#6885,.T.);
#14813=EDGE_CURVE('',#11898,#11884,#6886,.T.);
#14814=EDGE_CURVE('',#11896,#11899,#6887,.T.);
#14815=EDGE_CURVE('',#11899,#11897,#6888,.T.);
#14816=EDGE_CURVE('',#11900,#11901,#6889,.F.);
#14817=EDGE_CURVE('',#11901,#11896,#6890,.T.);
#14818=EDGE_CURVE('',#11883,#11900,#6891,.T.);
#14819=EDGE_CURVE('',#11902,#11898,#6892,.T.);
#14820=EDGE_CURVE('',#11824,#11902,#6893,.T.);
#14821=EDGE_CURVE('',#11897,#11903,#6894,.T.);
#14822=EDGE_CURVE('',#11903,#11904,#6895,.T.);
#14823=EDGE_CURVE('',#11905,#11904,#6896,.T.);
#14824=EDGE_CURVE('',#11905,#11902,#6897,.T.);
#14825=EDGE_CURVE('',#11899,#11890,#6898,.T.);
#14826=EDGE_CURVE('',#11889,#11903,#6899,.T.);
#14827=EDGE_CURVE('',#11901,#11906,#6900,.T.);
#14828=EDGE_CURVE('',#11906,#11907,#6901,.T.);
#14829=EDGE_CURVE('',#11907,#11908,#6902,.T.);
#14830=EDGE_CURVE('',#11909,#11908,#6903,.F.);
#14831=EDGE_CURVE('',#11910,#11909,#6904,.T.);
#14832=EDGE_CURVE('',#11911,#11910,#6905,.T.);
#14833=EDGE_CURVE('',#11912,#11911,#6906,.T.);
#14834=EDGE_CURVE('',#11913,#11912,#6907,.T.);
#14835=EDGE_CURVE('',#11913,#11914,#6908,.T.);
#14836=EDGE_CURVE('',#11914,#11915,#6909,.T.);
#14837=EDGE_CURVE('',#11916,#11915,#6910,.T.);
#14838=EDGE_CURVE('',#11891,#11916,#6911,.F.);
#14839=EDGE_CURVE('',#11917,#11918,#6912,.T.);
#14840=EDGE_CURVE('',#11918,#11919,#6913,.T.);
#14841=EDGE_CURVE('',#11919,#11913,#6914,.F.);
#14842=EDGE_CURVE('',#11912,#11917,#6915,.T.);
#14843=EDGE_CURVE('',#11920,#11917,#6916,.T.);
#14844=EDGE_CURVE('',#11920,#11921,#6917,.T.);
#14845=EDGE_CURVE('',#11921,#11922,#6918,.T.);
#14846=EDGE_CURVE('',#11922,#11923,#6919,.T.);
#14847=EDGE_CURVE('',#11923,#11918,#6920,.T.);
#14848=EDGE_CURVE('',#11924,#11911,#6921,.T.);
#14849=EDGE_CURVE('',#11925,#11924,#6922,.T.);
#14850=EDGE_CURVE('',#11925,#11920,#6923,.T.);
#14851=EDGE_CURVE('',#11876,#11926,#6924,.T.);
#14852=EDGE_CURVE('',#11926,#11927,#6925,.T.);
#14853=EDGE_CURVE('',#11927,#11928,#6926,.T.);
#14854=EDGE_CURVE('',#11928,#11877,#6927,.T.);
#14855=EDGE_CURVE('',#11928,#11929,#6928,.T.);
#14856=EDGE_CURVE('',#11929,#11930,#6929,.T.);
#14857=EDGE_CURVE('',#11930,#11878,#6930,.T.);
#14858=EDGE_CURVE('',#11931,#11828,#6931,.T.);
#14859=EDGE_CURVE('',#11931,#11932,#6932,.T.);
#14860=EDGE_CURVE('',#11926,#11932,#6933,.T.);
#14861=EDGE_CURVE('',#11933,#11930,#6934,.T.);
#14862=EDGE_CURVE('',#11933,#11934,#6935,.T.);
#14863=EDGE_CURVE('',#11935,#11934,#6936,.T.);
#14864=EDGE_CURVE('',#11879,#11935,#6937,.T.);
#14865=EDGE_CURVE('',#11936,#11937,#6938,.F.);
#14866=EDGE_CURVE('',#11937,#11909,#6939,.T.);
#14867=EDGE_CURVE('',#11908,#11936,#6940,.T.);
#14868=EDGE_CURVE('',#11938,#11928,#6941,.T.);
#14869=EDGE_CURVE('',#11910,#11938,#6942,.F.);
#14870=EDGE_CURVE('',#11937,#11939,#6943,.T.);
#14871=EDGE_CURVE('',#11939,#11940,#6944,.T.);
#14872=EDGE_CURVE('',#11941,#11940,#6945,.T.);
#14873=EDGE_CURVE('',#11942,#11941,#6946,.T.);
#14874=EDGE_CURVE('',#11929,#11942,#6947,.T.);
#14875=EDGE_CURVE('',#11938,#11943,#6948,.T.);
#14876=EDGE_CURVE('',#11943,#11924,#6949,.T.);
#14877=EDGE_CURVE('',#11932,#11925,#6950,.T.);
#14878=EDGE_CURVE('',#11943,#11927,#6951,.T.);
#14879=EDGE_CURVE('',#11836,#11944,#6952,.T.);
#14880=EDGE_CURVE('',#11944,#11945,#6953,.T.);
#14881=EDGE_CURVE('',#11945,#11832,#6954,.T.);
#14882=EDGE_CURVE('',#11945,#11946,#6955,.T.);
#14883=EDGE_CURVE('',#11946,#11831,#6956,.T.);
#14884=EDGE_CURVE('',#11946,#11931,#6957,.T.);
#14885=EDGE_CURVE('',#11921,#11944,#6958,.T.);
#14886=EDGE_CURVE('',#11835,#11947,#6959,.T.);
#14887=EDGE_CURVE('',#11922,#11947,#6960,.T.);
#14888=EDGE_CURVE('',#11948,#11923,#6961,.T.);
#14889=EDGE_CURVE('',#11948,#11919,#6962,.T.);
#14890=EDGE_CURVE('',#11947,#11949,#6963,.T.);
#14891=EDGE_CURVE('',#11949,#11948,#6964,.T.);
#14892=EDGE_CURVE('',#11950,#11834,#6965,.T.);
#14893=EDGE_CURVE('',#11951,#11950,#6966,.T.);
#14894=EDGE_CURVE('',#11952,#11951,#6967,.T.);
#14895=EDGE_CURVE('',#11953,#11952,#6968,.T.);
#14896=EDGE_CURVE('',#11949,#11953,#6969,.T.);
#14897=EDGE_CURVE('',#11953,#11865,#6970,.T.);
#14898=EDGE_CURVE('',#11864,#11948,#6971,.T.);
#14899=EDGE_CURVE('',#11895,#11952,#6972,.T.);
#14900=EDGE_CURVE('',#11894,#11866,#6973,.T.);
#14901=EDGE_CURVE('',#11951,#11888,#6974,.T.);
#14902=EDGE_CURVE('',#11950,#11905,#6975,.T.);
#14903=EDGE_CURVE('',#11904,#11888,#6976,.T.);
#14904=EDGE_CURVE('',#11935,#11954,#6977,.T.);
#14905=EDGE_CURVE('',#11954,#11881,#6978,.T.);
#14906=EDGE_CURVE('',#11906,#11955,#6979,.T.);
#14907=EDGE_CURVE('',#11955,#11956,#6980,.F.);
#14908=EDGE_CURVE('',#11956,#11907,#6981,.T.);
#14909=EDGE_CURVE('',#11957,#11954,#6982,.T.);
#14910=EDGE_CURVE('',#11958,#11957,#6983,.T.);
#14911=EDGE_CURVE('',#11959,#11958,#6984,.T.);
#14912=EDGE_CURVE('',#11960,#11959,#6985,.F.);
#14913=EDGE_CURVE('',#11960,#11955,#6986,.T.);
#14914=EDGE_CURVE('',#11881,#11900,#6987,.T.);
#14915=EDGE_CURVE('',#11914,#11961,#6988,.T.);
#14916=EDGE_CURVE('',#11961,#11962,#6989,.F.);
#14917=EDGE_CURVE('',#11962,#11915,#6990,.T.);
#14918=EDGE_CURVE('',#11963,#11962,#6991,.T.);
#14919=EDGE_CURVE('',#11916,#11963,#6992,.T.);
#14920=EDGE_CURVE('',#11964,#11964,#2197,.T.);
#14921=EDGE_CURVE('',#11965,#11965,#2198,.T.);
#14922=EDGE_CURVE('',#11966,#11967,#6993,.T.);
#14923=EDGE_CURVE('',#11967,#11968,#6994,.T.);
#14924=EDGE_CURVE('',#11968,#11969,#6995,.F.);
#14925=EDGE_CURVE('',#11969,#11970,#6996,.T.);
#14926=EDGE_CURVE('',#11970,#11966,#6997,.T.);
#14927=EDGE_CURVE('',#11968,#11961,#6998,.T.);
#14928=EDGE_CURVE('',#11971,#11967,#6999,.T.);
#14929=EDGE_CURVE('',#11939,#11971,#7000,.T.);
#14930=EDGE_CURVE('',#11956,#11936,#7001,.T.);
#14931=EDGE_CURVE('',#11972,#11960,#7002,.T.);
#14932=EDGE_CURVE('',#11973,#11972,#7003,.T.);
#14933=EDGE_CURVE('',#11893,#11973,#7004,.T.);
#14934=EDGE_CURVE('',#11963,#11892,#7005,.F.);
#14935=EDGE_CURVE('',#11974,#11966,#7006,.T.);
#14936=EDGE_CURVE('',#11974,#11975,#7007,.T.);
#14937=EDGE_CURVE('',#11975,#11971,#7008,.T.);
#14938=EDGE_CURVE('',#11871,#11974,#7009,.T.);
#14939=EDGE_CURVE('',#11970,#11854,#7010,.T.);
#14940=EDGE_CURVE('',#11840,#11973,#7011,.T.);
#14941=EDGE_CURVE('',#11972,#11976,#7012,.T.);
#14942=EDGE_CURVE('',#11976,#11849,#7013,.T.);
#14943=EDGE_CURVE('',#11959,#11977,#7014,.T.);
#14944=EDGE_CURVE('',#11976,#11977,#7015,.T.);
#14945=EDGE_CURVE('',#11816,#11978,#7016,.T.);
#14946=EDGE_CURVE('',#11978,#11979,#7017,.T.);
#14947=EDGE_CURVE('',#11979,#11811,#7018,.T.);
#14948=EDGE_CURVE('',#11979,#11872,#7019,.T.);
#14949=EDGE_CURVE('',#11980,#11978,#7020,.T.);
#14950=EDGE_CURVE('',#11975,#11980,#7021,.T.);
#14951=EDGE_CURVE('',#11815,#11981,#7022,.T.);
#14952=EDGE_CURVE('',#11982,#11981,#7023,.T.);
#14953=EDGE_CURVE('',#11980,#11982,#7024,.T.);
#14954=EDGE_CURVE('',#11983,#11975,#7025,.T.);
#14955=EDGE_CURVE('',#11971,#11983,#7026,.T.);
#14956=EDGE_CURVE('',#11983,#11940,#7027,.T.);
#14957=EDGE_CURVE('',#11982,#11984,#7028,.T.);
#14958=EDGE_CURVE('',#11984,#11983,#7029,.T.);
#14959=EDGE_CURVE('',#11941,#11984,#7030,.T.);
#14960=EDGE_CURVE('',#11981,#11985,#7031,.T.);
#14961=EDGE_CURVE('',#11985,#11941,#7032,.T.);
#14962=EDGE_CURVE('',#11977,#11986,#7033,.T.);
#14963=EDGE_CURVE('',#11986,#11987,#7034,.T.);
#14964=EDGE_CURVE('',#11987,#11850,#7035,.T.);
#14965=EDGE_CURVE('',#11986,#11958,#7036,.T.);
#14966=EDGE_CURVE('',#11988,#11958,#7037,.T.);
#14967=EDGE_CURVE('',#11988,#11989,#7038,.T.);
#14968=EDGE_CURVE('',#11989,#11987,#7039,.T.);
#14969=EDGE_CURVE('',#11989,#11814,#7040,.T.);
#14970=EDGE_CURVE('',#11990,#11988,#7041,.T.);
#14971=EDGE_CURVE('',#11991,#11990,#7042,.T.);
#14972=EDGE_CURVE('',#11985,#11991,#7043,.T.);
#14973=EDGE_CURVE('',#11991,#11992,#7044,.T.);
#14974=EDGE_CURVE('',#11992,#11942,#7045,.T.);
#14975=EDGE_CURVE('',#11993,#11992,#7046,.T.);
#14976=EDGE_CURVE('',#11993,#11933,#7047,.T.);
#14977=EDGE_CURVE('',#11994,#11990,#7048,.T.);
#14978=EDGE_CURVE('',#11995,#11994,#7049,.T.);
#14979=EDGE_CURVE('',#11995,#11993,#7050,.T.);
#14980=EDGE_CURVE('',#11957,#11994,#7051,.T.);
#14981=EDGE_CURVE('',#11934,#11995,#7052,.T.);
#14982=EDGE_CURVE('',#11996,#11997,#2199,.T.);
#14983=EDGE_CURVE('',#11997,#11996,#2200,.T.);
#14984=EDGE_CURVE('',#11996,#11998,#7053,.T.);
#14985=EDGE_CURVE('',#11998,#11999,#2201,.T.);
#14986=EDGE_CURVE('',#11999,#11998,#2202,.T.);
#14987=EDGE_CURVE('',#11999,#12000,#7054,.T.);
#14988=EDGE_CURVE('',#12001,#12000,#2203,.T.);
#14989=EDGE_CURVE('',#12000,#12001,#2204,.T.);
#14990=EDGE_CURVE('',#12002,#12002,#2205,.T.);
#14991=EDGE_CURVE('',#12002,#11997,#7055,.T.);
#14992=EDGE_CURVE('',#12001,#12003,#7056,.T.);
#14993=EDGE_CURVE('',#12003,#12003,#2206,.T.);
#14994=EDGE_CURVE('',#11965,#12004,#7057,.T.);
#14995=EDGE_CURVE('',#12004,#12004,#2207,.T.);
#14996=EDGE_CURVE('',#12004,#12005,#7058,.T.);
#14997=EDGE_CURVE('',#12005,#12005,#2208,.T.);
#14998=EDGE_CURVE('',#12006,#12006,#2209,.T.);
#14999=EDGE_CURVE('',#12006,#12005,#7059,.T.);
#15000=EDGE_CURVE('',#12007,#12007,#2210,.T.);
#15001=EDGE_CURVE('',#11964,#12008,#7060,.T.);
#15002=EDGE_CURVE('',#12008,#12008,#2211,.T.);
#15003=EDGE_CURVE('',#12008,#12009,#7061,.T.);
#15004=EDGE_CURVE('',#12009,#12009,#2212,.T.);
#15005=EDGE_CURVE('',#12007,#12009,#7062,.T.);
#15006=EDGE_CURVE('',#12010,#12010,#2213,.T.);
#15007=EDGE_CURVE('',#12010,#12002,#7063,.T.);
#15008=EDGE_CURVE('',#11969,#11855,#7064,.T.);
#15009=EDGE_CURVE('',#12011,#12012,#7065,.F.);
#15010=EDGE_CURVE('',#12012,#12013,#7066,.T.);
#15011=EDGE_CURVE('',#12013,#12014,#7067,.F.);
#15012=EDGE_CURVE('',#12014,#12011,#7068,.T.);
#15013=EDGE_CURVE('',#12015,#12012,#7069,.T.);
#15014=EDGE_CURVE('',#12016,#12015,#7070,.T.);
#15015=EDGE_CURVE('',#12013,#12016,#7071,.T.);
#15016=EDGE_CURVE('',#12017,#12018,#7072,.T.);
#15017=EDGE_CURVE('',#12018,#12019,#7073,.T.);
#15018=EDGE_CURVE('',#12019,#12020,#7074,.T.);
#15019=EDGE_CURVE('',#12020,#12021,#7075,.T.);
#15020=EDGE_CURVE('',#12021,#12022,#7076,.T.);
#15021=EDGE_CURVE('',#12022,#12017,#7077,.T.);
#15022=EDGE_CURVE('',#12023,#12021,#7078,.T.);
#15023=EDGE_CURVE('',#12024,#12023,#7079,.T.);
#15024=EDGE_CURVE('',#12022,#12024,#7080,.T.);
#15025=EDGE_CURVE('',#12025,#12020,#7081,.T.);
#15026=EDGE_CURVE('',#12025,#12026,#7082,.T.);
#15027=EDGE_CURVE('',#12027,#12026,#7083,.T.);
#15028=EDGE_CURVE('',#12023,#12027,#7084,.T.);
#15029=EDGE_CURVE('',#12019,#12028,#7085,.T.);
#15030=EDGE_CURVE('',#12029,#12028,#7086,.T.);
#15031=EDGE_CURVE('',#12030,#12029,#7087,.T.);
#15032=EDGE_CURVE('',#12030,#12025,#7088,.T.);
#15033=EDGE_CURVE('',#12031,#12032,#7089,.F.);
#15034=EDGE_CURVE('',#12032,#12033,#7090,.T.);
#15035=EDGE_CURVE('',#12033,#12034,#7091,.F.);
#15036=EDGE_CURVE('',#12034,#12031,#7092,.T.);
#15037=EDGE_CURVE('',#12033,#12014,#7093,.T.);
#15038=EDGE_CURVE('',#12011,#12032,#7094,.T.);
#15039=EDGE_CURVE('',#12035,#12036,#7095,.F.);
#15040=EDGE_CURVE('',#12036,#12037,#7096,.T.);
#15041=EDGE_CURVE('',#12037,#12038,#7097,.F.);
#15042=EDGE_CURVE('',#12038,#12035,#7098,.T.);
#15043=EDGE_CURVE('',#12039,#12036,#7099,.T.);
#15044=EDGE_CURVE('',#12040,#12039,#7100,.T.);
#15045=EDGE_CURVE('',#12037,#12040,#7101,.T.);
#15046=EDGE_CURVE('',#12041,#12042,#7102,.T.);
#15047=EDGE_CURVE('',#12042,#12043,#7103,.T.);
#15048=EDGE_CURVE('',#12043,#12044,#7104,.T.);
#15049=EDGE_CURVE('',#12044,#12045,#7105,.T.);
#15050=EDGE_CURVE('',#12045,#12046,#7106,.T.);
#15051=EDGE_CURVE('',#12046,#12041,#7107,.T.);
#15052=EDGE_CURVE('',#12046,#12047,#7108,.T.);
#15053=EDGE_CURVE('',#12048,#12047,#7109,.T.);
#15054=EDGE_CURVE('',#12049,#12048,#7110,.T.);
#15055=EDGE_CURVE('',#12049,#12050,#7111,.T.);
#15056=EDGE_CURVE('',#12041,#12050,#7112,.T.);
#15057=EDGE_CURVE('',#12051,#12045,#7113,.T.);
#15058=EDGE_CURVE('',#12047,#12051,#7114,.T.);
#15059=EDGE_CURVE('',#12052,#12044,#7115,.T.);
#15060=EDGE_CURVE('',#12052,#12053,#7116,.T.);
#15061=EDGE_CURVE('',#12054,#12053,#7117,.T.);
#15062=EDGE_CURVE('',#12051,#12054,#7118,.T.);
#15063=EDGE_CURVE('',#12054,#12055,#7119,.T.);
#15064=EDGE_CURVE('',#12055,#12056,#7120,.T.);
#15065=EDGE_CURVE('',#12056,#12048,#7121,.T.);
#15066=EDGE_CURVE('',#12056,#12057,#7122,.T.);
#15067=EDGE_CURVE('',#12057,#12058,#7123,.T.);
#15068=EDGE_CURVE('',#12058,#12049,#7124,.T.);
#15069=EDGE_CURVE('',#12059,#12055,#7125,.T.);
#15070=EDGE_CURVE('',#12057,#12059,#7126,.T.);
#15071=EDGE_CURVE('',#12053,#12060,#7127,.T.);
#15072=EDGE_CURVE('',#12060,#12061,#7128,.T.);
#15073=EDGE_CURVE('',#12059,#12061,#7129,.T.);
#15074=EDGE_CURVE('',#12050,#12062,#7130,.T.);
#15075=EDGE_CURVE('',#12062,#12063,#7131,.T.);
#15076=EDGE_CURVE('',#12063,#12042,#7132,.T.);
#15077=EDGE_CURVE('',#12062,#12064,#7133,.T.);
#15078=EDGE_CURVE('',#12064,#12065,#7134,.F.);
#15079=EDGE_CURVE('',#12065,#12063,#7135,.T.);
#15080=EDGE_CURVE('',#12066,#12063,#7136,.T.);
#15081=EDGE_CURVE('',#12043,#12066,#7137,.T.);
#15082=EDGE_CURVE('',#12067,#12065,#7138,.T.);
#15083=EDGE_CURVE('',#12066,#12067,#7139,.T.);
#15084=EDGE_CURVE('',#12068,#12069,#7140,.F.);
#15085=EDGE_CURVE('',#12069,#12070,#7141,.T.);
#15086=EDGE_CURVE('',#12070,#12071,#7142,.F.);
#15087=EDGE_CURVE('',#12071,#12068,#7143,.T.);
#15088=EDGE_CURVE('',#12070,#12038,#7144,.T.);
#15089=EDGE_CURVE('',#12035,#12069,#7145,.T.);
#15090=EDGE_CURVE('',#12072,#12057,#7146,.T.);
#15091=EDGE_CURVE('',#12058,#12072,#7147,.T.);
#15092=EDGE_CURVE('',#12061,#12073,#7148,.T.);
#15093=EDGE_CURVE('',#12073,#12072,#7149,.T.);
#15094=EDGE_CURVE('',#12074,#12075,#7150,.T.);
#15095=EDGE_CURVE('',#12076,#12074,#7151,.T.);
#15096=EDGE_CURVE('',#12075,#12076,#7152,.T.);
#15097=EDGE_CURVE('',#12028,#12076,#7153,.T.);
#15098=EDGE_CURVE('',#12074,#12077,#7154,.T.);
#15099=EDGE_CURVE('',#12077,#12029,#7155,.T.);
#15100=EDGE_CURVE('',#12017,#12078,#7156,.T.);
#15101=EDGE_CURVE('',#12078,#12075,#7157,.T.);
#15102=EDGE_CURVE('',#12076,#12018,#7158,.T.);
#15103=EDGE_CURVE('',#12015,#12074,#7159,.T.);
#15104=EDGE_CURVE('',#12075,#12079,#7160,.T.);
#15105=EDGE_CURVE('',#12079,#12015,#7161,.T.);
#15106=EDGE_CURVE('',#12079,#12080,#7162,.T.);
#15107=EDGE_CURVE('',#12080,#12016,#7163,.T.);
#15108=EDGE_CURVE('',#12080,#12058,#7164,.T.);
#15109=EDGE_CURVE('',#12072,#12016,#7165,.T.);
#15110=EDGE_CURVE('',#12060,#12081,#7166,.T.);
#15111=EDGE_CURVE('',#12081,#12039,#7167,.T.);
#15112=EDGE_CURVE('',#12039,#12073,#7168,.T.);
#15113=EDGE_CURVE('',#12082,#12078,#7169,.T.);
#15114=EDGE_CURVE('',#12083,#12082,#7170,.T.);
#15115=EDGE_CURVE('',#12084,#12083,#7171,.T.);
#15116=EDGE_CURVE('',#12085,#12084,#7172,.T.);
#15117=EDGE_CURVE('',#12086,#12085,#7173,.T.);
#15118=EDGE_CURVE('',#12087,#12086,#7174,.T.);
#15119=EDGE_CURVE('',#12088,#12087,#7175,.T.);
#15120=EDGE_CURVE('',#12089,#12088,#7176,.T.);
#15121=EDGE_CURVE('',#12090,#12089,#7177,.T.);
#15122=EDGE_CURVE('',#12091,#12090,#7178,.T.);
#15123=EDGE_CURVE('',#12092,#12091,#7179,.T.);
#15124=EDGE_CURVE('',#12064,#12092,#7180,.T.);
#15125=EDGE_CURVE('',#12093,#12024,#7181,.T.);
#15126=EDGE_CURVE('',#12027,#12094,#7182,.T.);
#15127=EDGE_CURVE('',#12094,#12095,#7183,.T.);
#15128=EDGE_CURVE('',#12095,#12093,#7184,.T.);
#15129=EDGE_CURVE('',#12095,#12096,#7185,.T.);
#15130=EDGE_CURVE('',#12083,#12096,#7186,.T.);
#15131=EDGE_CURVE('',#12082,#12093,#7187,.T.);
#15132=EDGE_CURVE('',#12097,#12094,#7188,.T.);
#15133=EDGE_CURVE('',#12097,#12096,#7189,.T.);
#15134=EDGE_CURVE('',#12026,#12098,#7190,.T.);
#15135=EDGE_CURVE('',#12098,#12097,#7191,.T.);
#15136=EDGE_CURVE('',#12096,#12099,#7192,.T.);
#15137=EDGE_CURVE('',#12099,#12084,#7193,.F.);
#15138=EDGE_CURVE('',#12100,#12101,#7194,.T.);
#15139=EDGE_CURVE('',#12101,#12102,#7195,.T.);
#15140=EDGE_CURVE('',#12102,#12090,#7196,.T.);
#15141=EDGE_CURVE('',#12089,#12100,#7197,.T.);
#15142=EDGE_CURVE('',#12088,#12103,#7198,.T.);
#15143=EDGE_CURVE('',#12103,#12100,#7199,.T.);
#15144=EDGE_CURVE('',#12104,#12087,#7200,.T.);
#15145=EDGE_CURVE('',#12105,#12104,#7201,.T.);
#15146=EDGE_CURVE('',#12087,#12105,#7202,.T.);
#15147=EDGE_CURVE('',#12106,#12107,#7203,.T.);
#15148=EDGE_CURVE('',#12107,#12105,#7204,.T.);
#15149=EDGE_CURVE('',#12104,#12108,#7205,.T.);
#15150=EDGE_CURVE('',#12108,#12106,#7206,.T.);
#15151=EDGE_CURVE('',#12105,#12103,#7207,.T.);
#15152=EDGE_CURVE('',#12109,#12110,#7208,.T.);
#15153=EDGE_CURVE('',#12110,#12104,#7209,.T.);
#15154=EDGE_CURVE('',#12086,#12109,#7210,.T.);
#15155=EDGE_CURVE('',#12100,#12034,#7211,.T.);
#15156=EDGE_CURVE('',#12031,#12103,#7212,.T.);
#15157=EDGE_CURVE('',#12111,#12107,#7213,.T.);
#15158=EDGE_CURVE('',#12111,#12071,#7214,.T.);
#15159=EDGE_CURVE('',#12077,#12040,#7215,.T.);
#15160=EDGE_CURVE('',#12112,#12106,#7216,.T.);
#15161=EDGE_CURVE('',#12112,#12113,#7217,.T.);
#15162=EDGE_CURVE('',#12113,#12111,#7218,.T.);
#15163=EDGE_CURVE('',#12108,#12114,#7219,.T.);
#15164=EDGE_CURVE('',#12115,#12114,#7220,.T.);
#15165=EDGE_CURVE('',#12115,#12116,#7221,.T.);
#15166=EDGE_CURVE('',#12116,#12112,#7222,.T.);
#15167=EDGE_CURVE('',#12114,#12110,#7223,.T.);
#15168=EDGE_CURVE('',#12117,#12118,#7224,.T.);
#15169=EDGE_CURVE('',#12119,#12117,#2214,.T.);
#15170=EDGE_CURVE('',#12120,#12119,#7225,.T.);
#15171=EDGE_CURVE('',#12118,#12120,#2215,.T.);
#15172=EDGE_CURVE('',#12109,#12121,#7226,.T.);
#15173=EDGE_CURVE('',#12121,#12122,#7227,.T.);
#15174=EDGE_CURVE('',#12122,#12115,#7228,.T.);
#15175=EDGE_CURVE('',#12122,#12123,#7229,.T.);
#15176=EDGE_CURVE('',#12124,#12123,#7230,.T.);
#15177=EDGE_CURVE('',#12125,#12124,#7231,.T.);
#15178=EDGE_CURVE('',#12125,#12116,#7232,.T.);
#15179=EDGE_CURVE('',#12126,#12127,#7233,.T.);
#15180=EDGE_CURVE('',#12127,#12128,#7234,.T.);
#15181=EDGE_CURVE('',#12128,#12124,#7235,.T.);
#15182=EDGE_CURVE('',#12123,#12129,#7236,.T.);
#15183=EDGE_CURVE('',#12129,#12126,#7237,.T.);
#15184=EDGE_CURVE('',#12128,#12130,#7238,.T.);
#15185=EDGE_CURVE('',#12131,#12130,#7239,.T.);
#15186=EDGE_CURVE('',#12131,#12125,#7240,.T.);
#15187=EDGE_CURVE('',#12099,#12127,#7241,.T.);
#15188=EDGE_CURVE('',#12130,#12099,#7242,.T.);
#15189=EDGE_CURVE('',#12132,#12133,#7243,.T.);
#15190=EDGE_CURVE('',#12134,#12132,#2216,.T.);
#15191=EDGE_CURVE('',#12135,#12134,#7244,.T.);
#15192=EDGE_CURVE('',#12133,#12135,#2217,.T.);
#15193=EDGE_CURVE('',#12126,#12085,#7245,.T.);
#15194=EDGE_CURVE('',#12129,#12121,#7246,.T.);
#15195=EDGE_CURVE('',#12081,#12136,#7247,.T.);
#15196=EDGE_CURVE('',#12136,#12040,#7248,.T.);
#15197=EDGE_CURVE('',#12136,#12030,#7249,.T.);
#15198=EDGE_CURVE('',#12137,#12052,#7250,.T.);
#15199=EDGE_CURVE('',#12138,#12137,#7251,.T.);
#15200=EDGE_CURVE('',#12139,#12138,#7252,.T.);
#15201=EDGE_CURVE('',#12140,#12139,#7253,.T.);
#15202=EDGE_CURVE('',#12141,#12140,#7254,.T.);
#15203=EDGE_CURVE('',#12142,#12141,#7255,.T.);
#15204=EDGE_CURVE('',#12113,#12142,#7256,.T.);
#15205=EDGE_CURVE('',#12098,#12131,#7257,.T.);
#15206=EDGE_CURVE('',#12130,#12097,#7258,.T.);
#15207=EDGE_CURVE('',#12143,#12144,#7259,.T.);
#15208=EDGE_CURVE('',#12141,#12143,#7260,.T.);
#15209=EDGE_CURVE('',#12144,#12141,#7261,.T.);
#15210=EDGE_CURVE('',#12143,#12145,#7262,.T.);
#15211=EDGE_CURVE('',#12145,#12142,#7263,.T.);
#15212=EDGE_CURVE('',#12146,#12147,#7264,.T.);
#15213=EDGE_CURVE('',#12147,#12144,#7265,.T.);
#15214=EDGE_CURVE('',#12140,#12146,#7266,.T.);
#15215=EDGE_CURVE('',#12101,#12143,#7267,.T.);
#15216=EDGE_CURVE('',#12144,#12148,#7268,.T.);
#15217=EDGE_CURVE('',#12148,#12102,#7269,.T.);
#15218=EDGE_CURVE('',#12145,#12111,#7270,.T.);
#15219=EDGE_CURVE('',#12148,#12149,#7271,.T.);
#15220=EDGE_CURVE('',#12149,#12150,#7272,.T.);
#15221=EDGE_CURVE('',#12150,#12091,#7273,.T.);
#15222=EDGE_CURVE('',#12068,#12145,#7274,.T.);
#15223=EDGE_CURVE('',#12151,#12150,#7275,.T.);
#15224=EDGE_CURVE('',#12151,#12152,#7276,.T.);
#15225=EDGE_CURVE('',#12153,#12152,#7277,.T.);
#15226=EDGE_CURVE('',#12092,#12153,#7278,.T.);
#15227=EDGE_CURVE('',#12067,#12138,#7279,.F.);
#15228=EDGE_CURVE('',#12137,#12066,#7280,.T.);
#15229=EDGE_CURVE('',#12153,#12154,#7281,.T.);
#15230=EDGE_CURVE('',#12154,#12065,#7282,.T.);
#15231=EDGE_CURVE('',#12155,#12154,#7283,.T.);
#15232=EDGE_CURVE('',#12067,#12155,#7284,.T.);
#15233=EDGE_CURVE('',#12156,#12157,#7285,.T.);
#15234=EDGE_CURVE('',#12158,#12156,#2218,.T.);
#15235=EDGE_CURVE('',#12159,#12158,#7286,.T.);
#15236=EDGE_CURVE('',#12157,#12159,#2219,.T.);
#15237=EDGE_CURVE('',#12152,#12160,#7287,.T.);
#15238=EDGE_CURVE('',#12160,#12161,#7288,.T.);
#15239=EDGE_CURVE('',#12155,#12161,#7289,.T.);
#15240=EDGE_CURVE('',#12161,#12139,#7290,.T.);
#15241=EDGE_CURVE('',#12160,#12162,#7291,.T.);
#15242=EDGE_CURVE('',#12146,#12162,#7292,.T.);
#15243=EDGE_CURVE('',#12162,#12151,#7293,.T.);
#15244=EDGE_CURVE('',#12149,#12147,#7294,.T.);
#15245=EDGE_CURVE('',#12163,#12164,#7295,.T.);
#15246=EDGE_CURVE('',#12165,#12163,#2220,.T.);
#15247=EDGE_CURVE('',#12166,#12165,#7296,.T.);
#15248=EDGE_CURVE('',#12164,#12166,#2221,.T.);
#15249=EDGE_CURVE('',#12167,#12132,#7297,.T.);
#15250=EDGE_CURVE('',#12133,#12168,#7298,.T.);
#15251=EDGE_CURVE('',#12168,#12167,#7299,.T.);
#15252=EDGE_CURVE('',#12169,#12134,#7300,.T.);
#15253=EDGE_CURVE('',#12167,#12169,#2222,.T.);
#15254=EDGE_CURVE('',#12170,#12135,#7301,.T.);
#15255=EDGE_CURVE('',#12169,#12170,#7302,.T.);
#15256=EDGE_CURVE('',#12170,#12168,#2223,.T.);
#15257=EDGE_CURVE('',#12171,#12167,#7303,.T.);
#15258=EDGE_CURVE('',#12172,#12171,#2224,.T.);
#15259=EDGE_CURVE('',#12172,#12169,#7304,.T.);
#15260=EDGE_CURVE('',#12173,#12168,#7305,.T.);
#15261=EDGE_CURVE('',#12171,#12173,#7306,.T.);
#15262=EDGE_CURVE('',#12173,#12117,#7307,.T.);
#15263=EDGE_CURVE('',#12118,#12171,#7308,.T.);
#15264=EDGE_CURVE('',#12174,#12119,#7309,.T.);
#15265=EDGE_CURVE('',#12173,#12174,#2225,.T.);
#15266=EDGE_CURVE('',#12172,#12120,#7310,.T.);
#15267=EDGE_CURVE('',#12174,#12172,#7311,.T.);
#15268=EDGE_CURVE('',#12174,#12170,#7312,.T.);
#15269=EDGE_CURVE('',#12175,#12156,#7313,.T.);
#15270=EDGE_CURVE('',#12157,#12176,#7314,.T.);
#15271=EDGE_CURVE('',#12176,#12175,#7315,.T.);
#15272=EDGE_CURVE('',#12177,#12158,#7316,.T.);
#15273=EDGE_CURVE('',#12175,#12177,#2226,.T.);
#15274=EDGE_CURVE('',#12178,#12159,#7317,.T.);
#15275=EDGE_CURVE('',#12177,#12178,#7318,.T.);
#15276=EDGE_CURVE('',#12178,#12176,#2227,.T.);
#15277=EDGE_CURVE('',#12179,#12175,#7319,.T.);
#15278=EDGE_CURVE('',#12180,#12179,#2228,.T.);
#15279=EDGE_CURVE('',#12180,#12177,#7320,.T.);
#15280=EDGE_CURVE('',#12181,#12176,#7321,.T.);
#15281=EDGE_CURVE('',#12179,#12181,#7322,.T.);
#15282=EDGE_CURVE('',#12181,#12163,#7323,.T.);
#15283=EDGE_CURVE('',#12164,#12179,#7324,.T.);
#15284=EDGE_CURVE('',#12182,#12165,#7325,.T.);
#15285=EDGE_CURVE('',#12181,#12182,#2229,.T.);
#15286=EDGE_CURVE('',#12180,#12166,#7326,.T.);
#15287=EDGE_CURVE('',#12182,#12180,#7327,.T.);
#15288=EDGE_CURVE('',#12182,#12178,#7328,.T.);
#15289=EDGE_CURVE('',#12183,#12184,#7329,.T.);
#15290=EDGE_CURVE('',#12184,#12185,#7330,.T.);
#15291=EDGE_CURVE('',#12185,#12186,#7331,.T.);
#15292=EDGE_CURVE('',#12186,#12187,#7332,.T.);
#15293=EDGE_CURVE('',#12187,#12188,#7333,.T.);
#15294=EDGE_CURVE('',#12188,#12183,#7334,.T.);
#15295=EDGE_CURVE('',#12185,#12189,#7335,.T.);
#15296=EDGE_CURVE('',#12190,#12189,#7336,.T.);
#15297=EDGE_CURVE('',#12190,#12191,#7337,.T.);
#15298=EDGE_CURVE('',#12191,#12192,#7338,.T.);
#15299=EDGE_CURVE('',#12192,#12186,#7339,.T.);
#15300=EDGE_CURVE('',#12193,#12184,#7340,.T.);
#15301=EDGE_CURVE('',#12189,#12193,#7341,.T.);
#15302=EDGE_CURVE('',#12194,#12183,#7342,.T.);
#15303=EDGE_CURVE('',#12194,#12195,#7343,.T.);
#15304=EDGE_CURVE('',#12195,#12196,#7344,.T.);
#15305=EDGE_CURVE('',#12193,#12196,#7345,.T.);
#15306=EDGE_CURVE('',#12196,#12197,#7346,.T.);
#15307=EDGE_CURVE('',#12197,#12198,#7347,.T.);
#15308=EDGE_CURVE('',#12198,#12190,#7348,.T.);
#15309=EDGE_CURVE('',#12199,#12200,#7349,.T.);
#15310=EDGE_CURVE('',#12200,#12201,#7350,.T.);
#15311=EDGE_CURVE('',#12201,#12202,#7351,.T.);
#15312=EDGE_CURVE('',#12202,#12203,#7352,.T.);
#15313=EDGE_CURVE('',#12203,#12204,#7353,.T.);
#15314=EDGE_CURVE('',#12204,#12199,#7354,.T.);
#15315=EDGE_CURVE('',#12205,#12202,#7355,.T.);
#15316=EDGE_CURVE('',#12205,#12206,#7356,.T.);
#15317=EDGE_CURVE('',#12206,#12207,#7357,.T.);
#15318=EDGE_CURVE('',#12208,#12207,#7358,.T.);
#15319=EDGE_CURVE('',#12208,#12203,#7359,.T.);
#15320=EDGE_CURVE('',#12201,#12209,#7360,.T.);
#15321=EDGE_CURVE('',#12210,#12209,#7361,.T.);
#15322=EDGE_CURVE('',#12210,#12205,#7362,.T.);
#15323=EDGE_CURVE('',#12211,#12200,#7363,.T.);
#15324=EDGE_CURVE('',#12209,#12211,#7364,.T.);
#15325=EDGE_CURVE('',#12212,#12212,#2230,.T.);
#15326=EDGE_CURVE('',#12213,#12213,#2231,.T.);
#15327=EDGE_CURVE('',#12214,#12215,#7365,.T.);
#15328=EDGE_CURVE('',#12215,#12216,#7366,.T.);
#15329=EDGE_CURVE('',#12216,#12217,#7367,.T.);
#15330=EDGE_CURVE('',#12217,#12218,#7368,.T.);
#15331=EDGE_CURVE('',#12218,#12219,#7369,.T.);
#15332=EDGE_CURVE('',#12219,#12214,#7370,.T.);
#15333=EDGE_CURVE('',#12216,#12220,#7371,.T.);
#15334=EDGE_CURVE('',#12207,#12220,#7372,.T.);
#15335=EDGE_CURVE('',#12206,#12221,#7373,.T.);
#15336=EDGE_CURVE('',#12221,#12217,#7374,.T.);
#15337=EDGE_CURVE('',#12222,#12215,#7375,.T.);
#15338=EDGE_CURVE('',#12220,#12222,#7376,.T.);
#15339=EDGE_CURVE('',#12223,#12223,#2232,.T.);
#15340=EDGE_CURVE('',#12224,#12224,#2233,.T.);
#15341=EDGE_CURVE('',#12225,#12214,#7377,.T.);
#15342=EDGE_CURVE('',#12225,#12226,#7378,.T.);
#15343=EDGE_CURVE('',#12226,#12227,#7379,.T.);
#15344=EDGE_CURVE('',#12222,#12227,#7380,.T.);
#15345=EDGE_CURVE('',#12227,#12228,#7381,.T.);
#15346=EDGE_CURVE('',#12228,#12208,#7382,.T.);
#15347=EDGE_CURVE('',#12204,#12228,#7383,.T.);
#15348=EDGE_CURVE('',#12226,#12229,#7384,.T.);
#15349=EDGE_CURVE('',#12229,#12199,#7385,.T.);
#15350=EDGE_CURVE('',#12212,#12230,#7386,.T.);
#15351=EDGE_CURVE('',#12230,#12230,#2234,.T.);
#15352=EDGE_CURVE('',#12231,#12231,#2235,.T.);
#15353=EDGE_CURVE('',#12231,#12230,#7387,.T.);
#15354=EDGE_CURVE('',#12224,#12231,#7388,.T.);
#15355=EDGE_CURVE('',#12213,#12232,#7389,.T.);
#15356=EDGE_CURVE('',#12232,#12232,#2236,.T.);
#15357=EDGE_CURVE('',#12233,#12233,#2237,.T.);
#15358=EDGE_CURVE('',#12233,#12232,#7390,.T.);
#15359=EDGE_CURVE('',#12223,#12233,#7391,.T.);
#15360=EDGE_CURVE('',#12229,#12234,#7392,.T.);
#15361=EDGE_CURVE('',#12234,#12211,#7393,.T.);
#15362=EDGE_CURVE('',#12188,#12211,#7394,.T.);
#15363=EDGE_CURVE('',#12234,#12194,#7395,.T.);
#15364=EDGE_CURVE('',#12195,#12225,#7396,.T.);
#15365=EDGE_CURVE('',#12219,#12197,#7397,.T.);
#15366=EDGE_CURVE('',#12198,#12218,#7398,.T.);
#15367=EDGE_CURVE('',#12221,#12191,#7399,.T.);
#15368=EDGE_CURVE('',#12192,#12210,#7400,.T.);
#15369=EDGE_CURVE('',#12209,#12187,#7401,.T.);
#15370=EDGE_CURVE('',#12235,#12236,#7402,.T.);
#15371=EDGE_CURVE('',#12236,#12237,#2238,.T.);
#15372=EDGE_CURVE('',#12237,#12238,#7403,.T.);
#15373=EDGE_CURVE('',#12238,#12235,#2239,.T.);
#15374=EDGE_CURVE('',#12239,#12240,#7404,.T.);
#15375=EDGE_CURVE('',#12240,#12236,#7405,.T.);
#15376=EDGE_CURVE('',#12235,#12239,#7406,.T.);
#15377=EDGE_CURVE('',#12241,#12242,#7407,.T.);
#15378=EDGE_CURVE('',#12242,#12240,#2240,.T.);
#15379=EDGE_CURVE('',#12239,#12241,#2241,.T.);
#15380=EDGE_CURVE('',#12243,#12244,#7408,.T.);
#15381=EDGE_CURVE('',#12244,#12242,#7409,.T.);
#15382=EDGE_CURVE('',#12241,#12243,#7410,.T.);
#15383=EDGE_CURVE('',#12245,#12246,#7411,.T.);
#15384=EDGE_CURVE('',#12246,#12244,#2242,.T.);
#15385=EDGE_CURVE('',#12243,#12245,#2243,.T.);
#15386=EDGE_CURVE('',#12247,#12248,#7412,.T.);
#15387=EDGE_CURVE('',#12248,#12246,#7413,.T.);
#15388=EDGE_CURVE('',#12245,#12247,#7414,.T.);
#15389=EDGE_CURVE('',#12249,#12250,#7415,.T.);
#15390=EDGE_CURVE('',#12250,#12248,#2244,.T.);
#15391=EDGE_CURVE('',#12247,#12249,#2245,.T.);
#15392=EDGE_CURVE('',#12237,#12250,#7416,.T.);
#15393=EDGE_CURVE('',#12249,#12238,#7417,.T.);
#15394=EDGE_CURVE('',#12248,#12251,#7418,.T.);
#15395=EDGE_CURVE('',#12252,#12251,#7419,.T.);
#15396=EDGE_CURVE('',#12246,#12252,#7420,.T.);
#15397=EDGE_CURVE('',#12250,#12253,#7421,.T.);
#15398=EDGE_CURVE('',#12251,#12253,#2246,.T.);
#15399=EDGE_CURVE('',#12254,#12237,#7422,.T.);
#15400=EDGE_CURVE('',#12253,#12254,#7423,.T.);
#15401=EDGE_CURVE('',#12236,#12255,#7424,.T.);
#15402=EDGE_CURVE('',#12254,#12255,#2247,.T.);
#15403=EDGE_CURVE('',#12256,#12256,#2248,.T.);
#15404=EDGE_CURVE('',#12257,#12257,#2249,.T.);
#15405=EDGE_CURVE('',#12258,#12258,#2250,.T.);
#15406=EDGE_CURVE('',#12259,#12260,#7425,.F.);
#15407=EDGE_CURVE('',#12260,#12261,#7426,.T.);
#15408=EDGE_CURVE('',#12261,#12262,#7427,.F.);
#15409=EDGE_CURVE('',#12262,#12259,#7428,.T.);
#15410=EDGE_CURVE('',#12260,#12263,#2251,.T.);
#15411=EDGE_CURVE('',#12264,#12263,#7429,.T.);
#15412=EDGE_CURVE('',#12261,#12264,#2252,.T.);
#15413=EDGE_CURVE('',#12265,#12264,#7430,.F.);
#15414=EDGE_CURVE('',#12263,#12266,#7431,.F.);
#15415=EDGE_CURVE('',#12266,#12265,#7432,.T.);
#15416=EDGE_CURVE('',#12267,#12253,#7433,.T.);
#15417=EDGE_CURVE('',#12254,#12268,#7434,.T.);
#15418=EDGE_CURVE('',#12268,#12267,#7435,.T.);
#15419=EDGE_CURVE('',#12269,#12251,#7436,.T.);
#15420=EDGE_CURVE('',#12267,#12269,#2253,.T.);
#15421=EDGE_CURVE('',#12270,#12252,#7437,.T.);
#15422=EDGE_CURVE('',#12269,#12270,#7438,.T.);
#15423=EDGE_CURVE('',#12271,#12272,#7439,.T.);
#15424=EDGE_CURVE('',#12272,#12252,#2254,.T.);
#15425=EDGE_CURVE('',#12270,#12271,#2255,.T.);
#15426=EDGE_CURVE('',#12273,#12274,#7440,.T.);
#15427=EDGE_CURVE('',#12274,#12272,#7441,.T.);
#15428=EDGE_CURVE('',#12271,#12273,#7442,.T.);
#15429=EDGE_CURVE('',#12275,#12276,#7443,.T.);
#15430=EDGE_CURVE('',#12276,#12274,#2256,.T.);
#15431=EDGE_CURVE('',#12273,#12275,#2257,.T.);
#15432=EDGE_CURVE('',#12277,#12255,#7444,.T.);
#15433=EDGE_CURVE('',#12255,#12276,#7445,.T.);
#15434=EDGE_CURVE('',#12275,#12277,#7446,.T.);
#15435=EDGE_CURVE('',#12277,#12268,#2258,.T.);
#15436=EDGE_CURVE('',#12270,#12278,#7447,.T.);
#15437=EDGE_CURVE('',#12279,#12278,#2259,.T.);
#15438=EDGE_CURVE('',#12279,#12271,#7448,.T.);
#15439=EDGE_CURVE('',#12280,#12269,#7449,.T.);
#15440=EDGE_CURVE('',#12278,#12280,#7450,.T.);
#15441=EDGE_CURVE('',#12267,#12281,#7451,.T.);
#15442=EDGE_CURVE('',#12280,#12281,#2260,.T.);
#15443=EDGE_CURVE('',#12282,#12268,#7452,.T.);
#15444=EDGE_CURVE('',#12281,#12282,#7453,.T.);
#15445=EDGE_CURVE('',#12283,#12283,#2261,.T.);
#15446=EDGE_CURVE('',#12242,#12274,#7454,.T.);
#15447=EDGE_CURVE('',#12240,#12276,#7455,.T.);
#15448=EDGE_CURVE('',#12284,#12285,#7456,.T.);
#15449=EDGE_CURVE('',#12285,#12286,#7457,.T.);
#15450=EDGE_CURVE('',#12286,#12287,#7458,.T.);
#15451=EDGE_CURVE('',#12287,#12284,#7459,.T.);
#15452=EDGE_CURVE('',#12288,#12289,#7460,.T.);
#15453=EDGE_CURVE('',#12289,#12287,#2262,.T.);
#15454=EDGE_CURVE('',#12286,#12288,#2263,.T.);
#15455=EDGE_CURVE('',#12290,#12291,#7461,.T.);
#15456=EDGE_CURVE('',#12291,#12289,#7462,.T.);
#15457=EDGE_CURVE('',#12288,#12290,#7463,.T.);
#15458=EDGE_CURVE('',#12292,#12293,#7464,.T.);
#15459=EDGE_CURVE('',#12293,#12291,#2264,.T.);
#15460=EDGE_CURVE('',#12290,#12292,#2265,.T.);
#15461=EDGE_CURVE('',#12294,#12295,#7465,.T.);
#15462=EDGE_CURVE('',#12295,#12293,#7466,.T.);
#15463=EDGE_CURVE('',#12292,#12294,#7467,.T.);
#15464=EDGE_CURVE('',#12296,#12294,#7468,.T.);
#15465=EDGE_CURVE('',#12297,#12296,#2266,.T.);
#15466=EDGE_CURVE('',#12295,#12297,#7469,.T.);
#15467=EDGE_CURVE('',#12285,#12298,#7470,.T.);
#15468=EDGE_CURVE('',#12296,#12298,#7471,.T.);
#15469=EDGE_CURVE('',#12299,#12300,#7472,.F.);
#15470=EDGE_CURVE('',#12300,#12301,#7473,.T.);
#15471=EDGE_CURVE('',#12301,#12302,#7474,.T.);
#15472=EDGE_CURVE('',#12302,#12299,#7475,.T.);
#15473=EDGE_CURVE('',#12303,#12304,#7476,.T.);
#15474=EDGE_CURVE('',#12304,#12302,#2267,.T.);
#15475=EDGE_CURVE('',#12301,#12303,#2268,.T.);
#15476=EDGE_CURVE('',#12305,#12306,#7477,.T.);
#15477=EDGE_CURVE('',#12306,#12304,#7478,.T.);
#15478=EDGE_CURVE('',#12303,#12305,#7479,.T.);
#15479=EDGE_CURVE('',#12307,#12308,#7480,.T.);
#15480=EDGE_CURVE('',#12308,#12306,#2269,.T.);
#15481=EDGE_CURVE('',#12305,#12307,#2270,.T.);
#15482=EDGE_CURVE('',#12309,#12310,#7481,.F.);
#15483=EDGE_CURVE('',#12310,#12308,#7482,.T.);
#15484=EDGE_CURVE('',#12307,#12309,#7483,.T.);
#15485=EDGE_CURVE('',#12309,#12300,#7484,.T.);
#15486=EDGE_CURVE('',#12311,#12311,#2271,.T.);
#15487=EDGE_CURVE('',#12312,#12313,#7485,.F.);
#15488=EDGE_CURVE('',#12313,#12314,#7486,.T.);
#15489=EDGE_CURVE('',#12314,#12315,#7487,.T.);
#15490=EDGE_CURVE('',#12315,#12312,#7488,.T.);
#15491=EDGE_CURVE('',#12316,#12317,#7489,.T.);
#15492=EDGE_CURVE('',#12317,#12315,#2272,.T.);
#15493=EDGE_CURVE('',#12314,#12316,#2273,.T.);
#15494=EDGE_CURVE('',#12318,#12319,#7490,.T.);
#15495=EDGE_CURVE('',#12319,#12317,#7491,.T.);
#15496=EDGE_CURVE('',#12316,#12318,#7492,.T.);
#15497=EDGE_CURVE('',#12320,#12321,#7493,.T.);
#15498=EDGE_CURVE('',#12321,#12319,#2274,.T.);
#15499=EDGE_CURVE('',#12318,#12320,#2275,.T.);
#15500=EDGE_CURVE('',#12322,#12323,#7494,.F.);
#15501=EDGE_CURVE('',#12323,#12321,#7495,.T.);
#15502=EDGE_CURVE('',#12320,#12322,#7496,.T.);
#15503=EDGE_CURVE('',#12322,#12313,#7497,.T.);
#15504=EDGE_CURVE('',#12324,#12324,#2276,.T.);
#15505=EDGE_CURVE('',#12325,#12326,#7498,.T.);
#15506=EDGE_CURVE('',#12326,#12327,#7499,.T.);
#15507=EDGE_CURVE('',#12327,#12328,#7500,.T.);
#15508=EDGE_CURVE('',#12328,#12325,#7501,.T.);
#15509=EDGE_CURVE('',#12329,#12330,#7502,.T.);
#15510=EDGE_CURVE('',#12330,#12328,#2277,.T.);
#15511=EDGE_CURVE('',#12327,#12329,#2278,.T.);
#15512=EDGE_CURVE('',#12331,#12332,#7503,.T.);
#15513=EDGE_CURVE('',#12332,#12330,#7504,.T.);
#15514=EDGE_CURVE('',#12329,#12331,#7505,.T.);
#15515=EDGE_CURVE('',#12333,#12334,#7506,.T.);
#15516=EDGE_CURVE('',#12334,#12332,#2279,.T.);
#15517=EDGE_CURVE('',#12331,#12333,#2280,.T.);
#15518=EDGE_CURVE('',#12335,#12336,#7507,.T.);
#15519=EDGE_CURVE('',#12336,#12334,#7508,.T.);
#15520=EDGE_CURVE('',#12333,#12335,#7509,.T.);
#15521=EDGE_CURVE('',#12337,#12323,#7510,.T.);
#15522=EDGE_CURVE('',#12337,#12325,#7511,.T.);
#15523=EDGE_CURVE('',#12321,#12328,#7512,.T.);
#15524=EDGE_CURVE('',#12330,#12319,#7513,.T.);
#15525=EDGE_CURVE('',#12317,#12332,#7514,.T.);
#15526=EDGE_CURVE('',#12334,#12315,#7515,.T.);
#15527=EDGE_CURVE('',#12336,#12338,#7516,.T.);
#15528=EDGE_CURVE('',#12312,#12338,#7517,.T.);
#15529=EDGE_CURVE('',#12339,#12335,#7518,.T.);
#15530=EDGE_CURVE('',#12338,#12339,#2281,.T.);
#15531=EDGE_CURVE('',#12340,#12340,#2282,.T.);
#15532=EDGE_CURVE('',#12340,#12341,#7519,.T.);
#15533=EDGE_CURVE('',#12341,#12341,#2283,.T.);
#15534=EDGE_CURVE('',#12342,#12342,#2284,.T.);
#15535=EDGE_CURVE('',#12341,#12258,#7520,.T.);
#15536=EDGE_CURVE('',#12342,#12343,#7521,.T.);
#15537=EDGE_CURVE('',#12343,#12343,#2285,.T.);
#15538=EDGE_CURVE('',#12344,#12344,#2286,.T.);
#15539=EDGE_CURVE('',#12344,#12343,#7522,.T.);
#15540=EDGE_CURVE('',#12283,#12345,#7523,.T.);
#15541=EDGE_CURVE('',#12345,#12345,#2287,.T.);
#15542=EDGE_CURVE('',#12345,#12346,#7524,.T.);
#15543=EDGE_CURVE('',#12346,#12346,#2288,.T.);
#15544=EDGE_CURVE('',#12346,#12347,#7525,.T.);
#15545=EDGE_CURVE('',#12348,#12344,#7526,.T.);
#15546=EDGE_CURVE('',#12311,#12324,#7527,.T.);
#15547=EDGE_CURVE('',#12293,#12302,#7528,.T.);
#15548=EDGE_CURVE('',#12304,#12291,#7529,.T.);
#15549=EDGE_CURVE('',#12289,#12306,#7530,.T.);
#15550=EDGE_CURVE('',#12308,#12287,#7531,.T.);
#15551=EDGE_CURVE('',#12349,#12284,#7532,.T.);
#15552=EDGE_CURVE('',#12298,#12349,#2289,.T.);
#15553=EDGE_CURVE('',#12349,#12310,#7533,.T.);
#15554=EDGE_CURVE('',#12299,#12297,#7534,.T.);
#15555=EDGE_CURVE('',#12296,#12298,#2290,.T.);
#15556=EDGE_CURVE('',#12350,#12337,#2291,.T.);
#15557=EDGE_CURVE('',#12326,#12350,#7535,.T.);
#15558=EDGE_CURVE('',#12339,#12350,#7536,.T.);
#15559=EDGE_CURVE('',#12339,#12350,#2292,.T.);
#15560=EDGE_CURVE('',#12351,#12297,#2293,.T.);
#15561=EDGE_CURVE('',#12337,#12351,#2294,.T.);
#15562=EDGE_CURVE('',#12349,#12338,#2295,.T.);
#15563=EDGE_CURVE('',#12351,#12352,#7537,.T.);
#15564=EDGE_CURVE('',#12352,#12352,#2296,.T.);
#15565=EDGE_CURVE('',#12352,#12257,#7538,.T.);
#15566=EDGE_CURVE('',#12353,#12353,#2297,.T.);
#15567=EDGE_CURVE('',#12353,#12354,#7539,.T.);
#15568=EDGE_CURVE('',#12354,#12354,#2298,.T.);
#15569=EDGE_CURVE('',#12355,#12355,#2299,.T.);
#15570=EDGE_CURVE('',#12355,#12354,#7540,.T.);
#15571=EDGE_CURVE('',#12356,#12356,#2300,.T.);
#15572=EDGE_CURVE('',#12266,#12259,#2301,.T.);
#15573=EDGE_CURVE('',#12262,#12265,#2302,.T.);
#15574=EDGE_CURVE('',#12357,#12358,#2303,.T.);
#15575=EDGE_CURVE('',#12358,#12256,#2304,.T.);
#15576=EDGE_CURVE('',#12358,#12357,#2305,.T.);
#15577=EDGE_CURVE('',#12359,#12359,#2306,.T.);
#15578=EDGE_CURVE('',#12359,#12357,#7541,.T.);
#15579=EDGE_CURVE('',#12360,#12360,#2307,.T.);
#15580=EDGE_CURVE('',#12361,#12361,#2308,.T.);
#15581=EDGE_CURVE('',#12361,#12360,#7542,.T.);
#15582=EDGE_CURVE('',#12362,#12362,#2309,.T.);
#15583=EDGE_CURVE('',#12362,#12361,#7543,.T.);
#15584=EDGE_CURVE('',#12356,#12362,#7544,.T.);
#15585=EDGE_CURVE('',#12363,#12278,#7545,.T.);
#15586=EDGE_CURVE('',#12280,#12364,#7546,.T.);
#15587=EDGE_CURVE('',#12364,#12363,#7547,.T.);
#15588=EDGE_CURVE('',#12365,#12279,#7548,.T.);
#15589=EDGE_CURVE('',#12363,#12365,#2310,.T.);
#15590=EDGE_CURVE('',#12366,#12367,#7549,.T.);
#15591=EDGE_CURVE('',#12367,#12279,#7550,.T.);
#15592=EDGE_CURVE('',#12365,#12366,#7551,.T.);
#15593=EDGE_CURVE('',#12368,#12369,#7552,.T.);
#15594=EDGE_CURVE('',#12369,#12367,#2311,.T.);
#15595=EDGE_CURVE('',#12366,#12368,#2312,.T.);
#15596=EDGE_CURVE('',#12370,#12371,#7553,.T.);
#15597=EDGE_CURVE('',#12371,#12369,#7554,.T.);
#15598=EDGE_CURVE('',#12368,#12370,#7555,.T.);
#15599=EDGE_CURVE('',#12372,#12282,#7556,.T.);
#15600=EDGE_CURVE('',#12282,#12371,#2313,.T.);
#15601=EDGE_CURVE('',#12370,#12372,#2314,.T.);
#15602=EDGE_CURVE('',#12373,#12281,#7557,.T.);
#15603=EDGE_CURVE('',#12372,#12373,#7558,.T.);
#15604=EDGE_CURVE('',#12373,#12364,#2315,.T.);
#15605=EDGE_CURVE('',#12277,#12371,#7559,.T.);
#15606=EDGE_CURVE('',#12244,#12272,#7560,.T.);
#15607=EDGE_CURVE('',#12369,#12275,#7561,.T.);
#15608=EDGE_CURVE('',#12273,#12367,#7562,.T.);
#15609=EDGE_CURVE('',#12374,#12375,#7563,.T.);
#15610=EDGE_CURVE('',#12374,#12376,#785,.T.);
#15611=EDGE_CURVE('',#12376,#12377,#2316,.F.);
#15612=EDGE_CURVE('',#12377,#12375,#786,.T.);
#15613=EDGE_CURVE('',#12378,#12379,#7564,.T.);
#15614=EDGE_CURVE('',#12378,#12374,#787,.T.);
#15615=EDGE_CURVE('',#12375,#12379,#788,.T.);
#15616=EDGE_CURVE('',#12380,#12381,#7565,.T.);
#15617=EDGE_CURVE('',#12380,#12378,#789,.T.);
#15618=EDGE_CURVE('',#12379,#12381,#790,.T.);
#15619=EDGE_CURVE('',#12382,#12383,#7566,.T.);
#15620=EDGE_CURVE('',#12382,#12380,#791,.T.);
#15621=EDGE_CURVE('',#12381,#12383,#792,.T.);
#15622=EDGE_CURVE('',#12384,#12385,#7567,.T.);
#15623=EDGE_CURVE('',#12386,#12384,#2317,.T.);
#15624=EDGE_CURVE('',#12386,#12382,#793,.T.);
#15625=EDGE_CURVE('',#12383,#12385,#794,.T.);
#15626=EDGE_CURVE('',#12387,#12388,#7568,.T.);
#15627=EDGE_CURVE('',#12387,#12389,#795,.T.);
#15628=EDGE_CURVE('',#12390,#12389,#2318,.T.);
#15629=EDGE_CURVE('',#12388,#12390,#796,.T.);
#15630=EDGE_CURVE('',#12391,#12392,#7569,.T.);
#15631=EDGE_CURVE('',#12391,#12387,#797,.T.);
#15632=EDGE_CURVE('',#12392,#12388,#798,.T.);
#15633=EDGE_CURVE('',#12393,#12394,#7570,.T.);
#15634=EDGE_CURVE('',#12393,#12391,#799,.T.);
#15635=EDGE_CURVE('',#12394,#12392,#800,.T.);
#15636=EDGE_CURVE('',#12395,#12396,#7571,.T.);
#15637=EDGE_CURVE('',#12395,#12393,#801,.T.);
#15638=EDGE_CURVE('',#12396,#12394,#802,.T.);
#15639=EDGE_CURVE('',#12397,#12398,#7572,.T.);
#15640=EDGE_CURVE('',#12397,#12399,#7573,.T.);
#15641=EDGE_CURVE('',#12400,#12399,#7574,.T.);
#15642=EDGE_CURVE('',#12398,#12400,#271,.T.);
#15643=EDGE_CURVE('',#12400,#12401,#272,.T.);
#15644=EDGE_CURVE('',#12399,#12402,#7575,.T.);
#15645=EDGE_CURVE('',#12401,#12402,#7576,.T.);
#15646=EDGE_CURVE('',#12397,#12402,#2319,.T.);
#15647=EDGE_CURVE('',#12403,#12404,#7577,.T.);
#15648=EDGE_CURVE('',#12403,#12405,#7578,.T.);
#15649=EDGE_CURVE('',#12406,#12405,#7579,.T.);
#15650=EDGE_CURVE('',#12404,#12406,#273,.T.);
#15651=EDGE_CURVE('',#12406,#12407,#274,.T.);
#15652=EDGE_CURVE('',#12405,#12408,#7580,.T.);
#15653=EDGE_CURVE('',#12407,#12408,#7581,.T.);
#15654=EDGE_CURVE('',#12403,#12408,#2320,.T.);
#15655=EDGE_CURVE('',#12409,#12410,#7582,.T.);
#15656=EDGE_CURVE('',#12409,#12411,#7583,.T.);
#15657=EDGE_CURVE('',#12412,#12411,#7584,.T.);
#15658=EDGE_CURVE('',#12410,#12412,#275,.T.);
#15659=EDGE_CURVE('',#12412,#12413,#276,.T.);
#15660=EDGE_CURVE('',#12411,#12414,#7585,.T.);
#15661=EDGE_CURVE('',#12413,#12414,#7586,.T.);
#15662=EDGE_CURVE('',#12409,#12414,#2321,.T.);
#15663=EDGE_CURVE('',#12415,#12416,#7587,.T.);
#15664=EDGE_CURVE('',#12415,#12417,#7588,.T.);
#15665=EDGE_CURVE('',#12418,#12417,#7589,.T.);
#15666=EDGE_CURVE('',#12416,#12418,#277,.T.);
#15667=EDGE_CURVE('',#12418,#12419,#278,.T.);
#15668=EDGE_CURVE('',#12417,#12420,#7590,.T.);
#15669=EDGE_CURVE('',#12419,#12420,#7591,.T.);
#15670=EDGE_CURVE('',#12415,#12420,#2322,.T.);
#15671=EDGE_CURVE('',#12421,#12422,#7592,.T.);
#15672=EDGE_CURVE('',#12421,#12423,#7593,.T.);
#15673=EDGE_CURVE('',#12424,#12423,#7594,.T.);
#15674=EDGE_CURVE('',#12422,#12424,#279,.T.);
#15675=EDGE_CURVE('',#12424,#12425,#280,.T.);
#15676=EDGE_CURVE('',#12423,#12426,#7595,.T.);
#15677=EDGE_CURVE('',#12425,#12426,#7596,.T.);
#15678=EDGE_CURVE('',#12421,#12426,#2323,.T.);
#15679=EDGE_CURVE('',#12427,#12428,#7597,.T.);
#15680=EDGE_CURVE('',#12427,#12429,#7598,.T.);
#15681=EDGE_CURVE('',#12430,#12429,#7599,.T.);
#15682=EDGE_CURVE('',#12428,#12430,#281,.T.);
#15683=EDGE_CURVE('',#12430,#12431,#282,.T.);
#15684=EDGE_CURVE('',#12429,#12432,#7600,.T.);
#15685=EDGE_CURVE('',#12431,#12432,#7601,.T.);
#15686=EDGE_CURVE('',#12427,#12433,#2324,.T.);
#15687=EDGE_CURVE('',#12433,#12432,#2325,.T.);
#15688=EDGE_CURVE('',#12434,#12435,#7602,.T.);
#15689=EDGE_CURVE('',#12434,#12436,#7603,.T.);
#15690=EDGE_CURVE('',#12437,#12436,#7604,.T.);
#15691=EDGE_CURVE('',#12435,#12437,#283,.T.);
#15692=EDGE_CURVE('',#12437,#12438,#284,.T.);
#15693=EDGE_CURVE('',#12436,#12439,#7605,.T.);
#15694=EDGE_CURVE('',#12438,#12439,#7606,.T.);
#15695=EDGE_CURVE('',#12434,#12439,#2326,.T.);
#15696=EDGE_CURVE('',#12440,#12441,#7607,.T.);
#15697=EDGE_CURVE('',#12440,#12442,#7608,.T.);
#15698=EDGE_CURVE('',#12443,#12442,#7609,.T.);
#15699=EDGE_CURVE('',#12441,#12443,#285,.T.);
#15700=EDGE_CURVE('',#12443,#12444,#286,.T.);
#15701=EDGE_CURVE('',#12442,#12445,#7610,.T.);
#15702=EDGE_CURVE('',#12444,#12445,#7611,.T.);
#15703=EDGE_CURVE('',#12440,#12445,#2327,.T.);
#15704=EDGE_CURVE('',#12446,#12447,#7612,.T.);
#15705=EDGE_CURVE('',#12446,#12448,#7613,.T.);
#15706=EDGE_CURVE('',#12449,#12448,#7614,.T.);
#15707=EDGE_CURVE('',#12447,#12449,#287,.T.);
#15708=EDGE_CURVE('',#12449,#12450,#288,.T.);
#15709=EDGE_CURVE('',#12448,#12451,#7615,.T.);
#15710=EDGE_CURVE('',#12450,#12451,#7616,.T.);
#15711=EDGE_CURVE('',#12446,#12451,#2328,.T.);
#15712=EDGE_CURVE('',#12452,#12453,#7617,.T.);
#15713=EDGE_CURVE('',#12452,#12454,#7618,.T.);
#15714=EDGE_CURVE('',#12455,#12454,#7619,.T.);
#15715=EDGE_CURVE('',#12453,#12455,#289,.T.);
#15716=EDGE_CURVE('',#12455,#12456,#290,.T.);
#15717=EDGE_CURVE('',#12454,#12457,#7620,.T.);
#15718=EDGE_CURVE('',#12456,#12457,#7621,.T.);
#15719=EDGE_CURVE('',#12452,#12457,#2329,.T.);
#15720=EDGE_CURVE('',#12458,#12459,#7622,.T.);
#15721=EDGE_CURVE('',#12458,#12460,#7623,.T.);
#15722=EDGE_CURVE('',#12461,#12460,#7624,.T.);
#15723=EDGE_CURVE('',#12459,#12461,#291,.T.);
#15724=EDGE_CURVE('',#12461,#12462,#292,.T.);
#15725=EDGE_CURVE('',#12460,#12463,#7625,.T.);
#15726=EDGE_CURVE('',#12462,#12463,#7626,.T.);
#15727=EDGE_CURVE('',#12458,#12463,#2330,.T.);
#15728=EDGE_CURVE('',#12464,#12465,#7627,.T.);
#15729=EDGE_CURVE('',#12464,#12466,#7628,.T.);
#15730=EDGE_CURVE('',#12467,#12466,#7629,.T.);
#15731=EDGE_CURVE('',#12465,#12467,#293,.T.);
#15732=EDGE_CURVE('',#12467,#12468,#294,.T.);
#15733=EDGE_CURVE('',#12466,#12469,#7630,.T.);
#15734=EDGE_CURVE('',#12468,#12469,#7631,.T.);
#15735=EDGE_CURVE('',#12464,#12469,#2331,.T.);
#15736=EDGE_CURVE('',#12470,#12471,#7632,.T.);
#15737=EDGE_CURVE('',#12470,#12472,#7633,.T.);
#15738=EDGE_CURVE('',#12473,#12472,#7634,.T.);
#15739=EDGE_CURVE('',#12471,#12473,#295,.T.);
#15740=EDGE_CURVE('',#12473,#12474,#296,.T.);
#15741=EDGE_CURVE('',#12472,#12475,#7635,.T.);
#15742=EDGE_CURVE('',#12474,#12475,#7636,.T.);
#15743=EDGE_CURVE('',#12470,#12475,#2332,.T.);
#15744=EDGE_CURVE('',#12476,#12477,#7637,.T.);
#15745=EDGE_CURVE('',#12476,#12478,#7638,.T.);
#15746=EDGE_CURVE('',#12479,#12478,#7639,.T.);
#15747=EDGE_CURVE('',#12477,#12479,#297,.T.);
#15748=EDGE_CURVE('',#12479,#12480,#298,.T.);
#15749=EDGE_CURVE('',#12478,#12481,#7640,.T.);
#15750=EDGE_CURVE('',#12480,#12481,#7641,.T.);
#15751=EDGE_CURVE('',#12476,#12481,#2333,.T.);
#15752=EDGE_CURVE('',#12482,#12483,#7642,.T.);
#15753=EDGE_CURVE('',#12482,#12484,#7643,.T.);
#15754=EDGE_CURVE('',#12485,#12484,#7644,.T.);
#15755=EDGE_CURVE('',#12483,#12485,#299,.T.);
#15756=EDGE_CURVE('',#12485,#12486,#300,.T.);
#15757=EDGE_CURVE('',#12484,#12487,#7645,.T.);
#15758=EDGE_CURVE('',#12486,#12487,#7646,.T.);
#15759=EDGE_CURVE('',#12482,#12487,#2334,.T.);
#15760=EDGE_CURVE('',#12488,#12489,#7647,.T.);
#15761=EDGE_CURVE('',#12488,#12490,#7648,.T.);
#15762=EDGE_CURVE('',#12491,#12490,#7649,.T.);
#15763=EDGE_CURVE('',#12489,#12491,#301,.T.);
#15764=EDGE_CURVE('',#12491,#12492,#302,.T.);
#15765=EDGE_CURVE('',#12490,#12493,#7650,.T.);
#15766=EDGE_CURVE('',#12492,#12493,#7651,.T.);
#15767=EDGE_CURVE('',#12488,#12493,#2335,.T.);
#15768=EDGE_CURVE('',#12494,#12495,#7652,.T.);
#15769=EDGE_CURVE('',#12494,#12496,#7653,.T.);
#15770=EDGE_CURVE('',#12497,#12496,#7654,.T.);
#15771=EDGE_CURVE('',#12495,#12497,#303,.T.);
#15772=EDGE_CURVE('',#12497,#12498,#304,.T.);
#15773=EDGE_CURVE('',#12496,#12499,#7655,.T.);
#15774=EDGE_CURVE('',#12498,#12499,#7656,.T.);
#15775=EDGE_CURVE('',#12494,#12499,#2336,.T.);
#15776=EDGE_CURVE('',#12500,#12501,#7657,.T.);
#15777=EDGE_CURVE('',#12500,#12502,#7658,.T.);
#15778=EDGE_CURVE('',#12503,#12502,#7659,.T.);
#15779=EDGE_CURVE('',#12501,#12503,#305,.T.);
#15780=EDGE_CURVE('',#12503,#12504,#306,.T.);
#15781=EDGE_CURVE('',#12502,#12505,#7660,.T.);
#15782=EDGE_CURVE('',#12504,#12505,#7661,.T.);
#15783=EDGE_CURVE('',#12500,#12505,#2337,.T.);
#15784=EDGE_CURVE('',#12506,#12507,#7662,.T.);
#15785=EDGE_CURVE('',#12506,#12508,#7663,.T.);
#15786=EDGE_CURVE('',#12509,#12508,#7664,.T.);
#15787=EDGE_CURVE('',#12507,#12509,#307,.T.);
#15788=EDGE_CURVE('',#12509,#12510,#308,.T.);
#15789=EDGE_CURVE('',#12508,#12511,#7665,.T.);
#15790=EDGE_CURVE('',#12510,#12511,#7666,.T.);
#15791=EDGE_CURVE('',#12506,#12511,#2338,.T.);
#15792=EDGE_CURVE('',#12512,#12513,#7667,.T.);
#15793=EDGE_CURVE('',#12512,#12514,#7668,.T.);
#15794=EDGE_CURVE('',#12515,#12514,#7669,.T.);
#15795=EDGE_CURVE('',#12513,#12515,#309,.T.);
#15796=EDGE_CURVE('',#12515,#12516,#310,.T.);
#15797=EDGE_CURVE('',#12514,#12517,#7670,.T.);
#15798=EDGE_CURVE('',#12516,#12517,#7671,.T.);
#15799=EDGE_CURVE('',#12512,#12517,#2339,.T.);
#15800=EDGE_CURVE('',#12518,#12519,#7672,.T.);
#15801=EDGE_CURVE('',#12518,#12520,#7673,.T.);
#15802=EDGE_CURVE('',#12521,#12520,#7674,.T.);
#15803=EDGE_CURVE('',#12519,#12521,#311,.T.);
#15804=EDGE_CURVE('',#12521,#12522,#312,.T.);
#15805=EDGE_CURVE('',#12520,#12523,#7675,.T.);
#15806=EDGE_CURVE('',#12522,#12523,#7676,.T.);
#15807=EDGE_CURVE('',#12518,#12523,#2340,.T.);
#15808=EDGE_CURVE('',#12524,#12525,#7677,.T.);
#15809=EDGE_CURVE('',#12524,#12526,#7678,.T.);
#15810=EDGE_CURVE('',#12527,#12526,#7679,.T.);
#15811=EDGE_CURVE('',#12525,#12527,#313,.T.);
#15812=EDGE_CURVE('',#12527,#12528,#314,.T.);
#15813=EDGE_CURVE('',#12526,#12529,#7680,.T.);
#15814=EDGE_CURVE('',#12528,#12529,#7681,.T.);
#15815=EDGE_CURVE('',#12524,#12529,#2341,.T.);
#15816=EDGE_CURVE('',#12530,#12531,#7682,.T.);
#15817=EDGE_CURVE('',#12530,#12532,#7683,.T.);
#15818=EDGE_CURVE('',#12533,#12532,#7684,.T.);
#15819=EDGE_CURVE('',#12531,#12533,#315,.T.);
#15820=EDGE_CURVE('',#12533,#12534,#316,.T.);
#15821=EDGE_CURVE('',#12532,#12535,#7685,.T.);
#15822=EDGE_CURVE('',#12534,#12535,#7686,.T.);
#15823=EDGE_CURVE('',#12530,#12535,#2342,.T.);
#15824=EDGE_CURVE('',#12536,#12537,#7687,.T.);
#15825=EDGE_CURVE('',#12536,#12538,#7688,.T.);
#15826=EDGE_CURVE('',#12539,#12538,#7689,.T.);
#15827=EDGE_CURVE('',#12537,#12539,#317,.T.);
#15828=EDGE_CURVE('',#12539,#12540,#318,.T.);
#15829=EDGE_CURVE('',#12538,#12541,#7690,.T.);
#15830=EDGE_CURVE('',#12540,#12541,#7691,.T.);
#15831=EDGE_CURVE('',#12536,#12541,#2343,.T.);
#15832=EDGE_CURVE('',#12542,#12542,#2344,.T.);
#15833=EDGE_CURVE('',#12542,#12430,#7692,.T.);
#15834=EDGE_CURVE('',#12431,#12507,#2345,.T.);
#15835=EDGE_CURVE('',#12510,#12422,#2346,.T.);
#15836=EDGE_CURVE('',#12425,#12513,#2347,.T.);
#15837=EDGE_CURVE('',#12516,#12416,#2348,.T.);
#15838=EDGE_CURVE('',#12419,#12519,#2349,.T.);
#15839=EDGE_CURVE('',#12522,#12410,#2350,.T.);
#15840=EDGE_CURVE('',#12413,#12525,#2351,.T.);
#15841=EDGE_CURVE('',#12528,#12404,#2352,.T.);
#15842=EDGE_CURVE('',#12407,#12531,#2353,.T.);
#15843=EDGE_CURVE('',#12534,#12398,#2354,.T.);
#15844=EDGE_CURVE('',#12401,#12537,#2355,.T.);
#15845=EDGE_CURVE('',#12540,#12501,#2356,.T.);
#15846=EDGE_CURVE('',#12504,#12465,#2357,.T.);
#15847=EDGE_CURVE('',#12468,#12471,#2358,.T.);
#15848=EDGE_CURVE('',#12474,#12459,#2359,.T.);
#15849=EDGE_CURVE('',#12462,#12477,#2360,.T.);
#15850=EDGE_CURVE('',#12480,#12453,#2361,.T.);
#15851=EDGE_CURVE('',#12456,#12483,#2362,.T.);
#15852=EDGE_CURVE('',#12486,#12447,#2363,.T.);
#15853=EDGE_CURVE('',#12450,#12489,#2364,.T.);
#15854=EDGE_CURVE('',#12492,#12441,#2365,.T.);
#15855=EDGE_CURVE('',#12444,#12495,#2366,.T.);
#15856=EDGE_CURVE('',#12498,#12435,#2367,.T.);
#15857=EDGE_CURVE('',#12438,#12428,#2368,.T.);
#15858=EDGE_CURVE('',#12541,#12500,#2369,.T.);
#15859=EDGE_CURVE('',#12469,#12470,#2370,.T.);
#15860=EDGE_CURVE('',#12505,#12464,#2371,.T.);
#15861=EDGE_CURVE('',#12463,#12476,#2372,.T.);
#15862=EDGE_CURVE('',#12475,#12458,#2373,.T.);
#15863=EDGE_CURVE('',#12457,#12482,#2374,.T.);
#15864=EDGE_CURVE('',#12481,#12452,#2375,.T.);
#15865=EDGE_CURVE('',#12451,#12488,#2376,.T.);
#15866=EDGE_CURVE('',#12487,#12446,#2377,.T.);
#15867=EDGE_CURVE('',#12445,#12494,#2378,.T.);
#15868=EDGE_CURVE('',#12493,#12440,#2379,.T.);
#15869=EDGE_CURVE('',#12499,#12434,#2380,.T.);
#15870=EDGE_CURVE('',#12432,#12506,#2381,.T.);
#15871=EDGE_CURVE('',#12439,#12427,#2382,.T.);
#15872=EDGE_CURVE('',#12426,#12512,#2383,.T.);
#15873=EDGE_CURVE('',#12511,#12421,#2384,.T.);
#15874=EDGE_CURVE('',#12420,#12518,#2385,.T.);
#15875=EDGE_CURVE('',#12517,#12415,#2386,.T.);
#15876=EDGE_CURVE('',#12414,#12524,#2387,.T.);
#15877=EDGE_CURVE('',#12523,#12409,#2388,.T.);
#15878=EDGE_CURVE('',#12408,#12530,#2389,.T.);
#15879=EDGE_CURVE('',#12529,#12403,#2390,.T.);
#15880=EDGE_CURVE('',#12402,#12536,#2391,.T.);
#15881=EDGE_CURVE('',#12543,#12390,#803,.T.);
#15882=EDGE_CURVE('',#12385,#12543,#804,.T.);
#15883=EDGE_CURVE('',#12544,#12377,#805,.T.);
#15884=EDGE_CURVE('',#12544,#12396,#806,.T.);
#15885=EDGE_CURVE('',#12545,#12544,#2392,.T.);
#15886=EDGE_CURVE('',#12545,#12395,#807,.T.);
#15887=EDGE_CURVE('',#12389,#12386,#808,.T.);
#15888=EDGE_CURVE('',#12376,#12545,#809,.T.);
#15889=EDGE_CURVE('',#12384,#12543,#2393,.T.);
#15890=EDGE_CURVE('',#12546,#12546,#2394,.T.);
#15891=EDGE_CURVE('',#12547,#12547,#2395,.T.);
#15892=EDGE_CURVE('',#12547,#12546,#7693,.T.);
#15893=EDGE_CURVE('',#12548,#12548,#2396,.T.);
#15894=EDGE_CURVE('',#12548,#12547,#7694,.T.);
#15895=EDGE_CURVE('',#12549,#12549,#2397,.T.);
#15896=EDGE_CURVE('',#12549,#12548,#7695,.T.);
#15897=EDGE_CURVE('',#12550,#12550,#2398,.T.);
#15898=EDGE_CURVE('',#12535,#12397,#2399,.T.);
#15899=EDGE_CURVE('',#12433,#12550,#7696,.T.);
#15900=EDGE_CURVE('',#12551,#12552,#7697,.T.);
#15901=EDGE_CURVE('',#12551,#12553,#810,.T.);
#15902=EDGE_CURVE('',#12553,#12554,#2400,.T.);
#15903=EDGE_CURVE('',#12554,#12552,#811,.T.);
#15904=EDGE_CURVE('',#12555,#12556,#7698,.T.);
#15905=EDGE_CURVE('',#12555,#12551,#812,.T.);
#15906=EDGE_CURVE('',#12552,#12556,#813,.T.);
#15907=EDGE_CURVE('',#12557,#12558,#7699,.T.);
#15908=EDGE_CURVE('',#12557,#12555,#814,.T.);
#15909=EDGE_CURVE('',#12556,#12558,#815,.T.);
#15910=EDGE_CURVE('',#12559,#12560,#7700,.T.);
#15911=EDGE_CURVE('',#12559,#12557,#816,.T.);
#15912=EDGE_CURVE('',#12558,#12560,#817,.T.);
#15913=EDGE_CURVE('',#12561,#12562,#7701,.T.);
#15914=EDGE_CURVE('',#12561,#12559,#818,.T.);
#15915=EDGE_CURVE('',#12560,#12562,#819,.T.);
#15916=EDGE_CURVE('',#12563,#12564,#7702,.T.);
#15917=EDGE_CURVE('',#12563,#12561,#820,.T.);
#15918=EDGE_CURVE('',#12562,#12564,#821,.T.);
#15919=EDGE_CURVE('',#12565,#12566,#7703,.T.);
#15920=EDGE_CURVE('',#12565,#12563,#822,.T.);
#15921=EDGE_CURVE('',#12564,#12566,#823,.T.);
#15922=EDGE_CURVE('',#12567,#12568,#7704,.T.);
#15923=EDGE_CURVE('',#12567,#12565,#824,.T.);
#15924=EDGE_CURVE('',#12566,#12568,#825,.T.);
#15925=EDGE_CURVE('',#12569,#12570,#7705,.T.);
#15926=EDGE_CURVE('',#12569,#12567,#826,.T.);
#15927=EDGE_CURVE('',#12568,#12570,#827,.T.);
#15928=EDGE_CURVE('',#12571,#12572,#7706,.T.);
#15929=EDGE_CURVE('',#12571,#12569,#828,.T.);
#15930=EDGE_CURVE('',#12570,#12572,#829,.T.);
#15931=EDGE_CURVE('',#12573,#12574,#7707,.T.);
#15932=EDGE_CURVE('',#12573,#12571,#830,.T.);
#15933=EDGE_CURVE('',#12572,#12574,#831,.T.);
#15934=EDGE_CURVE('',#12575,#12576,#7708,.T.);
#15935=EDGE_CURVE('',#12575,#12573,#832,.T.);
#15936=EDGE_CURVE('',#12574,#12576,#833,.T.);
#15937=EDGE_CURVE('',#12577,#12578,#7709,.T.);
#15938=EDGE_CURVE('',#12577,#12575,#834,.T.);
#15939=EDGE_CURVE('',#12576,#12578,#835,.T.);
#15940=EDGE_CURVE('',#12579,#12580,#7710,.T.);
#15941=EDGE_CURVE('',#12579,#12577,#836,.T.);
#15942=EDGE_CURVE('',#12578,#12580,#837,.T.);
#15943=EDGE_CURVE('',#12581,#12582,#7711,.T.);
#15944=EDGE_CURVE('',#12581,#12579,#838,.T.);
#15945=EDGE_CURVE('',#12580,#12582,#839,.T.);
#15946=EDGE_CURVE('',#12583,#12584,#7712,.T.);
#15947=EDGE_CURVE('',#12583,#12585,#840,.T.);
#15948=EDGE_CURVE('',#12586,#12585,#2401,.T.);
#15949=EDGE_CURVE('',#12584,#12586,#841,.T.);
#15950=EDGE_CURVE('',#12587,#12588,#7713,.T.);
#15951=EDGE_CURVE('',#12587,#12583,#842,.T.);
#15952=EDGE_CURVE('',#12588,#12584,#843,.T.);
#15953=EDGE_CURVE('',#12589,#12590,#7714,.T.);
#15954=EDGE_CURVE('',#12589,#12587,#844,.T.);
#15955=EDGE_CURVE('',#12590,#12588,#845,.T.);
#15956=EDGE_CURVE('',#12591,#12592,#7715,.T.);
#15957=EDGE_CURVE('',#12591,#12589,#846,.T.);
#15958=EDGE_CURVE('',#12592,#12590,#847,.T.);
#15959=EDGE_CURVE('',#12593,#12594,#7716,.T.);
#15960=EDGE_CURVE('',#12593,#12591,#848,.T.);
#15961=EDGE_CURVE('',#12594,#12592,#849,.T.);
#15962=EDGE_CURVE('',#12595,#12596,#7717,.T.);
#15963=EDGE_CURVE('',#12595,#12593,#850,.T.);
#15964=EDGE_CURVE('',#12596,#12594,#851,.T.);
#15965=EDGE_CURVE('',#12597,#12598,#7718,.T.);
#15966=EDGE_CURVE('',#12597,#12595,#852,.T.);
#15967=EDGE_CURVE('',#12598,#12596,#853,.T.);
#15968=EDGE_CURVE('',#12599,#12600,#7719,.T.);
#15969=EDGE_CURVE('',#12599,#12597,#854,.T.);
#15970=EDGE_CURVE('',#12600,#12598,#855,.T.);
#15971=EDGE_CURVE('',#12601,#12602,#7720,.T.);
#15972=EDGE_CURVE('',#12601,#12599,#856,.T.);
#15973=EDGE_CURVE('',#12602,#12600,#857,.T.);
#15974=EDGE_CURVE('',#12603,#12604,#7721,.T.);
#15975=EDGE_CURVE('',#12603,#12601,#858,.T.);
#15976=EDGE_CURVE('',#12604,#12602,#859,.T.);
#15977=EDGE_CURVE('',#12605,#12606,#7722,.T.);
#15978=EDGE_CURVE('',#12605,#12603,#860,.T.);
#15979=EDGE_CURVE('',#12606,#12604,#861,.T.);
#15980=EDGE_CURVE('',#12607,#12608,#7723,.T.);
#15981=EDGE_CURVE('',#12607,#12605,#862,.T.);
#15982=EDGE_CURVE('',#12608,#12606,#863,.T.);
#15983=EDGE_CURVE('',#12609,#12610,#7724,.T.);
#15984=EDGE_CURVE('',#12609,#12607,#864,.T.);
#15985=EDGE_CURVE('',#12610,#12608,#865,.T.);
#15986=EDGE_CURVE('',#12611,#12612,#7725,.T.);
#15987=EDGE_CURVE('',#12611,#12609,#866,.T.);
#15988=EDGE_CURVE('',#12612,#12610,#867,.T.);
#15989=EDGE_CURVE('',#12613,#12614,#7726,.T.);
#15990=EDGE_CURVE('',#12613,#12611,#868,.T.);
#15991=EDGE_CURVE('',#12614,#12612,#869,.T.);
#15992=EDGE_CURVE('',#12615,#12616,#319,.T.);
#15993=EDGE_CURVE('',#12615,#12617,#7727,.T.);
#15994=EDGE_CURVE('',#12617,#12618,#7728,.T.);
#15995=EDGE_CURVE('',#12616,#12618,#7729,.T.);
#15996=EDGE_CURVE('',#12618,#12619,#2402,.T.);
#15997=EDGE_CURVE('',#12619,#12617,#7730,.T.);
#15998=EDGE_CURVE('',#12620,#12615,#320,.T.);
#15999=EDGE_CURVE('',#12619,#12620,#7731,.T.);
#16000=EDGE_CURVE('',#12621,#12622,#321,.T.);
#16001=EDGE_CURVE('',#12621,#12623,#7732,.T.);
#16002=EDGE_CURVE('',#12623,#12624,#7733,.T.);
#16003=EDGE_CURVE('',#12622,#12624,#7734,.T.);
#16004=EDGE_CURVE('',#12624,#12625,#2403,.T.);
#16005=EDGE_CURVE('',#12625,#12623,#7735,.T.);
#16006=EDGE_CURVE('',#12626,#12621,#322,.T.);
#16007=EDGE_CURVE('',#12625,#12626,#7736,.T.);
#16008=EDGE_CURVE('',#12627,#12628,#323,.T.);
#16009=EDGE_CURVE('',#12627,#12629,#7737,.T.);
#16010=EDGE_CURVE('',#12629,#12630,#7738,.T.);
#16011=EDGE_CURVE('',#12628,#12630,#7739,.T.);
#16012=EDGE_CURVE('',#12630,#12631,#2404,.T.);
#16013=EDGE_CURVE('',#12631,#12629,#7740,.T.);
#16014=EDGE_CURVE('',#12632,#12627,#324,.T.);
#16015=EDGE_CURVE('',#12631,#12632,#7741,.T.);
#16016=EDGE_CURVE('',#12633,#12634,#325,.T.);
#16017=EDGE_CURVE('',#12633,#12635,#7742,.T.);
#16018=EDGE_CURVE('',#12635,#12636,#7743,.T.);
#16019=EDGE_CURVE('',#12634,#12636,#7744,.T.);
#16020=EDGE_CURVE('',#12636,#12637,#2405,.T.);
#16021=EDGE_CURVE('',#12637,#12635,#7745,.T.);
#16022=EDGE_CURVE('',#12638,#12633,#326,.T.);
#16023=EDGE_CURVE('',#12637,#12638,#7746,.T.);
#16024=EDGE_CURVE('',#12639,#12640,#327,.T.);
#16025=EDGE_CURVE('',#12639,#12641,#7747,.T.);
#16026=EDGE_CURVE('',#12641,#12642,#7748,.T.);
#16027=EDGE_CURVE('',#12640,#12642,#7749,.T.);
#16028=EDGE_CURVE('',#12642,#12643,#2406,.T.);
#16029=EDGE_CURVE('',#12643,#12641,#7750,.T.);
#16030=EDGE_CURVE('',#12644,#12639,#328,.T.);
#16031=EDGE_CURVE('',#12643,#12644,#7751,.T.);
#16032=EDGE_CURVE('',#12645,#12646,#329,.T.);
#16033=EDGE_CURVE('',#12645,#12647,#7752,.T.);
#16034=EDGE_CURVE('',#12647,#12648,#7753,.T.);
#16035=EDGE_CURVE('',#12646,#12648,#7754,.T.);
#16036=EDGE_CURVE('',#12648,#12649,#2407,.T.);
#16037=EDGE_CURVE('',#12649,#12647,#7755,.T.);
#16038=EDGE_CURVE('',#12650,#12645,#330,.T.);
#16039=EDGE_CURVE('',#12649,#12650,#7756,.T.);
#16040=EDGE_CURVE('',#12651,#12652,#331,.T.);
#16041=EDGE_CURVE('',#12651,#12653,#7757,.T.);
#16042=EDGE_CURVE('',#12653,#12654,#7758,.T.);
#16043=EDGE_CURVE('',#12652,#12654,#7759,.T.);
#16044=EDGE_CURVE('',#12654,#12655,#2408,.T.);
#16045=EDGE_CURVE('',#12655,#12653,#7760,.T.);
#16046=EDGE_CURVE('',#12656,#12651,#332,.T.);
#16047=EDGE_CURVE('',#12655,#12656,#7761,.T.);
#16048=EDGE_CURVE('',#12657,#12658,#333,.T.);
#16049=EDGE_CURVE('',#12657,#12659,#7762,.T.);
#16050=EDGE_CURVE('',#12659,#12660,#7763,.T.);
#16051=EDGE_CURVE('',#12658,#12660,#7764,.T.);
#16052=EDGE_CURVE('',#12660,#12661,#2409,.T.);
#16053=EDGE_CURVE('',#12661,#12659,#7765,.T.);
#16054=EDGE_CURVE('',#12662,#12657,#334,.T.);
#16055=EDGE_CURVE('',#12661,#12662,#7766,.T.);
#16056=EDGE_CURVE('',#12663,#12664,#335,.T.);
#16057=EDGE_CURVE('',#12663,#12665,#7767,.T.);
#16058=EDGE_CURVE('',#12665,#12666,#7768,.T.);
#16059=EDGE_CURVE('',#12664,#12666,#7769,.T.);
#16060=EDGE_CURVE('',#12666,#12667,#2410,.T.);
#16061=EDGE_CURVE('',#12667,#12665,#7770,.T.);
#16062=EDGE_CURVE('',#12668,#12663,#336,.T.);
#16063=EDGE_CURVE('',#12667,#12668,#7771,.T.);
#16064=EDGE_CURVE('',#12669,#12670,#337,.T.);
#16065=EDGE_CURVE('',#12669,#12671,#7772,.T.);
#16066=EDGE_CURVE('',#12671,#12672,#7773,.T.);
#16067=EDGE_CURVE('',#12670,#12672,#7774,.T.);
#16068=EDGE_CURVE('',#12672,#12673,#2411,.T.);
#16069=EDGE_CURVE('',#12673,#12671,#7775,.T.);
#16070=EDGE_CURVE('',#12674,#12669,#338,.T.);
#16071=EDGE_CURVE('',#12673,#12674,#7776,.T.);
#16072=EDGE_CURVE('',#12675,#12676,#339,.T.);
#16073=EDGE_CURVE('',#12675,#12677,#7777,.T.);
#16074=EDGE_CURVE('',#12677,#12678,#7778,.T.);
#16075=EDGE_CURVE('',#12676,#12678,#7779,.T.);
#16076=EDGE_CURVE('',#12678,#12679,#2412,.T.);
#16077=EDGE_CURVE('',#12679,#12677,#7780,.T.);
#16078=EDGE_CURVE('',#12680,#12675,#340,.T.);
#16079=EDGE_CURVE('',#12679,#12680,#7781,.T.);
#16080=EDGE_CURVE('',#12681,#12682,#341,.T.);
#16081=EDGE_CURVE('',#12681,#12683,#7782,.T.);
#16082=EDGE_CURVE('',#12683,#12684,#7783,.T.);
#16083=EDGE_CURVE('',#12682,#12684,#7784,.T.);
#16084=EDGE_CURVE('',#12684,#12685,#2413,.T.);
#16085=EDGE_CURVE('',#12685,#12683,#7785,.T.);
#16086=EDGE_CURVE('',#12686,#12681,#342,.T.);
#16087=EDGE_CURVE('',#12685,#12686,#7786,.T.);
#16088=EDGE_CURVE('',#12687,#12688,#343,.T.);
#16089=EDGE_CURVE('',#12687,#12689,#7787,.T.);
#16090=EDGE_CURVE('',#12689,#12690,#7788,.T.);
#16091=EDGE_CURVE('',#12688,#12690,#7789,.T.);
#16092=EDGE_CURVE('',#12690,#12691,#2414,.T.);
#16093=EDGE_CURVE('',#12691,#12689,#7790,.T.);
#16094=EDGE_CURVE('',#12692,#12687,#344,.T.);
#16095=EDGE_CURVE('',#12691,#12692,#7791,.T.);
#16096=EDGE_CURVE('',#12693,#12694,#345,.T.);
#16097=EDGE_CURVE('',#12693,#12695,#7792,.T.);
#16098=EDGE_CURVE('',#12695,#12696,#7793,.T.);
#16099=EDGE_CURVE('',#12694,#12696,#7794,.T.);
#16100=EDGE_CURVE('',#12696,#12697,#2415,.T.);
#16101=EDGE_CURVE('',#12698,#12695,#7795,.T.);
#16102=EDGE_CURVE('',#12697,#12698,#2416,.T.);
#16103=EDGE_CURVE('',#12699,#12693,#346,.T.);
#16104=EDGE_CURVE('',#12698,#12699,#7796,.T.);
#16105=EDGE_CURVE('',#12700,#12701,#347,.T.);
#16106=EDGE_CURVE('',#12700,#12702,#7797,.T.);
#16107=EDGE_CURVE('',#12702,#12703,#7798,.T.);
#16108=EDGE_CURVE('',#12701,#12703,#7799,.T.);
#16109=EDGE_CURVE('',#12703,#12704,#2417,.T.);
#16110=EDGE_CURVE('',#12704,#12702,#7800,.T.);
#16111=EDGE_CURVE('',#12705,#12700,#348,.T.);
#16112=EDGE_CURVE('',#12704,#12705,#7801,.T.);
#16113=EDGE_CURVE('',#12706,#12707,#349,.T.);
#16114=EDGE_CURVE('',#12706,#12708,#7802,.T.);
#16115=EDGE_CURVE('',#12708,#12709,#7803,.T.);
#16116=EDGE_CURVE('',#12707,#12709,#7804,.T.);
#16117=EDGE_CURVE('',#12709,#12710,#2418,.T.);
#16118=EDGE_CURVE('',#12710,#12708,#7805,.T.);
#16119=EDGE_CURVE('',#12711,#12706,#350,.T.);
#16120=EDGE_CURVE('',#12710,#12711,#7806,.T.);
#16121=EDGE_CURVE('',#12712,#12713,#351,.T.);
#16122=EDGE_CURVE('',#12712,#12714,#7807,.T.);
#16123=EDGE_CURVE('',#12714,#12715,#7808,.T.);
#16124=EDGE_CURVE('',#12713,#12715,#7809,.T.);
#16125=EDGE_CURVE('',#12715,#12716,#2419,.T.);
#16126=EDGE_CURVE('',#12716,#12714,#7810,.T.);
#16127=EDGE_CURVE('',#12717,#12712,#352,.T.);
#16128=EDGE_CURVE('',#12716,#12717,#7811,.T.);
#16129=EDGE_CURVE('',#12718,#12719,#353,.T.);
#16130=EDGE_CURVE('',#12718,#12720,#7812,.T.);
#16131=EDGE_CURVE('',#12720,#12721,#7813,.T.);
#16132=EDGE_CURVE('',#12719,#12721,#7814,.T.);
#16133=EDGE_CURVE('',#12721,#12722,#2420,.T.);
#16134=EDGE_CURVE('',#12722,#12720,#7815,.T.);
#16135=EDGE_CURVE('',#12723,#12718,#354,.T.);
#16136=EDGE_CURVE('',#12722,#12723,#7816,.T.);
#16137=EDGE_CURVE('',#12713,#12620,#2421,.T.);
#16138=EDGE_CURVE('',#12622,#12717,#2422,.T.);
#16139=EDGE_CURVE('',#12707,#12626,#2423,.T.);
#16140=EDGE_CURVE('',#12628,#12711,#2424,.T.);
#16141=EDGE_CURVE('',#12701,#12632,#2425,.T.);
#16142=EDGE_CURVE('',#12634,#12705,#2426,.T.);
#16143=EDGE_CURVE('',#12694,#12638,#2427,.T.);
#16144=EDGE_CURVE('',#12697,#12724,#7817,.T.);
#16145=EDGE_CURVE('',#12724,#12724,#2428,.T.);
#16146=EDGE_CURVE('',#12688,#12699,#2429,.T.);
#16147=EDGE_CURVE('',#12646,#12692,#2430,.T.);
#16148=EDGE_CURVE('',#12682,#12650,#2431,.T.);
#16149=EDGE_CURVE('',#12652,#12686,#2432,.T.);
#16150=EDGE_CURVE('',#12676,#12656,#2433,.T.);
#16151=EDGE_CURVE('',#12658,#12680,#2434,.T.);
#16152=EDGE_CURVE('',#12670,#12662,#2435,.T.);
#16153=EDGE_CURVE('',#12664,#12674,#2436,.T.);
#16154=EDGE_CURVE('',#12640,#12668,#2437,.T.);
#16155=EDGE_CURVE('',#12719,#12644,#2438,.T.);
#16156=EDGE_CURVE('',#12616,#12723,#2439,.T.);
#16157=EDGE_CURVE('',#12725,#12586,#870,.T.);
#16158=EDGE_CURVE('',#12582,#12725,#871,.T.);
#16159=EDGE_CURVE('',#12726,#12554,#872,.T.);
#16160=EDGE_CURVE('',#12726,#12614,#873,.T.);
#16161=EDGE_CURVE('',#12554,#12727,#2440,.T.);
#16162=EDGE_CURVE('',#12727,#12553,#2441,.T.);
#16163=EDGE_CURVE('',#12553,#12728,#874,.T.);
#16164=EDGE_CURVE('',#12728,#12726,#2442,.T.);
#16165=EDGE_CURVE('',#12728,#12613,#875,.T.);
#16166=EDGE_CURVE('',#12585,#12729,#876,.T.);
#16167=EDGE_CURVE('',#12729,#12581,#877,.T.);
#16168=EDGE_CURVE('',#12730,#12730,#2443,.T.);
#16169=EDGE_CURVE('',#12727,#12730,#7818,.T.);
#16170=EDGE_CURVE('',#12729,#12725,#2444,.T.);
#16171=EDGE_CURVE('',#12731,#12731,#2445,.T.);
#16172=EDGE_CURVE('',#12724,#12731,#7819,.T.);
#16173=EDGE_CURVE('',#12732,#12732,#2446,.T.);
#16174=EDGE_CURVE('',#12732,#12693,#7820,.T.);
#16175=EDGE_CURVE('',#12733,#12733,#2447,.T.);
#16176=EDGE_CURVE('',#12733,#12734,#7821,.T.);
#16177=EDGE_CURVE('',#12734,#12734,#2448,.T.);
#16178=EDGE_CURVE('',#12735,#12736,#7822,.T.);
#16179=EDGE_CURVE('',#12736,#12737,#7823,.T.);
#16180=EDGE_CURVE('',#12737,#12738,#7824,.T.);
#16181=EDGE_CURVE('',#12738,#12739,#7825,.T.);
#16182=EDGE_CURVE('',#12739,#12740,#7826,.T.);
#16183=EDGE_CURVE('',#12740,#12735,#7827,.T.);
#16184=EDGE_CURVE('',#12741,#12741,#2449,.T.);
#16185=EDGE_CURVE('',#12742,#12743,#7828,.T.);
#16186=EDGE_CURVE('',#12743,#12735,#7829,.T.);
#16187=EDGE_CURVE('',#12742,#12740,#7830,.T.);
#16188=EDGE_CURVE('',#12744,#12742,#7831,.T.);
#16189=EDGE_CURVE('',#12744,#12739,#7832,.T.);
#16190=EDGE_CURVE('',#12745,#12744,#7833,.T.);
#16191=EDGE_CURVE('',#12745,#12738,#7834,.T.);
#16192=EDGE_CURVE('',#12746,#12745,#7835,.T.);
#16193=EDGE_CURVE('',#12746,#12737,#7836,.T.);
#16194=EDGE_CURVE('',#12747,#12746,#7837,.T.);
#16195=EDGE_CURVE('',#12747,#12736,#7838,.T.);
#16196=EDGE_CURVE('',#12743,#12747,#7839,.T.);
#16197=EDGE_CURVE('',#12748,#12749,#7840,.T.);
#16198=EDGE_CURVE('',#12748,#12749,#2450,.T.);
#16199=EDGE_CURVE('',#12750,#12751,#7841,.T.);
#16200=EDGE_CURVE('',#12750,#12752,#2451,.T.);
#16201=EDGE_CURVE('',#12752,#12751,#2452,.T.);
#16202=EDGE_CURVE('',#12751,#12748,#878,.T.);
#16203=EDGE_CURVE('',#12752,#12741,#7842,.T.);
#16204=EDGE_CURVE('',#12749,#12750,#879,.T.);
#16205=EDGE_CURVE('',#12753,#12754,#2453,.T.);
#16206=EDGE_CURVE('',#12753,#12755,#7843,.T.);
#16207=EDGE_CURVE('',#12756,#12755,#2454,.T.);
#16208=EDGE_CURVE('',#12754,#12756,#7844,.T.);
#16209=EDGE_CURVE('',#12754,#12757,#7845,.T.);
#16210=EDGE_CURVE('',#12758,#12756,#7846,.T.);
#16211=EDGE_CURVE('',#12757,#12758,#7847,.T.);
#16212=EDGE_CURVE('',#12757,#12759,#7848,.T.);
#16213=EDGE_CURVE('',#12760,#12758,#7849,.T.);
#16214=EDGE_CURVE('',#12759,#12760,#7850,.T.);
#16215=EDGE_CURVE('',#12759,#12761,#7851,.T.);
#16216=EDGE_CURVE('',#12762,#12760,#7852,.T.);
#16217=EDGE_CURVE('',#12761,#12762,#7853,.T.);
#16218=EDGE_CURVE('',#12761,#12763,#2455,.T.);
#16219=EDGE_CURVE('',#12764,#12762,#2456,.T.);
#16220=EDGE_CURVE('',#12763,#12764,#7854,.T.);
#16221=EDGE_CURVE('',#12763,#12765,#7855,.T.);
#16222=EDGE_CURVE('',#12766,#12764,#7856,.T.);
#16223=EDGE_CURVE('',#12765,#12766,#7857,.T.);
#16224=EDGE_CURVE('',#12765,#12753,#7858,.T.);
#16225=EDGE_CURVE('',#12755,#12766,#7859,.T.);
#16226=EDGE_CURVE('',#12767,#12768,#7860,.T.);
#16227=EDGE_CURVE('',#12767,#12769,#7861,.T.);
#16228=EDGE_CURVE('',#12769,#12770,#7862,.T.);
#16229=EDGE_CURVE('',#12768,#12770,#7863,.T.);
#16230=EDGE_CURVE('',#12771,#12767,#7864,.T.);
#16231=EDGE_CURVE('',#12771,#12772,#7865,.T.);
#16232=EDGE_CURVE('',#12772,#12769,#7866,.T.);
#16233=EDGE_CURVE('',#12773,#12771,#7867,.T.);
#16234=EDGE_CURVE('',#12773,#12774,#7868,.T.);
#16235=EDGE_CURVE('',#12774,#12772,#7869,.T.);
#16236=EDGE_CURVE('',#12768,#12773,#7870,.T.);
#16237=EDGE_CURVE('',#12770,#12774,#7871,.T.);
#16238=EDGE_CURVE('',#12775,#12776,#7872,.T.);
#16239=EDGE_CURVE('',#12775,#12777,#7873,.T.);
#16240=EDGE_CURVE('',#12777,#12778,#7874,.T.);
#16241=EDGE_CURVE('',#12776,#12778,#7875,.T.);
#16242=EDGE_CURVE('',#12779,#12775,#7876,.T.);
#16243=EDGE_CURVE('',#12779,#12780,#7877,.T.);
#16244=EDGE_CURVE('',#12780,#12777,#7878,.T.);
#16245=EDGE_CURVE('',#12781,#12779,#7879,.T.);
#16246=EDGE_CURVE('',#12781,#12782,#7880,.T.);
#16247=EDGE_CURVE('',#12782,#12780,#7881,.T.);
#16248=EDGE_CURVE('',#12776,#12781,#7882,.T.);
#16249=EDGE_CURVE('',#12778,#12782,#7883,.T.);
#16250=EDGE_CURVE('',#12783,#12784,#7884,.T.);
#16251=EDGE_CURVE('',#12783,#12785,#7885,.T.);
#16252=EDGE_CURVE('',#12785,#12786,#7886,.T.);
#16253=EDGE_CURVE('',#12784,#12786,#7887,.T.);
#16254=EDGE_CURVE('',#12787,#12783,#7888,.T.);
#16255=EDGE_CURVE('',#12787,#12788,#7889,.T.);
#16256=EDGE_CURVE('',#12788,#12785,#7890,.T.);
#16257=EDGE_CURVE('',#12789,#12787,#7891,.T.);
#16258=EDGE_CURVE('',#12789,#12790,#7892,.T.);
#16259=EDGE_CURVE('',#12790,#12788,#7893,.T.);
#16260=EDGE_CURVE('',#12784,#12789,#7894,.T.);
#16261=EDGE_CURVE('',#12786,#12790,#7895,.T.);
#16262=EDGE_CURVE('',#12791,#12792,#7896,.T.);
#16263=EDGE_CURVE('',#12791,#12793,#7897,.T.);
#16264=EDGE_CURVE('',#12793,#12794,#7898,.T.);
#16265=EDGE_CURVE('',#12792,#12794,#7899,.T.);
#16266=EDGE_CURVE('',#12795,#12791,#7900,.T.);
#16267=EDGE_CURVE('',#12795,#12796,#7901,.T.);
#16268=EDGE_CURVE('',#12796,#12793,#7902,.T.);
#16269=EDGE_CURVE('',#12797,#12795,#7903,.T.);
#16270=EDGE_CURVE('',#12797,#12798,#7904,.T.);
#16271=EDGE_CURVE('',#12798,#12796,#7905,.T.);
#16272=EDGE_CURVE('',#12792,#12797,#7906,.T.);
#16273=EDGE_CURVE('',#12794,#12798,#7907,.T.);
#16274=EDGE_CURVE('',#12799,#12800,#7908,.T.);
#16275=EDGE_CURVE('',#12799,#12801,#7909,.T.);
#16276=EDGE_CURVE('',#12801,#12802,#7910,.T.);
#16277=EDGE_CURVE('',#12800,#12802,#7911,.T.);
#16278=EDGE_CURVE('',#12803,#12799,#7912,.T.);
#16279=EDGE_CURVE('',#12803,#12804,#7913,.T.);
#16280=EDGE_CURVE('',#12804,#12801,#7914,.T.);
#16281=EDGE_CURVE('',#12805,#12803,#7915,.T.);
#16282=EDGE_CURVE('',#12805,#12806,#7916,.T.);
#16283=EDGE_CURVE('',#12806,#12804,#7917,.T.);
#16284=EDGE_CURVE('',#12800,#12805,#7918,.T.);
#16285=EDGE_CURVE('',#12802,#12806,#7919,.T.);
#16286=EDGE_CURVE('',#12807,#12808,#7920,.T.);
#16287=EDGE_CURVE('',#12807,#12809,#7921,.T.);
#16288=EDGE_CURVE('',#12809,#12810,#7922,.T.);
#16289=EDGE_CURVE('',#12808,#12810,#7923,.T.);
#16290=EDGE_CURVE('',#12811,#12807,#7924,.T.);
#16291=EDGE_CURVE('',#12811,#12812,#7925,.T.);
#16292=EDGE_CURVE('',#12812,#12809,#7926,.T.);
#16293=EDGE_CURVE('',#12813,#12811,#7927,.T.);
#16294=EDGE_CURVE('',#12813,#12814,#7928,.T.);
#16295=EDGE_CURVE('',#12814,#12812,#7929,.T.);
#16296=EDGE_CURVE('',#12808,#12813,#7930,.T.);
#16297=EDGE_CURVE('',#12810,#12814,#7931,.T.);
#16298=EDGE_CURVE('',#12815,#12816,#7932,.T.);
#16299=EDGE_CURVE('',#12815,#12817,#7933,.T.);
#16300=EDGE_CURVE('',#12817,#12818,#7934,.T.);
#16301=EDGE_CURVE('',#12816,#12818,#7935,.T.);
#16302=EDGE_CURVE('',#12819,#12815,#7936,.T.);
#16303=EDGE_CURVE('',#12819,#12820,#7937,.T.);
#16304=EDGE_CURVE('',#12820,#12817,#7938,.T.);
#16305=EDGE_CURVE('',#12821,#12819,#7939,.T.);
#16306=EDGE_CURVE('',#12821,#12822,#7940,.T.);
#16307=EDGE_CURVE('',#12822,#12820,#7941,.T.);
#16308=EDGE_CURVE('',#12816,#12821,#7942,.T.);
#16309=EDGE_CURVE('',#12818,#12822,#7943,.T.);
#16310=EDGE_CURVE('',#12823,#12824,#7944,.T.);
#16311=EDGE_CURVE('',#12823,#12825,#7945,.T.);
#16312=EDGE_CURVE('',#12825,#12826,#7946,.T.);
#16313=EDGE_CURVE('',#12824,#12826,#7947,.T.);
#16314=EDGE_CURVE('',#12827,#12823,#7948,.T.);
#16315=EDGE_CURVE('',#12827,#12828,#7949,.T.);
#16316=EDGE_CURVE('',#12828,#12825,#7950,.T.);
#16317=EDGE_CURVE('',#12829,#12827,#7951,.T.);
#16318=EDGE_CURVE('',#12829,#12830,#7952,.T.);
#16319=EDGE_CURVE('',#12830,#12828,#7953,.T.);
#16320=EDGE_CURVE('',#12824,#12829,#7954,.T.);
#16321=EDGE_CURVE('',#12826,#12830,#7955,.T.);
#16322=EDGE_CURVE('',#12831,#12832,#7956,.T.);
#16323=EDGE_CURVE('',#12831,#12833,#7957,.T.);
#16324=EDGE_CURVE('',#12833,#12834,#7958,.T.);
#16325=EDGE_CURVE('',#12832,#12834,#7959,.T.);
#16326=EDGE_CURVE('',#12835,#12831,#7960,.T.);
#16327=EDGE_CURVE('',#12835,#12836,#7961,.T.);
#16328=EDGE_CURVE('',#12836,#12833,#7962,.T.);
#16329=EDGE_CURVE('',#12837,#12835,#7963,.T.);
#16330=EDGE_CURVE('',#12837,#12838,#7964,.T.);
#16331=EDGE_CURVE('',#12838,#12836,#7965,.T.);
#16332=EDGE_CURVE('',#12832,#12837,#7966,.T.);
#16333=EDGE_CURVE('',#12834,#12838,#7967,.T.);
#16334=EDGE_CURVE('',#12839,#12840,#7968,.T.);
#16335=EDGE_CURVE('',#12839,#12841,#7969,.T.);
#16336=EDGE_CURVE('',#12841,#12842,#7970,.T.);
#16337=EDGE_CURVE('',#12840,#12842,#7971,.T.);
#16338=EDGE_CURVE('',#12843,#12839,#7972,.T.);
#16339=EDGE_CURVE('',#12843,#12844,#7973,.T.);
#16340=EDGE_CURVE('',#12844,#12841,#7974,.T.);
#16341=EDGE_CURVE('',#12845,#12843,#7975,.T.);
#16342=EDGE_CURVE('',#12845,#12846,#7976,.T.);
#16343=EDGE_CURVE('',#12846,#12844,#7977,.T.);
#16344=EDGE_CURVE('',#12840,#12845,#7978,.T.);
#16345=EDGE_CURVE('',#12842,#12846,#7979,.T.);
#16346=EDGE_CURVE('',#12847,#12848,#7980,.T.);
#16347=EDGE_CURVE('',#12847,#12849,#7981,.T.);
#16348=EDGE_CURVE('',#12849,#12850,#7982,.T.);
#16349=EDGE_CURVE('',#12848,#12850,#7983,.T.);
#16350=EDGE_CURVE('',#12851,#12847,#7984,.T.);
#16351=EDGE_CURVE('',#12851,#12852,#7985,.T.);
#16352=EDGE_CURVE('',#12852,#12849,#7986,.T.);
#16353=EDGE_CURVE('',#12853,#12851,#7987,.T.);
#16354=EDGE_CURVE('',#12853,#12854,#7988,.T.);
#16355=EDGE_CURVE('',#12854,#12852,#7989,.T.);
#16356=EDGE_CURVE('',#12848,#12853,#7990,.T.);
#16357=EDGE_CURVE('',#12850,#12854,#7991,.T.);
#16358=EDGE_CURVE('',#12855,#12855,#2457,.T.);
#16359=EDGE_CURVE('',#12855,#12856,#7992,.T.);
#16360=EDGE_CURVE('',#12856,#12856,#2458,.T.);
#16361=EDGE_CURVE('',#12857,#12857,#2459,.T.);
#16362=EDGE_CURVE('',#12858,#12858,#2460,.T.);
#16363=EDGE_CURVE('',#12858,#12857,#7993,.T.);
#16364=EDGE_CURVE('',#12859,#12859,#2461,.T.);
#16365=EDGE_CURVE('',#12859,#12858,#7994,.T.);
#16366=EDGE_CURVE('',#12860,#12860,#2462,.T.);
#16367=EDGE_CURVE('',#12861,#12861,#2463,.T.);
#16368=EDGE_CURVE('',#12861,#12860,#7995,.T.);
#16369=EDGE_CURVE('',#12862,#12862,#2464,.T.);
#16370=EDGE_CURVE('',#12862,#12861,#7996,.T.);
#16371=EDGE_CURVE('',#12863,#12864,#7997,.T.);
#16372=EDGE_CURVE('',#12864,#12865,#880,.T.);
#16373=EDGE_CURVE('',#12865,#12864,#881,.T.);
#16374=EDGE_CURVE('',#12863,#12863,#882,.T.);
#16375=EDGE_CURVE('',#12865,#12866,#7998,.T.);
#16376=EDGE_CURVE('',#12867,#12866,#883,.T.);
#16377=EDGE_CURVE('',#12866,#12867,#884,.T.);
#16378=EDGE_CURVE('',#12868,#12868,#2465,.T.);
#16379=EDGE_CURVE('',#12868,#12869,#7999,.T.);
#16380=EDGE_CURVE('',#12869,#12869,#2466,.T.);
#16381=EDGE_CURVE('',#12870,#12870,#885,.T.);
#16382=EDGE_CURVE('',#12870,#12867,#8000,.T.);
#16383=EDGE_CURVE('',#12871,#12871,#2467,.T.);
#16384=EDGE_CURVE('',#12871,#12871,#2468,.T.);
#16385=EDGE_CURVE('',#12872,#12873,#886,.T.);
#16386=EDGE_CURVE('',#12874,#12872,#887,.T.);
#16387=EDGE_CURVE('',#12873,#12874,#888,.T.);
#16388=EDGE_CURVE('',#12875,#12875,#2469,.T.);
#16389=EDGE_CURVE('',#12875,#12874,#8001,.T.);
#16390=EDGE_CURVE('',#12873,#12876,#8002,.T.);
#16391=EDGE_CURVE('',#12876,#12876,#2470,.T.);
#16392=EDGE_CURVE('',#12877,#12877,#2471,.T.);
#16393=EDGE_CURVE('',#12876,#12877,#8003,.T.);
#16394=EDGE_CURVE('',#12878,#12878,#2472,.T.);
#16395=EDGE_CURVE('',#12879,#12879,#2473,.T.);
#16396=EDGE_CURVE('',#12879,#12878,#8004,.T.);
#16397=EDGE_CURVE('',#12880,#12880,#2474,.T.);
#16398=EDGE_CURVE('',#12880,#12879,#8005,.T.);
#16399=EDGE_CURVE('',#12881,#12881,#2475,.T.);
#16400=EDGE_CURVE('',#12881,#12880,#8006,.T.);
#16401=EDGE_CURVE('',#12882,#12882,#2476,.T.);
#16402=EDGE_CURVE('',#12882,#12868,#8007,.T.);
#16403=EDGE_CURVE('',#12883,#12883,#2477,.T.);
#16404=EDGE_CURVE('',#12883,#12884,#889,.T.);
#16405=EDGE_CURVE('',#12884,#12884,#2478,.T.);
#16406=EDGE_CURVE('',#12885,#12886,#8008,.F.);
#16407=EDGE_CURVE('',#12886,#12887,#8009,.T.);
#16408=EDGE_CURVE('',#12887,#12888,#8010,.F.);
#16409=EDGE_CURVE('',#12888,#12885,#8011,.T.);
#16410=EDGE_CURVE('',#12889,#12886,#8012,.T.);
#16411=EDGE_CURVE('',#12890,#12889,#8013,.T.);
#16412=EDGE_CURVE('',#12887,#12890,#8014,.T.);
#16413=EDGE_CURVE('',#12891,#12890,#8015,.F.);
#16414=EDGE_CURVE('',#12889,#12892,#8016,.F.);
#16415=EDGE_CURVE('',#12892,#12891,#8017,.T.);
#16416=EDGE_CURVE('',#12893,#12894,#8018,.F.);
#16417=EDGE_CURVE('',#12894,#12895,#8019,.T.);
#16418=EDGE_CURVE('',#12895,#12896,#8020,.F.);
#16419=EDGE_CURVE('',#12896,#12893,#8021,.T.);
#16420=EDGE_CURVE('',#12897,#12894,#8022,.T.);
#16421=EDGE_CURVE('',#12898,#12897,#8023,.T.);
#16422=EDGE_CURVE('',#12895,#12898,#8024,.T.);
#16423=EDGE_CURVE('',#12899,#12898,#8025,.F.);
#16424=EDGE_CURVE('',#12897,#12900,#8026,.F.);
#16425=EDGE_CURVE('',#12900,#12899,#8027,.T.);
#16426=EDGE_CURVE('',#12901,#12902,#8028,.T.);
#16427=EDGE_CURVE('',#12902,#12903,#8029,.T.);
#16428=EDGE_CURVE('',#12903,#12904,#8030,.F.);
#16429=EDGE_CURVE('',#12904,#12905,#8031,.T.);
#16430=EDGE_CURVE('',#12905,#12901,#8032,.T.);
#16431=EDGE_CURVE('',#12906,#12904,#8033,.T.);
#16432=EDGE_CURVE('',#12906,#12907,#8034,.T.);
#16433=EDGE_CURVE('',#12907,#12908,#8035,.T.);
#16434=EDGE_CURVE('',#12908,#12909,#8036,.T.);
#16435=EDGE_CURVE('',#12910,#12909,#8037,.T.);
#16436=EDGE_CURVE('',#12911,#12910,#8038,.T.);
#16437=EDGE_CURVE('',#12911,#12905,#8039,.T.);
#16438=EDGE_CURVE('',#12912,#12906,#8040,.T.);
#16439=EDGE_CURVE('',#12907,#12912,#8041,.F.);
#16440=EDGE_CURVE('',#12913,#12910,#8042,.T.);
#16441=EDGE_CURVE('',#12913,#12914,#8043,.T.);
#16442=EDGE_CURVE('',#12914,#12915,#8044,.T.);
#16443=EDGE_CURVE('',#12915,#12911,#8045,.T.);
#16444=EDGE_CURVE('',#12909,#12916,#8046,.T.);
#16445=EDGE_CURVE('',#12908,#12916,#8047,.T.);
#16446=EDGE_CURVE('',#12917,#12900,#8048,.T.);
#16447=EDGE_CURVE('',#12918,#12917,#8049,.F.);
#16448=EDGE_CURVE('',#12918,#12919,#8050,.T.);
#16449=EDGE_CURVE('',#12919,#12914,#8051,.T.);
#16450=EDGE_CURVE('',#12899,#12913,#8052,.T.);
#16451=EDGE_CURVE('',#12920,#12907,#8053,.T.);
#16452=EDGE_CURVE('',#12921,#12920,#8054,.T.);
#16453=EDGE_CURVE('',#12922,#12921,#8055,.T.);
#16454=EDGE_CURVE('',#12923,#12922,#8056,.T.);
#16455=EDGE_CURVE('',#12908,#12923,#8057,.T.);
#16456=EDGE_CURVE('',#12924,#12921,#8058,.T.);
#16457=EDGE_CURVE('',#12920,#12925,#8059,.T.);
#16458=EDGE_CURVE('',#12925,#12926,#8060,.T.);
#16459=EDGE_CURVE('',#12926,#12927,#8061,.T.);
#16460=EDGE_CURVE('',#12927,#12924,#8062,.T.);
#16461=EDGE_CURVE('',#12928,#12924,#8063,.T.);
#16462=EDGE_CURVE('',#12928,#12929,#8064,.T.);
#16463=EDGE_CURVE('',#12930,#12929,#8065,.T.);
#16464=EDGE_CURVE('',#12922,#12930,#8066,.T.);
#16465=EDGE_CURVE('',#12927,#12931,#8067,.T.);
#16466=EDGE_CURVE('',#12931,#12932,#8068,.F.);
#16467=EDGE_CURVE('',#12932,#12928,#8069,.T.);
#16468=EDGE_CURVE('',#12933,#12923,#8070,.T.);
#16469=EDGE_CURVE('',#12930,#12934,#8071,.T.);
#16470=EDGE_CURVE('',#12934,#12935,#8072,.T.);
#16471=EDGE_CURVE('',#12935,#12933,#8073,.T.);
#16472=EDGE_CURVE('',#12936,#12933,#8074,.T.);
#16473=EDGE_CURVE('',#12936,#12916,#8075,.T.);
#16474=EDGE_CURVE('',#12935,#12937,#8076,.T.);
#16475=EDGE_CURVE('',#12937,#12938,#8077,.F.);
#16476=EDGE_CURVE('',#12938,#12936,#8078,.T.);
#16477=EDGE_CURVE('',#12939,#12940,#8079,.T.);
#16478=EDGE_CURVE('',#12941,#12940,#8080,.T.);
#16479=EDGE_CURVE('',#12941,#12942,#8081,.T.);
#16480=EDGE_CURVE('',#12942,#12943,#8082,.T.);
#16481=EDGE_CURVE('',#12943,#12939,#8083,.T.);
#16482=EDGE_CURVE('',#12940,#12944,#8084,.T.);
#16483=EDGE_CURVE('',#12939,#12945,#8085,.T.);
#16484=EDGE_CURVE('',#12946,#12945,#8086,.T.);
#16485=EDGE_CURVE('',#12947,#12946,#8087,.T.);
#16486=EDGE_CURVE('',#12947,#12948,#8088,.T.);
#16487=EDGE_CURVE('',#12948,#12949,#8089,.T.);
#16488=EDGE_CURVE('',#12949,#12944,#8090,.T.);
#16489=EDGE_CURVE('',#12943,#12950,#8091,.T.);
#16490=EDGE_CURVE('',#12945,#12950,#8092,.T.);
#16491=EDGE_CURVE('',#12951,#12888,#8093,.T.);
#16492=EDGE_CURVE('',#12952,#12951,#8094,.F.);
#16493=EDGE_CURVE('',#12952,#12953,#8095,.T.);
#16494=EDGE_CURVE('',#12953,#12942,#8096,.T.);
#16495=EDGE_CURVE('',#12885,#12941,#8097,.T.);
#16496=EDGE_CURVE('',#12954,#12953,#8098,.T.);
#16497=EDGE_CURVE('',#12955,#12954,#8099,.T.);
#16498=EDGE_CURVE('',#12950,#12955,#8100,.T.);
#16499=EDGE_CURVE('',#12955,#12956,#8101,.T.);
#16500=EDGE_CURVE('',#12956,#12946,#8102,.F.);
#16501=EDGE_CURVE('',#12956,#12892,#8103,.T.);
#16502=EDGE_CURVE('',#12954,#12957,#8104,.T.);
#16503=EDGE_CURVE('',#12957,#12958,#8105,.T.);
#16504=EDGE_CURVE('',#12891,#12958,#8106,.T.);
#16505=EDGE_CURVE('',#12959,#12947,#8107,.T.);
#16506=EDGE_CURVE('',#12948,#12959,#8108,.F.);
#16507=EDGE_CURVE('',#12944,#12960,#8109,.T.);
#16508=EDGE_CURVE('',#12949,#12960,#8110,.T.);
#16509=EDGE_CURVE('',#12961,#12948,#8111,.T.);
#16510=EDGE_CURVE('',#12962,#12961,#8112,.T.);
#16511=EDGE_CURVE('',#12963,#12962,#8113,.T.);
#16512=EDGE_CURVE('',#12964,#12963,#8114,.T.);
#16513=EDGE_CURVE('',#12949,#12964,#8115,.T.);
#16514=EDGE_CURVE('',#12965,#12964,#8116,.T.);
#16515=EDGE_CURVE('',#12963,#12966,#8117,.T.);
#16516=EDGE_CURVE('',#12966,#12967,#8118,.T.);
#16517=EDGE_CURVE('',#12967,#12968,#8119,.T.);
#16518=EDGE_CURVE('',#12968,#12965,#8120,.T.);
#16519=EDGE_CURVE('',#12966,#12969,#8121,.T.);
#16520=EDGE_CURVE('',#12969,#12970,#8122,.T.);
#16521=EDGE_CURVE('',#12970,#12971,#8123,.F.);
#16522=EDGE_CURVE('',#12971,#12967,#8124,.T.);
#16523=EDGE_CURVE('',#12972,#12962,#8125,.T.);
#16524=EDGE_CURVE('',#12973,#12972,#8126,.T.);
#16525=EDGE_CURVE('',#12973,#12969,#8127,.T.);
#16526=EDGE_CURVE('',#12961,#12974,#8128,.T.);
#16527=EDGE_CURVE('',#12974,#12975,#8129,.T.);
#16528=EDGE_CURVE('',#12975,#12976,#8130,.T.);
#16529=EDGE_CURVE('',#12976,#12972,#8131,.T.);
#16530=EDGE_CURVE('',#12976,#12977,#8132,.T.);
#16531=EDGE_CURVE('',#12977,#12978,#8133,.F.);
#16532=EDGE_CURVE('',#12978,#12973,#8134,.T.);
#16533=EDGE_CURVE('',#12979,#12980,#8135,.T.);
#16534=EDGE_CURVE('',#12980,#12981,#2479,.T.);
#16535=EDGE_CURVE('',#12981,#12982,#8136,.T.);
#16536=EDGE_CURVE('',#12982,#12979,#2480,.T.);
#16537=EDGE_CURVE('',#12983,#12984,#8137,.T.);
#16538=EDGE_CURVE('',#12984,#12980,#8138,.T.);
#16539=EDGE_CURVE('',#12979,#12983,#8139,.T.);
#16540=EDGE_CURVE('',#12985,#12986,#8140,.T.);
#16541=EDGE_CURVE('',#12986,#12984,#2481,.T.);
#16542=EDGE_CURVE('',#12983,#12985,#2482,.T.);
#16543=EDGE_CURVE('',#12987,#12988,#8141,.T.);
#16544=EDGE_CURVE('',#12988,#12986,#8142,.T.);
#16545=EDGE_CURVE('',#12985,#12987,#8143,.T.);
#16546=EDGE_CURVE('',#12989,#12990,#8144,.T.);
#16547=EDGE_CURVE('',#12990,#12988,#2483,.T.);
#16548=EDGE_CURVE('',#12987,#12989,#2484,.T.);
#16549=EDGE_CURVE('',#12991,#12992,#8145,.T.);
#16550=EDGE_CURVE('',#12992,#12990,#8146,.T.);
#16551=EDGE_CURVE('',#12989,#12991,#8147,.T.);
#16552=EDGE_CURVE('',#12993,#12994,#8148,.T.);
#16553=EDGE_CURVE('',#12994,#12992,#2485,.T.);
#16554=EDGE_CURVE('',#12991,#12993,#2486,.T.);
#16555=EDGE_CURVE('',#12981,#12994,#8149,.T.);
#16556=EDGE_CURVE('',#12993,#12982,#8150,.T.);
#16557=EDGE_CURVE('',#12995,#12992,#8151,.T.);
#16558=EDGE_CURVE('',#12996,#12995,#8152,.T.);
#16559=EDGE_CURVE('',#12990,#12996,#8153,.T.);
#16560=EDGE_CURVE('',#12994,#12997,#8154,.T.);
#16561=EDGE_CURVE('',#12995,#12997,#2487,.T.);
#16562=EDGE_CURVE('',#12998,#12981,#8155,.T.);
#16563=EDGE_CURVE('',#12997,#12998,#8156,.T.);
#16564=EDGE_CURVE('',#12980,#12999,#8157,.T.);
#16565=EDGE_CURVE('',#12998,#12999,#2488,.T.);
#16566=EDGE_CURVE('',#13000,#13000,#2489,.T.);
#16567=EDGE_CURVE('',#13001,#13001,#2490,.T.);
#16568=EDGE_CURVE('',#13002,#12975,#8158,.T.);
#16569=EDGE_CURVE('',#12977,#13002,#8159,.T.);
#16570=EDGE_CURVE('',#13003,#12971,#8160,.T.);
#16571=EDGE_CURVE('',#12968,#13003,#8161,.T.);
#16572=EDGE_CURVE('',#12974,#13004,#8162,.T.);
#16573=EDGE_CURVE('',#13004,#13005,#8163,.T.);
#16574=EDGE_CURVE('',#13005,#13002,#8164,.F.);
#16575=EDGE_CURVE('',#12959,#13004,#8165,.T.);
#16576=EDGE_CURVE('',#13006,#12960,#8166,.T.);
#16577=EDGE_CURVE('',#13007,#13006,#8167,.T.);
#16578=EDGE_CURVE('',#13005,#13007,#8168,.T.);
#16579=EDGE_CURVE('',#13008,#13008,#2491,.T.);
#16580=EDGE_CURVE('',#13009,#13009,#2492,.T.);
#16581=EDGE_CURVE('',#13003,#13007,#8169,.F.);
#16582=EDGE_CURVE('',#13006,#12965,#8170,.T.);
#16583=EDGE_CURVE('',#12925,#13010,#8171,.T.);
#16584=EDGE_CURVE('',#13010,#13011,#8172,.T.);
#16585=EDGE_CURVE('',#13011,#13012,#8173,.F.);
#16586=EDGE_CURVE('',#13012,#12926,#8174,.T.);
#16587=EDGE_CURVE('',#12912,#13010,#8175,.T.);
#16588=EDGE_CURVE('',#12903,#12896,#8176,.T.);
#16589=EDGE_CURVE('',#13011,#12938,#8177,.T.);
#16590=EDGE_CURVE('',#13013,#13013,#2493,.T.);
#16591=EDGE_CURVE('',#13014,#13014,#2494,.T.);
#16592=EDGE_CURVE('',#13015,#12934,#8178,.T.);
#16593=EDGE_CURVE('',#12937,#13015,#8179,.T.);
#16594=EDGE_CURVE('',#12929,#13016,#8180,.T.);
#16595=EDGE_CURVE('',#13016,#13015,#8181,.F.);
#16596=EDGE_CURVE('',#12931,#13012,#8182,.T.);
#16597=EDGE_CURVE('',#13017,#13017,#2495,.T.);
#16598=EDGE_CURVE('',#13017,#13018,#8183,.T.);
#16599=EDGE_CURVE('',#13018,#13018,#2496,.T.);
#16600=EDGE_CURVE('',#13019,#13019,#2497,.T.);
#16601=EDGE_CURVE('',#13019,#13018,#8184,.T.);
#16602=EDGE_CURVE('',#13016,#12932,#8185,.T.);
#16603=EDGE_CURVE('',#13020,#13020,#2498,.T.);
#16604=EDGE_CURVE('',#13013,#13019,#8186,.T.);
#16605=EDGE_CURVE('',#13008,#13021,#8187,.T.);
#16606=EDGE_CURVE('',#13021,#13021,#2499,.T.);
#16607=EDGE_CURVE('',#13022,#13022,#2500,.T.);
#16608=EDGE_CURVE('',#13022,#13021,#8188,.T.);
#16609=EDGE_CURVE('',#13023,#13023,#2501,.T.);
#16610=EDGE_CURVE('',#13023,#13022,#8189,.T.);
#16611=EDGE_CURVE('',#12970,#12978,#8190,.T.);
#16612=EDGE_CURVE('',#13024,#13024,#2502,.T.);
#16613=EDGE_CURVE('',#13020,#13025,#8191,.T.);
#16614=EDGE_CURVE('',#13025,#13025,#2503,.T.);
#16615=EDGE_CURVE('',#13026,#13026,#2504,.T.);
#16616=EDGE_CURVE('',#13026,#13025,#8192,.T.);
#16617=EDGE_CURVE('',#13014,#13026,#8193,.T.);
#16618=EDGE_CURVE('',#13009,#13027,#8194,.T.);
#16619=EDGE_CURVE('',#13027,#13027,#2505,.T.);
#16620=EDGE_CURVE('',#13028,#13028,#2506,.T.);
#16621=EDGE_CURVE('',#13028,#13027,#8195,.T.);
#16622=EDGE_CURVE('',#13024,#13028,#8196,.T.);
#16623=EDGE_CURVE('',#13000,#13029,#8197,.T.);
#16624=EDGE_CURVE('',#13029,#13029,#2507,.T.);
#16625=EDGE_CURVE('',#13029,#13030,#8198,.T.);
#16626=EDGE_CURVE('',#13030,#13030,#2508,.T.);
#16627=EDGE_CURVE('',#13001,#13031,#8199,.T.);
#16628=EDGE_CURVE('',#13031,#13031,#2509,.T.);
#16629=EDGE_CURVE('',#13031,#13032,#8200,.T.);
#16630=EDGE_CURVE('',#13032,#13032,#2510,.T.);
#16631=EDGE_CURVE('',#12917,#13033,#8201,.T.);
#16632=EDGE_CURVE('',#13033,#13034,#8202,.T.);
#16633=EDGE_CURVE('',#13034,#12918,#8203,.T.);
#16634=EDGE_CURVE('',#13035,#13036,#8204,.T.);
#16635=EDGE_CURVE('',#13036,#13034,#2511,.T.);
#16636=EDGE_CURVE('',#13033,#13035,#2512,.T.);
#16637=EDGE_CURVE('',#13037,#13038,#8205,.T.);
#16638=EDGE_CURVE('',#13038,#13036,#8206,.T.);
#16639=EDGE_CURVE('',#13035,#13037,#8207,.T.);
#16640=EDGE_CURVE('',#13039,#13040,#8208,.T.);
#16641=EDGE_CURVE('',#13040,#13038,#2513,.T.);
#16642=EDGE_CURVE('',#13037,#13039,#2514,.T.);
#16643=EDGE_CURVE('',#12957,#13040,#8209,.T.);
#16644=EDGE_CURVE('',#13039,#12958,#8210,.T.);
#16645=EDGE_CURVE('',#12893,#13041,#8211,.T.);
#16646=EDGE_CURVE('',#13042,#13041,#8212,.T.);
#16647=EDGE_CURVE('',#13043,#13042,#2515,.T.);
#16648=EDGE_CURVE('',#13044,#13043,#8213,.T.);
#16649=EDGE_CURVE('',#13045,#13044,#2516,.T.);
#16650=EDGE_CURVE('',#12951,#13045,#8214,.T.);
#16651=EDGE_CURVE('',#13046,#13046,#2517,.T.);
#16652=EDGE_CURVE('',#13047,#13047,#2518,.T.);
#16653=EDGE_CURVE('',#13045,#13048,#8215,.T.);
#16654=EDGE_CURVE('',#13048,#12952,#8216,.T.);
#16655=EDGE_CURVE('',#13044,#13049,#8217,.T.);
#16656=EDGE_CURVE('',#13049,#13048,#2519,.T.);
#16657=EDGE_CURVE('',#13043,#13050,#8218,.T.);
#16658=EDGE_CURVE('',#13050,#13049,#8219,.T.);
#16659=EDGE_CURVE('',#13042,#13051,#8220,.T.);
#16660=EDGE_CURVE('',#13051,#13050,#2520,.T.);
#16661=EDGE_CURVE('',#13052,#13041,#8221,.T.);
#16662=EDGE_CURVE('',#13052,#13051,#8222,.T.);
#16663=EDGE_CURVE('',#13047,#13032,#8223,.T.);
#16664=EDGE_CURVE('',#13046,#13030,#8224,.T.);
#16665=EDGE_CURVE('',#12901,#12915,#8225,.T.);
#16666=EDGE_CURVE('',#13053,#12919,#8226,.T.);
#16667=EDGE_CURVE('',#12902,#13053,#8227,.T.);
#16668=EDGE_CURVE('',#13053,#13052,#8228,.T.);
#16669=EDGE_CURVE('',#13036,#12998,#8229,.T.);
#16670=EDGE_CURVE('',#12999,#13034,#8230,.T.);
#16671=EDGE_CURVE('',#13038,#12997,#8231,.T.);
#16672=EDGE_CURVE('',#13040,#12995,#8232,.T.);
#16673=EDGE_CURVE('',#13048,#12996,#8233,.T.);
#16674=EDGE_CURVE('',#13049,#13054,#8234,.T.);
#16675=EDGE_CURVE('',#13054,#12996,#2521,.T.);
#16676=EDGE_CURVE('',#13050,#13055,#8235,.T.);
#16677=EDGE_CURVE('',#13055,#13054,#8236,.T.);
#16678=EDGE_CURVE('',#13051,#13056,#8237,.T.);
#16679=EDGE_CURVE('',#13056,#13055,#2522,.T.);
#16680=EDGE_CURVE('',#12999,#13056,#8238,.T.);
#16681=EDGE_CURVE('',#13054,#12988,#8239,.T.);
#16682=EDGE_CURVE('',#12986,#13055,#8240,.T.);
#16683=EDGE_CURVE('',#13056,#12984,#8241,.T.);
#16684=EDGE_CURVE('',#13057,#13057,#2523,.T.);
#16685=EDGE_CURVE('',#13057,#13057,#2524,.T.);
#16686=EDGE_CURVE('',#13058,#13059,#890,.T.);
#16687=EDGE_CURVE('',#13060,#13058,#891,.T.);
#16688=EDGE_CURVE('',#13059,#13060,#892,.T.);
#16689=EDGE_CURVE('',#13061,#13061,#893,.T.);
#16690=EDGE_CURVE('',#13062,#13063,#894,.T.);
#16691=EDGE_CURVE('',#13064,#13062,#895,.T.);
#16692=EDGE_CURVE('',#13065,#13064,#896,.T.);
#16693=EDGE_CURVE('',#13066,#13065,#897,.T.);
#16694=EDGE_CURVE('',#13067,#13066,#898,.T.);
#16695=EDGE_CURVE('',#13063,#13067,#899,.T.);
#16696=EDGE_CURVE('',#13066,#13067,#2525,.T.);
#16697=EDGE_CURVE('',#13064,#13062,#2526,.T.);
#16698=EDGE_CURVE('',#13060,#13058,#2527,.T.);
#16699=EDGE_CURVE('',#13068,#13068,#2528,.T.);
#16700=EDGE_CURVE('',#13068,#13068,#2529,.T.);
#16701=EDGE_CURVE('',#13069,#13070,#2530,.T.);
#16702=EDGE_CURVE('',#13071,#13070,#900,.T.);
#16703=EDGE_CURVE('',#13072,#13071,#901,.T.);
#16704=EDGE_CURVE('',#13073,#13072,#902,.T.);
#16705=EDGE_CURVE('',#13074,#13073,#903,.T.);
#16706=EDGE_CURVE('',#13075,#13074,#904,.T.);
#16707=EDGE_CURVE('',#13069,#13075,#905,.T.);
#16708=EDGE_CURVE('',#13076,#13076,#906,.T.);
#16709=EDGE_CURVE('',#13072,#13077,#8242,.T.);
#16710=EDGE_CURVE('',#13077,#13073,#2531,.T.);
#16711=EDGE_CURVE('',#13077,#13071,#2532,.T.);
#16712=EDGE_CURVE('',#13077,#13075,#907,.T.);
#16713=EDGE_CURVE('',#13059,#13074,#908,.T.);
#16714=EDGE_CURVE('',#13078,#13079,#8243,.T.);
#16715=EDGE_CURVE('',#13078,#13080,#909,.T.);
#16716=EDGE_CURVE('',#13080,#13081,#2533,.T.);
#16717=EDGE_CURVE('',#13081,#13079,#910,.T.);
#16718=EDGE_CURVE('',#13082,#13083,#8244,.T.);
#16719=EDGE_CURVE('',#13082,#13078,#911,.T.);
#16720=EDGE_CURVE('',#13079,#13083,#912,.T.);
#16721=EDGE_CURVE('',#13084,#13085,#8245,.T.);
#16722=EDGE_CURVE('',#13084,#13082,#913,.T.);
#16723=EDGE_CURVE('',#13083,#13085,#914,.T.);
#16724=EDGE_CURVE('',#13086,#13087,#8246,.T.);
#16725=EDGE_CURVE('',#13086,#13084,#915,.T.);
#16726=EDGE_CURVE('',#13085,#13087,#916,.T.);
#16727=EDGE_CURVE('',#13088,#13089,#8247,.T.);
#16728=EDGE_CURVE('',#13088,#13086,#917,.T.);
#16729=EDGE_CURVE('',#13087,#13089,#918,.T.);
#16730=EDGE_CURVE('',#13090,#13091,#8248,.T.);
#16731=EDGE_CURVE('',#13090,#13088,#919,.T.);
#16732=EDGE_CURVE('',#13089,#13091,#920,.T.);
#16733=EDGE_CURVE('',#13092,#13093,#8249,.T.);
#16734=EDGE_CURVE('',#13092,#13090,#921,.T.);
#16735=EDGE_CURVE('',#13091,#13093,#922,.T.);
#16736=EDGE_CURVE('',#13094,#13095,#8250,.T.);
#16737=EDGE_CURVE('',#13094,#13092,#923,.T.);
#16738=EDGE_CURVE('',#13093,#13095,#924,.T.);
#16739=EDGE_CURVE('',#13096,#13097,#8251,.T.);
#16740=EDGE_CURVE('',#13096,#13094,#925,.T.);
#16741=EDGE_CURVE('',#13095,#13097,#926,.T.);
#16742=EDGE_CURVE('',#13098,#13099,#8252,.T.);
#16743=EDGE_CURVE('',#13098,#13096,#927,.T.);
#16744=EDGE_CURVE('',#13097,#13099,#928,.T.);
#16745=EDGE_CURVE('',#13100,#13101,#8253,.T.);
#16746=EDGE_CURVE('',#13100,#13098,#929,.T.);
#16747=EDGE_CURVE('',#13099,#13101,#930,.T.);
#16748=EDGE_CURVE('',#13102,#13103,#8254,.T.);
#16749=EDGE_CURVE('',#13102,#13104,#931,.T.);
#16750=EDGE_CURVE('',#13104,#13105,#2534,.T.);
#16751=EDGE_CURVE('',#13103,#13105,#932,.T.);
#16752=EDGE_CURVE('',#13106,#13107,#8255,.T.);
#16753=EDGE_CURVE('',#13106,#13102,#933,.T.);
#16754=EDGE_CURVE('',#13107,#13103,#934,.T.);
#16755=EDGE_CURVE('',#13108,#13109,#8256,.T.);
#16756=EDGE_CURVE('',#13108,#13106,#935,.T.);
#16757=EDGE_CURVE('',#13109,#13107,#936,.T.);
#16758=EDGE_CURVE('',#13110,#13111,#8257,.T.);
#16759=EDGE_CURVE('',#13110,#13108,#937,.T.);
#16760=EDGE_CURVE('',#13111,#13109,#938,.T.);
#16761=EDGE_CURVE('',#13112,#13113,#8258,.T.);
#16762=EDGE_CURVE('',#13112,#13110,#939,.T.);
#16763=EDGE_CURVE('',#13113,#13111,#940,.T.);
#16764=EDGE_CURVE('',#13114,#13115,#8259,.T.);
#16765=EDGE_CURVE('',#13114,#13112,#941,.T.);
#16766=EDGE_CURVE('',#13115,#13113,#942,.T.);
#16767=EDGE_CURVE('',#13116,#13117,#8260,.T.);
#16768=EDGE_CURVE('',#13116,#13114,#943,.T.);
#16769=EDGE_CURVE('',#13117,#13115,#944,.T.);
#16770=EDGE_CURVE('',#13118,#13119,#8261,.T.);
#16771=EDGE_CURVE('',#13118,#13116,#945,.T.);
#16772=EDGE_CURVE('',#13119,#13117,#946,.T.);
#16773=EDGE_CURVE('',#13120,#13121,#8262,.T.);
#16774=EDGE_CURVE('',#13120,#13118,#947,.T.);
#16775=EDGE_CURVE('',#13121,#13119,#948,.T.);
#16776=EDGE_CURVE('',#13122,#13123,#8263,.T.);
#16777=EDGE_CURVE('',#13122,#13120,#949,.T.);
#16778=EDGE_CURVE('',#13123,#13121,#950,.T.);
#16779=EDGE_CURVE('',#13124,#13125,#8264,.T.);
#16780=EDGE_CURVE('',#13124,#13122,#951,.T.);
#16781=EDGE_CURVE('',#13125,#13123,#952,.T.);
#16782=EDGE_CURVE('',#13126,#13127,#2535,.T.);
#16783=EDGE_CURVE('',#13128,#13126,#953,.T.);
#16784=EDGE_CURVE('',#13129,#13128,#954,.T.);
#16785=EDGE_CURVE('',#13130,#13129,#955,.T.);
#16786=EDGE_CURVE('',#13131,#13130,#956,.T.);
#16787=EDGE_CURVE('',#13132,#13131,#957,.T.);
#16788=EDGE_CURVE('',#13127,#13132,#2536,.T.);
#16789=EDGE_CURVE('',#13127,#13127,#2537,.T.);
#16790=EDGE_CURVE('',#13133,#13132,#958,.T.);
#16791=EDGE_CURVE('',#13134,#13133,#959,.T.);
#16792=EDGE_CURVE('',#13135,#13134,#960,.T.);
#16793=EDGE_CURVE('',#13136,#13135,#961,.T.);
#16794=EDGE_CURVE('',#13126,#13136,#962,.T.);
#16795=EDGE_CURVE('',#13137,#13137,#2538,.T.);
#16796=EDGE_CURVE('',#13129,#13135,#2539,.T.);
#16797=EDGE_CURVE('',#13134,#13130,#2540,.T.);
#16798=EDGE_CURVE('',#13136,#13128,#2541,.T.);
#16799=EDGE_CURVE('',#13131,#13133,#2542,.T.);
#16800=EDGE_CURVE('',#13138,#13138,#2543,.T.);
#16801=EDGE_CURVE('',#13105,#13139,#963,.T.);
#16802=EDGE_CURVE('',#13140,#13104,#964,.T.);
#16803=EDGE_CURVE('',#13139,#13140,#2544,.T.);
#16804=EDGE_CURVE('',#13141,#13141,#2545,.T.);
#16805=EDGE_CURVE('',#13141,#13138,#8265,.T.);
#16806=EDGE_CURVE('',#13137,#13141,#8266,.T.);
#16807=EDGE_CURVE('',#13142,#13124,#965,.T.);
#16808=EDGE_CURVE('',#13080,#13142,#966,.T.);
#16809=EDGE_CURVE('',#13140,#13100,#967,.T.);
#16810=EDGE_CURVE('',#13143,#13125,#968,.T.);
#16811=EDGE_CURVE('',#13142,#13143,#2546,.T.);
#16812=EDGE_CURVE('',#13101,#13139,#969,.T.);
#16813=EDGE_CURVE('',#13143,#13081,#970,.T.);
#16814=EDGE_CURVE('',#13081,#13144,#2547,.T.);
#16815=EDGE_CURVE('',#13144,#13080,#2548,.T.);
#16816=EDGE_CURVE('',#13145,#13145,#2549,.T.);
#16817=EDGE_CURVE('',#13144,#13145,#8267,.T.);
#16818=EDGE_CURVE('',#13146,#13147,#8268,.T.);
#16819=EDGE_CURVE('',#13147,#13148,#8269,.T.);
#16820=EDGE_CURVE('',#13148,#13149,#8270,.T.);
#16821=EDGE_CURVE('',#13149,#13150,#8271,.T.);
#16822=EDGE_CURVE('',#13150,#13151,#8272,.T.);
#16823=EDGE_CURVE('',#13151,#13146,#8273,.T.);
#16824=EDGE_CURVE('',#13152,#13150,#8274,.T.);
#16825=EDGE_CURVE('',#13153,#13152,#8275,.T.);
#16826=EDGE_CURVE('',#13151,#13153,#8276,.T.);
#16827=EDGE_CURVE('',#13154,#13149,#8277,.T.);
#16828=EDGE_CURVE('',#13154,#13155,#8278,.T.);
#16829=EDGE_CURVE('',#13156,#13155,#8279,.T.);
#16830=EDGE_CURVE('',#13152,#13156,#8280,.T.);
#16831=EDGE_CURVE('',#13148,#13157,#8281,.T.);
#16832=EDGE_CURVE('',#13157,#13158,#8282,.T.);
#16833=EDGE_CURVE('',#13158,#13159,#8283,.T.);
#16834=EDGE_CURVE('',#13159,#13154,#8284,.T.);
#16835=EDGE_CURVE('',#13160,#13147,#8285,.T.);
#16836=EDGE_CURVE('',#13161,#13160,#8286,.T.);
#16837=EDGE_CURVE('',#13162,#13161,#8287,.T.);
#16838=EDGE_CURVE('',#13163,#13162,#8288,.T.);
#16839=EDGE_CURVE('',#13164,#13163,#8289,.T.);
#16840=EDGE_CURVE('',#13165,#13164,#8290,.T.);
#16841=EDGE_CURVE('',#13166,#13165,#8291,.T.);
#16842=EDGE_CURVE('',#13157,#13166,#8292,.T.);
#16843=EDGE_CURVE('',#13167,#13159,#8293,.T.);
#16844=EDGE_CURVE('',#13155,#13167,#8294,.T.);
#16845=EDGE_CURVE('',#13168,#13166,#8295,.T.);
#16846=EDGE_CURVE('',#13165,#13169,#8296,.F.);
#16847=EDGE_CURVE('',#13169,#13170,#8297,.T.);
#16848=EDGE_CURVE('',#13170,#13168,#8298,.T.);
#16849=EDGE_CURVE('',#13171,#13168,#8299,.T.);
#16850=EDGE_CURVE('',#13171,#13172,#8300,.T.);
#16851=EDGE_CURVE('',#13172,#13158,#8301,.T.);
#16852=EDGE_CURVE('',#13170,#13173,#8302,.T.);
#16853=EDGE_CURVE('',#13173,#13174,#8303,.T.);
#16854=EDGE_CURVE('',#13174,#13171,#8304,.T.);
#16855=EDGE_CURVE('',#13175,#13176,#8305,.T.);
#16856=EDGE_CURVE('',#13176,#13177,#8306,.T.);
#16857=EDGE_CURVE('',#13177,#13178,#8307,.T.);
#16858=EDGE_CURVE('',#13178,#13179,#8308,.T.);
#16859=EDGE_CURVE('',#13179,#13180,#8309,.T.);
#16860=EDGE_CURVE('',#13180,#13175,#8310,.T.);
#16861=EDGE_CURVE('',#13181,#13176,#8311,.T.);
#16862=EDGE_CURVE('',#13182,#13181,#8312,.T.);
#16863=EDGE_CURVE('',#13177,#13182,#8313,.T.);
#16864=EDGE_CURVE('',#13164,#13175,#8314,.T.);
#16865=EDGE_CURVE('',#13163,#13183,#8315,.T.);
#16866=EDGE_CURVE('',#13183,#13181,#8316,.T.);
#16867=EDGE_CURVE('',#13180,#13169,#8317,.T.);
#16868=EDGE_CURVE('',#13184,#13179,#8318,.T.);
#16869=EDGE_CURVE('',#13184,#13169,#8319,.T.);
#16870=EDGE_CURVE('',#13185,#13183,#8320,.T.);
#16871=EDGE_CURVE('',#13185,#13186,#8321,.T.);
#16872=EDGE_CURVE('',#13187,#13186,#8322,.T.);
#16873=EDGE_CURVE('',#13182,#13187,#8323,.T.);
#16874=EDGE_CURVE('',#13187,#13188,#8324,.T.);
#16875=EDGE_CURVE('',#13188,#13189,#8325,.T.);
#16876=EDGE_CURVE('',#13189,#13178,#8326,.T.);
#16877=EDGE_CURVE('',#13189,#13190,#8327,.T.);
#16878=EDGE_CURVE('',#13190,#13184,#8328,.T.);
#16879=EDGE_CURVE('',#13191,#13173,#8329,.T.);
#16880=EDGE_CURVE('',#13174,#13191,#8330,.T.);
#16881=EDGE_CURVE('',#13190,#13191,#8331,.T.);
#16882=EDGE_CURVE('',#13173,#13184,#8332,.T.);
#16883=EDGE_CURVE('',#13192,#13193,#8333,.T.);
#16884=EDGE_CURVE('',#13193,#13174,#8334,.T.);
#16885=EDGE_CURVE('',#13191,#13194,#8335,.T.);
#16886=EDGE_CURVE('',#13194,#13192,#8336,.T.);
#16887=EDGE_CURVE('',#13186,#13195,#8337,.T.);
#16888=EDGE_CURVE('',#13195,#13196,#8338,.T.);
#16889=EDGE_CURVE('',#13196,#13188,#8339,.T.);
#16890=EDGE_CURVE('',#13194,#13197,#8340,.T.);
#16891=EDGE_CURVE('',#13197,#13156,#8341,.T.);
#16892=EDGE_CURVE('',#13167,#13192,#8342,.T.);
#16893=EDGE_CURVE('',#13197,#13198,#8343,.T.);
#16894=EDGE_CURVE('',#13198,#13199,#8344,.T.);
#16895=EDGE_CURVE('',#13199,#13153,#8345,.T.);
#16896=EDGE_CURVE('',#13200,#13199,#8346,.T.);
#16897=EDGE_CURVE('',#13200,#13201,#8347,.T.);
#16898=EDGE_CURVE('',#13146,#13201,#8348,.T.);
#16899=EDGE_CURVE('',#13198,#13202,#8349,.T.);
#16900=EDGE_CURVE('',#13202,#13203,#8350,.T.);
#16901=EDGE_CURVE('',#13203,#13200,#8351,.T.);
#16902=EDGE_CURVE('',#13204,#13205,#8352,.T.);
#16903=EDGE_CURVE('',#13162,#13204,#8353,.T.);
#16904=EDGE_CURVE('',#13205,#13162,#8354,.T.);
#16905=EDGE_CURVE('',#13204,#13185,#8355,.T.);
#16906=EDGE_CURVE('',#13206,#13195,#8356,.T.);
#16907=EDGE_CURVE('',#13196,#13206,#8357,.T.);
#16908=EDGE_CURVE('',#13195,#13204,#8358,.T.);
#16909=EDGE_CURVE('',#13205,#13206,#8359,.T.);
#16910=EDGE_CURVE('',#13207,#13208,#8360,.T.);
#16911=EDGE_CURVE('',#13160,#13207,#8361,.T.);
#16912=EDGE_CURVE('',#13208,#13160,#8362,.T.);
#16913=EDGE_CURVE('',#13207,#13209,#8363,.T.);
#16914=EDGE_CURVE('',#13209,#13161,#8364,.T.);
#16915=EDGE_CURVE('',#13201,#13208,#8365,.T.);
#16916=EDGE_CURVE('',#13203,#13210,#8366,.T.);
#16917=EDGE_CURVE('',#13210,#13202,#8367,.T.);
#16918=EDGE_CURVE('',#13211,#13210,#8368,.T.);
#16919=EDGE_CURVE('',#13202,#13212,#8369,.T.);
#16920=EDGE_CURVE('',#13212,#13211,#8370,.T.);
#16921=EDGE_CURVE('',#13208,#13203,#8371,.T.);
#16922=EDGE_CURVE('',#13210,#13207,#8372,.T.);
#16923=EDGE_CURVE('',#13212,#13196,#8373,.T.);
#16924=EDGE_CURVE('',#13206,#13211,#8374,.T.);
#16925=EDGE_CURVE('',#13209,#13205,#8375,.T.);
#16926=EDGE_CURVE('',#13211,#13209,#8376,.T.);
#16927=EDGE_CURVE('',#13172,#13193,#8377,.T.);
#16928=EDGE_CURVE('',#13213,#13214,#8378,.T.);
#16929=EDGE_CURVE('',#13213,#13215,#971,.T.);
#16930=EDGE_CURVE('',#13215,#13216,#2550,.T.);
#16931=EDGE_CURVE('',#13216,#13214,#972,.T.);
#16932=EDGE_CURVE('',#13217,#13218,#8379,.T.);
#16933=EDGE_CURVE('',#13217,#13213,#973,.T.);
#16934=EDGE_CURVE('',#13214,#13218,#974,.T.);
#16935=EDGE_CURVE('',#13219,#13220,#8380,.T.);
#16936=EDGE_CURVE('',#13219,#13217,#975,.T.);
#16937=EDGE_CURVE('',#13218,#13220,#976,.T.);
#16938=EDGE_CURVE('',#13221,#13222,#8381,.T.);
#16939=EDGE_CURVE('',#13221,#13219,#977,.T.);
#16940=EDGE_CURVE('',#13220,#13222,#978,.T.);
#16941=EDGE_CURVE('',#13223,#13224,#8382,.T.);
#16942=EDGE_CURVE('',#13223,#13221,#979,.T.);
#16943=EDGE_CURVE('',#13222,#13224,#980,.T.);
#16944=EDGE_CURVE('',#13225,#13226,#8383,.T.);
#16945=EDGE_CURVE('',#13225,#13223,#981,.T.);
#16946=EDGE_CURVE('',#13224,#13226,#982,.T.);
#16947=EDGE_CURVE('',#13227,#13228,#8384,.T.);
#16948=EDGE_CURVE('',#13227,#13225,#983,.T.);
#16949=EDGE_CURVE('',#13226,#13228,#984,.T.);
#16950=EDGE_CURVE('',#13229,#13230,#8385,.T.);
#16951=EDGE_CURVE('',#13229,#13227,#985,.T.);
#16952=EDGE_CURVE('',#13228,#13230,#986,.T.);
#16953=EDGE_CURVE('',#13231,#13232,#8386,.T.);
#16954=EDGE_CURVE('',#13231,#13229,#987,.T.);
#16955=EDGE_CURVE('',#13230,#13232,#988,.T.);
#16956=EDGE_CURVE('',#13233,#13234,#8387,.T.);
#16957=EDGE_CURVE('',#13233,#13231,#989,.T.);
#16958=EDGE_CURVE('',#13232,#13234,#990,.T.);
#16959=EDGE_CURVE('',#13235,#13236,#8388,.T.);
#16960=EDGE_CURVE('',#13235,#13233,#991,.T.);
#16961=EDGE_CURVE('',#13234,#13236,#992,.T.);
#16962=EDGE_CURVE('',#13237,#13238,#8389,.T.);
#16963=EDGE_CURVE('',#13237,#13235,#993,.T.);
#16964=EDGE_CURVE('',#13236,#13238,#994,.T.);
#16965=EDGE_CURVE('',#13239,#13240,#8390,.T.);
#16966=EDGE_CURVE('',#13239,#13237,#995,.T.);
#16967=EDGE_CURVE('',#13238,#13240,#996,.T.);
#16968=EDGE_CURVE('',#13241,#13242,#8391,.T.);
#16969=EDGE_CURVE('',#13241,#13239,#997,.T.);
#16970=EDGE_CURVE('',#13240,#13242,#998,.T.);
#16971=EDGE_CURVE('',#13243,#13244,#8392,.T.);
#16972=EDGE_CURVE('',#13243,#13241,#999,.T.);
#16973=EDGE_CURVE('',#13242,#13244,#1000,.T.);
#16974=EDGE_CURVE('',#13245,#13246,#8393,.T.);
#16975=EDGE_CURVE('',#13245,#13243,#1001,.T.);
#16976=EDGE_CURVE('',#13244,#13246,#1002,.T.);
#16977=EDGE_CURVE('',#13247,#13248,#8394,.T.);
#16978=EDGE_CURVE('',#13247,#13245,#1003,.T.);
#16979=EDGE_CURVE('',#13246,#13248,#1004,.T.);
#16980=EDGE_CURVE('',#13249,#13250,#8395,.T.);
#16981=EDGE_CURVE('',#13249,#13247,#1005,.T.);
#16982=EDGE_CURVE('',#13248,#13250,#1006,.T.);
#16983=EDGE_CURVE('',#13251,#13252,#8396,.T.);
#16984=EDGE_CURVE('',#13251,#13249,#1007,.T.);
#16985=EDGE_CURVE('',#13250,#13252,#1008,.T.);
#16986=EDGE_CURVE('',#13253,#13254,#8397,.T.);
#16987=EDGE_CURVE('',#13253,#13251,#1009,.T.);
#16988=EDGE_CURVE('',#13252,#13254,#1010,.T.);
#16989=EDGE_CURVE('',#13255,#13256,#8398,.T.);
#16990=EDGE_CURVE('',#13255,#13253,#1011,.T.);
#16991=EDGE_CURVE('',#13254,#13256,#1012,.T.);
#16992=EDGE_CURVE('',#13257,#13258,#8399,.T.);
#16993=EDGE_CURVE('',#13257,#13255,#1013,.T.);
#16994=EDGE_CURVE('',#13256,#13258,#1014,.T.);
#16995=EDGE_CURVE('',#13259,#13260,#8400,.T.);
#16996=EDGE_CURVE('',#13259,#13257,#1015,.T.);
#16997=EDGE_CURVE('',#13258,#13260,#1016,.T.);
#16998=EDGE_CURVE('',#13261,#13262,#8401,.T.);
#16999=EDGE_CURVE('',#13261,#13259,#1017,.T.);
#17000=EDGE_CURVE('',#13260,#13262,#1018,.T.);
#17001=EDGE_CURVE('',#13263,#13264,#8402,.T.);
#17002=EDGE_CURVE('',#13263,#13261,#1019,.T.);
#17003=EDGE_CURVE('',#13262,#13264,#1020,.T.);
#17004=EDGE_CURVE('',#13265,#13266,#8403,.T.);
#17005=EDGE_CURVE('',#13265,#13263,#1021,.T.);
#17006=EDGE_CURVE('',#13264,#13266,#1022,.T.);
#17007=EDGE_CURVE('',#13267,#13268,#8404,.T.);
#17008=EDGE_CURVE('',#13267,#13265,#1023,.T.);
#17009=EDGE_CURVE('',#13266,#13268,#1024,.T.);
#17010=EDGE_CURVE('',#13269,#13270,#8405,.T.);
#17011=EDGE_CURVE('',#13269,#13267,#1025,.T.);
#17012=EDGE_CURVE('',#13268,#13270,#1026,.T.);
#17013=EDGE_CURVE('',#13271,#13272,#8406,.T.);
#17014=EDGE_CURVE('',#13271,#13269,#1027,.T.);
#17015=EDGE_CURVE('',#13270,#13272,#1028,.T.);
#17016=EDGE_CURVE('',#13273,#13274,#8407,.T.);
#17017=EDGE_CURVE('',#13273,#13271,#1029,.T.);
#17018=EDGE_CURVE('',#13272,#13274,#1030,.T.);
#17019=EDGE_CURVE('',#13275,#13276,#8408,.T.);
#17020=EDGE_CURVE('',#13275,#13273,#1031,.T.);
#17021=EDGE_CURVE('',#13274,#13276,#1032,.T.);
#17022=EDGE_CURVE('',#13277,#13278,#8409,.T.);
#17023=EDGE_CURVE('',#13277,#13275,#1033,.T.);
#17024=EDGE_CURVE('',#13276,#13278,#1034,.T.);
#17025=EDGE_CURVE('',#13279,#13280,#8410,.T.);
#17026=EDGE_CURVE('',#13279,#13277,#1035,.T.);
#17027=EDGE_CURVE('',#13278,#13280,#1036,.T.);
#17028=EDGE_CURVE('',#13281,#13282,#8411,.T.);
#17029=EDGE_CURVE('',#13281,#13279,#1037,.T.);
#17030=EDGE_CURVE('',#13280,#13282,#1038,.T.);
#17031=EDGE_CURVE('',#13283,#13284,#8412,.T.);
#17032=EDGE_CURVE('',#13283,#13281,#1039,.T.);
#17033=EDGE_CURVE('',#13282,#13284,#1040,.T.);
#17034=EDGE_CURVE('',#13285,#13286,#8413,.T.);
#17035=EDGE_CURVE('',#13285,#13283,#1041,.T.);
#17036=EDGE_CURVE('',#13284,#13286,#1042,.T.);
#17037=EDGE_CURVE('',#13287,#13288,#8414,.T.);
#17038=EDGE_CURVE('',#13287,#13285,#1043,.T.);
#17039=EDGE_CURVE('',#13286,#13288,#1044,.T.);
#17040=EDGE_CURVE('',#13289,#13290,#8415,.T.);
#17041=EDGE_CURVE('',#13289,#13287,#1045,.T.);
#17042=EDGE_CURVE('',#13288,#13290,#1046,.T.);
#17043=EDGE_CURVE('',#13291,#13292,#8416,.T.);
#17044=EDGE_CURVE('',#13291,#13289,#1047,.T.);
#17045=EDGE_CURVE('',#13290,#13292,#1048,.T.);
#17046=EDGE_CURVE('',#13293,#13294,#8417,.T.);
#17047=EDGE_CURVE('',#13293,#13291,#1049,.T.);
#17048=EDGE_CURVE('',#13292,#13294,#1050,.T.);
#17049=EDGE_CURVE('',#13295,#13296,#8418,.T.);
#17050=EDGE_CURVE('',#13295,#13293,#1051,.T.);
#17051=EDGE_CURVE('',#13294,#13296,#1052,.T.);
#17052=EDGE_CURVE('',#13297,#13298,#8419,.T.);
#17053=EDGE_CURVE('',#13297,#13295,#1053,.T.);
#17054=EDGE_CURVE('',#13296,#13298,#1054,.T.);
#17055=EDGE_CURVE('',#13299,#13300,#8420,.T.);
#17056=EDGE_CURVE('',#13299,#13297,#1055,.T.);
#17057=EDGE_CURVE('',#13298,#13300,#1056,.T.);
#17058=EDGE_CURVE('',#13301,#13302,#8421,.T.);
#17059=EDGE_CURVE('',#13301,#13299,#1057,.T.);
#17060=EDGE_CURVE('',#13300,#13302,#1058,.T.);
#17061=EDGE_CURVE('',#13303,#13304,#8422,.T.);
#17062=EDGE_CURVE('',#13303,#13301,#1059,.T.);
#17063=EDGE_CURVE('',#13302,#13304,#1060,.T.);
#17064=EDGE_CURVE('',#13305,#13306,#8423,.T.);
#17065=EDGE_CURVE('',#13305,#13303,#1061,.T.);
#17066=EDGE_CURVE('',#13304,#13306,#1062,.T.);
#17067=EDGE_CURVE('',#13307,#13308,#8424,.T.);
#17068=EDGE_CURVE('',#13307,#13305,#1063,.T.);
#17069=EDGE_CURVE('',#13306,#13308,#1064,.T.);
#17070=EDGE_CURVE('',#13309,#13310,#8425,.T.);
#17071=EDGE_CURVE('',#13309,#13307,#1065,.T.);
#17072=EDGE_CURVE('',#13308,#13310,#1066,.T.);
#17073=EDGE_CURVE('',#13311,#13312,#8426,.T.);
#17074=EDGE_CURVE('',#13311,#13309,#1067,.T.);
#17075=EDGE_CURVE('',#13310,#13312,#1068,.T.);
#17076=EDGE_CURVE('',#13313,#13314,#8427,.T.);
#17077=EDGE_CURVE('',#13313,#13311,#1069,.T.);
#17078=EDGE_CURVE('',#13312,#13314,#1070,.T.);
#17079=EDGE_CURVE('',#13315,#13316,#8428,.T.);
#17080=EDGE_CURVE('',#13315,#13313,#1071,.T.);
#17081=EDGE_CURVE('',#13314,#13316,#1072,.T.);
#17082=EDGE_CURVE('',#13317,#13318,#8429,.T.);
#17083=EDGE_CURVE('',#13317,#13315,#1073,.T.);
#17084=EDGE_CURVE('',#13316,#13318,#1074,.T.);
#17085=EDGE_CURVE('',#13319,#13320,#8430,.T.);
#17086=EDGE_CURVE('',#13319,#13317,#1075,.T.);
#17087=EDGE_CURVE('',#13318,#13320,#1076,.T.);
#17088=EDGE_CURVE('',#13321,#13322,#8431,.T.);
#17089=EDGE_CURVE('',#13321,#13319,#1077,.T.);
#17090=EDGE_CURVE('',#13320,#13322,#1078,.T.);
#17091=EDGE_CURVE('',#13323,#13324,#8432,.T.);
#17092=EDGE_CURVE('',#13323,#13321,#1079,.T.);
#17093=EDGE_CURVE('',#13322,#13324,#1080,.T.);
#17094=EDGE_CURVE('',#13325,#13326,#8433,.T.);
#17095=EDGE_CURVE('',#13325,#13323,#1081,.T.);
#17096=EDGE_CURVE('',#13324,#13326,#1082,.T.);
#17097=EDGE_CURVE('',#13327,#13328,#8434,.T.);
#17098=EDGE_CURVE('',#13327,#13325,#1083,.T.);
#17099=EDGE_CURVE('',#13326,#13328,#1084,.T.);
#17100=EDGE_CURVE('',#13329,#13330,#8435,.T.);
#17101=EDGE_CURVE('',#13329,#13327,#1085,.T.);
#17102=EDGE_CURVE('',#13328,#13330,#1086,.T.);
#17103=EDGE_CURVE('',#13331,#13332,#8436,.T.);
#17104=EDGE_CURVE('',#13331,#13329,#1087,.T.);
#17105=EDGE_CURVE('',#13330,#13332,#1088,.T.);
#17106=EDGE_CURVE('',#13333,#13334,#8437,.T.);
#17107=EDGE_CURVE('',#13335,#13333,#2551,.T.);
#17108=EDGE_CURVE('',#13335,#13331,#1089,.T.);
#17109=EDGE_CURVE('',#13332,#13334,#1090,.T.);
#17110=EDGE_CURVE('',#13336,#13337,#8438,.T.);
#17111=EDGE_CURVE('',#13336,#13338,#1091,.T.);
#17112=EDGE_CURVE('',#13339,#13338,#2552,.T.);
#17113=EDGE_CURVE('',#13337,#13339,#1092,.T.);
#17114=EDGE_CURVE('',#13340,#13341,#8439,.T.);
#17115=EDGE_CURVE('',#13340,#13336,#1093,.T.);
#17116=EDGE_CURVE('',#13341,#13337,#1094,.T.);
#17117=EDGE_CURVE('',#13342,#13343,#8440,.T.);
#17118=EDGE_CURVE('',#13342,#13340,#1095,.T.);
#17119=EDGE_CURVE('',#13343,#13341,#1096,.T.);
#17120=EDGE_CURVE('',#13344,#13345,#8441,.T.);
#17121=EDGE_CURVE('',#13344,#13342,#1097,.T.);
#17122=EDGE_CURVE('',#13345,#13343,#1098,.T.);
#17123=EDGE_CURVE('',#13346,#13347,#8442,.T.);
#17124=EDGE_CURVE('',#13346,#13344,#1099,.T.);
#17125=EDGE_CURVE('',#13347,#13345,#1100,.T.);
#17126=EDGE_CURVE('',#13348,#13349,#8443,.T.);
#17127=EDGE_CURVE('',#13348,#13346,#1101,.T.);
#17128=EDGE_CURVE('',#13349,#13347,#1102,.T.);
#17129=EDGE_CURVE('',#13350,#13351,#8444,.T.);
#17130=EDGE_CURVE('',#13350,#13348,#1103,.T.);
#17131=EDGE_CURVE('',#13351,#13349,#1104,.T.);
#17132=EDGE_CURVE('',#13352,#13353,#8445,.T.);
#17133=EDGE_CURVE('',#13352,#13350,#1105,.T.);
#17134=EDGE_CURVE('',#13353,#13351,#1106,.T.);
#17135=EDGE_CURVE('',#13354,#13355,#8446,.T.);
#17136=EDGE_CURVE('',#13354,#13352,#1107,.T.);
#17137=EDGE_CURVE('',#13355,#13353,#1108,.T.);
#17138=EDGE_CURVE('',#13356,#13357,#8447,.T.);
#17139=EDGE_CURVE('',#13356,#13354,#1109,.T.);
#17140=EDGE_CURVE('',#13357,#13355,#1110,.T.);
#17141=EDGE_CURVE('',#13358,#13359,#8448,.T.);
#17142=EDGE_CURVE('',#13358,#13356,#1111,.T.);
#17143=EDGE_CURVE('',#13359,#13357,#1112,.T.);
#17144=EDGE_CURVE('',#13360,#13361,#8449,.T.);
#17145=EDGE_CURVE('',#13360,#13358,#1113,.T.);
#17146=EDGE_CURVE('',#13361,#13359,#1114,.T.);
#17147=EDGE_CURVE('',#13362,#13363,#8450,.T.);
#17148=EDGE_CURVE('',#13362,#13360,#1115,.T.);
#17149=EDGE_CURVE('',#13363,#13361,#1116,.T.);
#17150=EDGE_CURVE('',#13364,#13365,#8451,.T.);
#17151=EDGE_CURVE('',#13364,#13362,#1117,.T.);
#17152=EDGE_CURVE('',#13365,#13363,#1118,.T.);
#17153=EDGE_CURVE('',#13366,#13367,#8452,.T.);
#17154=EDGE_CURVE('',#13366,#13364,#1119,.T.);
#17155=EDGE_CURVE('',#13367,#13365,#1120,.T.);
#17156=EDGE_CURVE('',#13368,#13369,#8453,.T.);
#17157=EDGE_CURVE('',#13368,#13366,#1121,.T.);
#17158=EDGE_CURVE('',#13369,#13367,#1122,.T.);
#17159=EDGE_CURVE('',#13370,#13371,#8454,.T.);
#17160=EDGE_CURVE('',#13370,#13368,#1123,.T.);
#17161=EDGE_CURVE('',#13371,#13369,#1124,.T.);
#17162=EDGE_CURVE('',#13372,#13373,#8455,.T.);
#17163=EDGE_CURVE('',#13372,#13370,#1125,.T.);
#17164=EDGE_CURVE('',#13373,#13371,#1126,.T.);
#17165=EDGE_CURVE('',#13374,#13375,#8456,.T.);
#17166=EDGE_CURVE('',#13374,#13372,#1127,.T.);
#17167=EDGE_CURVE('',#13375,#13373,#1128,.T.);
#17168=EDGE_CURVE('',#13376,#13377,#8457,.T.);
#17169=EDGE_CURVE('',#13376,#13374,#1129,.T.);
#17170=EDGE_CURVE('',#13377,#13375,#1130,.T.);
#17171=EDGE_CURVE('',#13378,#13379,#8458,.T.);
#17172=EDGE_CURVE('',#13378,#13376,#1131,.T.);
#17173=EDGE_CURVE('',#13379,#13377,#1132,.T.);
#17174=EDGE_CURVE('',#13380,#13381,#8459,.T.);
#17175=EDGE_CURVE('',#13380,#13378,#1133,.T.);
#17176=EDGE_CURVE('',#13381,#13379,#1134,.T.);
#17177=EDGE_CURVE('',#13382,#13383,#8460,.T.);
#17178=EDGE_CURVE('',#13382,#13380,#1135,.T.);
#17179=EDGE_CURVE('',#13383,#13381,#1136,.T.);
#17180=EDGE_CURVE('',#13384,#13385,#8461,.T.);
#17181=EDGE_CURVE('',#13384,#13382,#1137,.T.);
#17182=EDGE_CURVE('',#13385,#13383,#1138,.T.);
#17183=EDGE_CURVE('',#13386,#13387,#8462,.T.);
#17184=EDGE_CURVE('',#13386,#13384,#1139,.T.);
#17185=EDGE_CURVE('',#13387,#13385,#1140,.T.);
#17186=EDGE_CURVE('',#13388,#13389,#8463,.T.);
#17187=EDGE_CURVE('',#13388,#13386,#1141,.T.);
#17188=EDGE_CURVE('',#13389,#13387,#1142,.T.);
#17189=EDGE_CURVE('',#13390,#13391,#8464,.T.);
#17190=EDGE_CURVE('',#13390,#13388,#1143,.T.);
#17191=EDGE_CURVE('',#13391,#13389,#1144,.T.);
#17192=EDGE_CURVE('',#13392,#13393,#8465,.T.);
#17193=EDGE_CURVE('',#13392,#13390,#1145,.T.);
#17194=EDGE_CURVE('',#13393,#13391,#1146,.T.);
#17195=EDGE_CURVE('',#13394,#13395,#8466,.T.);
#17196=EDGE_CURVE('',#13394,#13392,#1147,.T.);
#17197=EDGE_CURVE('',#13395,#13393,#1148,.T.);
#17198=EDGE_CURVE('',#13396,#13397,#8467,.T.);
#17199=EDGE_CURVE('',#13396,#13394,#1149,.T.);
#17200=EDGE_CURVE('',#13397,#13395,#1150,.T.);
#17201=EDGE_CURVE('',#13398,#13399,#8468,.T.);
#17202=EDGE_CURVE('',#13398,#13396,#1151,.T.);
#17203=EDGE_CURVE('',#13399,#13397,#1152,.T.);
#17204=EDGE_CURVE('',#13400,#13401,#8469,.T.);
#17205=EDGE_CURVE('',#13400,#13398,#1153,.T.);
#17206=EDGE_CURVE('',#13401,#13399,#1154,.T.);
#17207=EDGE_CURVE('',#13402,#13403,#8470,.T.);
#17208=EDGE_CURVE('',#13402,#13400,#1155,.T.);
#17209=EDGE_CURVE('',#13403,#13401,#1156,.T.);
#17210=EDGE_CURVE('',#13404,#13405,#8471,.T.);
#17211=EDGE_CURVE('',#13404,#13402,#1157,.T.);
#17212=EDGE_CURVE('',#13405,#13403,#1158,.T.);
#17213=EDGE_CURVE('',#13406,#13407,#8472,.T.);
#17214=EDGE_CURVE('',#13406,#13404,#1159,.T.);
#17215=EDGE_CURVE('',#13407,#13405,#1160,.T.);
#17216=EDGE_CURVE('',#13408,#13409,#8473,.T.);
#17217=EDGE_CURVE('',#13408,#13406,#1161,.T.);
#17218=EDGE_CURVE('',#13409,#13407,#1162,.T.);
#17219=EDGE_CURVE('',#13410,#13411,#8474,.T.);
#17220=EDGE_CURVE('',#13410,#13408,#1163,.T.);
#17221=EDGE_CURVE('',#13411,#13409,#1164,.T.);
#17222=EDGE_CURVE('',#13412,#13413,#8475,.T.);
#17223=EDGE_CURVE('',#13412,#13410,#1165,.T.);
#17224=EDGE_CURVE('',#13413,#13411,#1166,.T.);
#17225=EDGE_CURVE('',#13414,#13415,#8476,.T.);
#17226=EDGE_CURVE('',#13414,#13412,#1167,.T.);
#17227=EDGE_CURVE('',#13415,#13413,#1168,.T.);
#17228=EDGE_CURVE('',#13416,#13417,#8477,.T.);
#17229=EDGE_CURVE('',#13416,#13414,#1169,.T.);
#17230=EDGE_CURVE('',#13417,#13415,#1170,.T.);
#17231=EDGE_CURVE('',#13418,#13419,#8478,.T.);
#17232=EDGE_CURVE('',#13418,#13416,#1171,.T.);
#17233=EDGE_CURVE('',#13419,#13417,#1172,.T.);
#17234=EDGE_CURVE('',#13420,#13421,#8479,.T.);
#17235=EDGE_CURVE('',#13420,#13418,#1173,.T.);
#17236=EDGE_CURVE('',#13421,#13419,#1174,.T.);
#17237=EDGE_CURVE('',#13422,#13423,#8480,.T.);
#17238=EDGE_CURVE('',#13422,#13420,#1175,.T.);
#17239=EDGE_CURVE('',#13423,#13421,#1176,.T.);
#17240=EDGE_CURVE('',#13424,#13425,#8481,.T.);
#17241=EDGE_CURVE('',#13424,#13422,#1177,.T.);
#17242=EDGE_CURVE('',#13425,#13423,#1178,.T.);
#17243=EDGE_CURVE('',#13426,#13427,#8482,.T.);
#17244=EDGE_CURVE('',#13426,#13424,#1179,.T.);
#17245=EDGE_CURVE('',#13427,#13425,#1180,.T.);
#17246=EDGE_CURVE('',#13428,#13429,#8483,.T.);
#17247=EDGE_CURVE('',#13428,#13426,#1181,.T.);
#17248=EDGE_CURVE('',#13429,#13427,#1182,.T.);
#17249=EDGE_CURVE('',#13430,#13431,#8484,.T.);
#17250=EDGE_CURVE('',#13430,#13428,#1183,.T.);
#17251=EDGE_CURVE('',#13431,#13429,#1184,.T.);
#17252=EDGE_CURVE('',#13432,#13433,#8485,.T.);
#17253=EDGE_CURVE('',#13432,#13430,#1185,.T.);
#17254=EDGE_CURVE('',#13433,#13431,#1186,.T.);
#17255=EDGE_CURVE('',#13434,#13435,#8486,.T.);
#17256=EDGE_CURVE('',#13434,#13432,#1187,.T.);
#17257=EDGE_CURVE('',#13435,#13433,#1188,.T.);
#17258=EDGE_CURVE('',#13436,#13437,#8487,.T.);
#17259=EDGE_CURVE('',#13436,#13434,#1189,.T.);
#17260=EDGE_CURVE('',#13437,#13435,#1190,.T.);
#17261=EDGE_CURVE('',#13438,#13439,#8488,.T.);
#17262=EDGE_CURVE('',#13438,#13436,#1191,.T.);
#17263=EDGE_CURVE('',#13439,#13437,#1192,.T.);
#17264=EDGE_CURVE('',#13440,#13441,#8489,.T.);
#17265=EDGE_CURVE('',#13440,#13438,#1193,.T.);
#17266=EDGE_CURVE('',#13441,#13439,#1194,.T.);
#17267=EDGE_CURVE('',#13442,#13443,#8490,.T.);
#17268=EDGE_CURVE('',#13442,#13440,#1195,.T.);
#17269=EDGE_CURVE('',#13443,#13441,#1196,.T.);
#17270=EDGE_CURVE('',#13444,#13445,#8491,.T.);
#17271=EDGE_CURVE('',#13444,#13442,#1197,.T.);
#17272=EDGE_CURVE('',#13445,#13443,#1198,.T.);
#17273=EDGE_CURVE('',#13446,#13447,#8492,.T.);
#17274=EDGE_CURVE('',#13446,#13444,#1199,.T.);
#17275=EDGE_CURVE('',#13447,#13445,#1200,.T.);
#17276=EDGE_CURVE('',#13448,#13449,#8493,.T.);
#17277=EDGE_CURVE('',#13448,#13446,#1201,.T.);
#17278=EDGE_CURVE('',#13449,#13447,#1202,.T.);
#17279=EDGE_CURVE('',#13450,#13451,#8494,.T.);
#17280=EDGE_CURVE('',#13450,#13448,#1203,.T.);
#17281=EDGE_CURVE('',#13451,#13449,#1204,.T.);
#17282=EDGE_CURVE('',#13452,#13453,#8495,.T.);
#17283=EDGE_CURVE('',#13452,#13450,#1205,.T.);
#17284=EDGE_CURVE('',#13453,#13451,#1206,.T.);
#17285=EDGE_CURVE('',#13454,#13455,#8496,.T.);
#17286=EDGE_CURVE('',#13454,#13452,#1207,.T.);
#17287=EDGE_CURVE('',#13455,#13453,#1208,.T.);
#17288=EDGE_CURVE('',#13456,#13457,#1209,.T.);
#17289=EDGE_CURVE('',#13456,#13458,#8497,.T.);
#17290=EDGE_CURVE('',#13458,#13459,#1210,.T.);
#17291=EDGE_CURVE('',#13457,#13459,#8498,.T.);
#17292=EDGE_CURVE('',#13460,#13456,#1211,.T.);
#17293=EDGE_CURVE('',#13460,#13461,#8499,.T.);
#17294=EDGE_CURVE('',#13461,#13458,#1212,.T.);
#17295=EDGE_CURVE('',#13462,#13460,#1213,.T.);
#17296=EDGE_CURVE('',#13462,#13463,#8500,.T.);
#17297=EDGE_CURVE('',#13463,#13461,#1214,.T.);
#17298=EDGE_CURVE('',#13464,#13462,#1215,.T.);
#17299=EDGE_CURVE('',#13464,#13465,#8501,.T.);
#17300=EDGE_CURVE('',#13465,#13463,#1216,.T.);
#17301=EDGE_CURVE('',#13466,#13464,#1217,.T.);
#17302=EDGE_CURVE('',#13466,#13467,#8502,.T.);
#17303=EDGE_CURVE('',#13467,#13465,#1218,.T.);
#17304=EDGE_CURVE('',#13468,#13466,#1219,.T.);
#17305=EDGE_CURVE('',#13468,#13469,#8503,.T.);
#17306=EDGE_CURVE('',#13469,#13467,#1220,.T.);
#17307=EDGE_CURVE('',#13470,#13468,#1221,.T.);
#17308=EDGE_CURVE('',#13470,#13471,#8504,.T.);
#17309=EDGE_CURVE('',#13471,#13469,#1222,.T.);
#17310=EDGE_CURVE('',#13472,#13470,#1223,.T.);
#17311=EDGE_CURVE('',#13472,#13473,#8505,.T.);
#17312=EDGE_CURVE('',#13473,#13471,#1224,.T.);
#17313=EDGE_CURVE('',#13457,#13472,#1225,.T.);
#17314=EDGE_CURVE('',#13459,#13473,#1226,.T.);
#17315=EDGE_CURVE('',#13474,#13475,#1227,.T.);
#17316=EDGE_CURVE('',#13474,#13476,#8506,.T.);
#17317=EDGE_CURVE('',#13476,#13477,#1228,.T.);
#17318=EDGE_CURVE('',#13475,#13477,#8507,.T.);
#17319=EDGE_CURVE('',#13478,#13474,#1229,.T.);
#17320=EDGE_CURVE('',#13478,#13479,#8508,.T.);
#17321=EDGE_CURVE('',#13479,#13476,#1230,.T.);
#17322=EDGE_CURVE('',#13480,#13478,#1231,.T.);
#17323=EDGE_CURVE('',#13480,#13481,#8509,.T.);
#17324=EDGE_CURVE('',#13481,#13479,#1232,.T.);
#17325=EDGE_CURVE('',#13482,#13480,#1233,.T.);
#17326=EDGE_CURVE('',#13482,#13483,#8510,.T.);
#17327=EDGE_CURVE('',#13483,#13481,#1234,.T.);
#17328=EDGE_CURVE('',#13484,#13482,#1235,.T.);
#17329=EDGE_CURVE('',#13484,#13485,#8511,.T.);
#17330=EDGE_CURVE('',#13485,#13483,#1236,.T.);
#17331=EDGE_CURVE('',#13486,#13484,#1237,.T.);
#17332=EDGE_CURVE('',#13486,#13487,#8512,.T.);
#17333=EDGE_CURVE('',#13487,#13485,#1238,.T.);
#17334=EDGE_CURVE('',#13488,#13486,#1239,.T.);
#17335=EDGE_CURVE('',#13488,#13489,#8513,.T.);
#17336=EDGE_CURVE('',#13489,#13487,#1240,.T.);
#17337=EDGE_CURVE('',#13475,#13488,#1241,.T.);
#17338=EDGE_CURVE('',#13477,#13489,#1242,.T.);
#17339=EDGE_CURVE('',#13490,#13491,#1243,.T.);
#17340=EDGE_CURVE('',#13490,#13492,#8514,.T.);
#17341=EDGE_CURVE('',#13492,#13493,#1244,.T.);
#17342=EDGE_CURVE('',#13491,#13493,#8515,.T.);
#17343=EDGE_CURVE('',#13494,#13490,#1245,.T.);
#17344=EDGE_CURVE('',#13494,#13495,#8516,.T.);
#17345=EDGE_CURVE('',#13495,#13492,#1246,.T.);
#17346=EDGE_CURVE('',#13496,#13494,#1247,.T.);
#17347=EDGE_CURVE('',#13496,#13497,#8517,.T.);
#17348=EDGE_CURVE('',#13497,#13495,#1248,.T.);
#17349=EDGE_CURVE('',#13498,#13496,#1249,.T.);
#17350=EDGE_CURVE('',#13498,#13499,#8518,.T.);
#17351=EDGE_CURVE('',#13499,#13497,#1250,.T.);
#17352=EDGE_CURVE('',#13500,#13498,#1251,.T.);
#17353=EDGE_CURVE('',#13500,#13501,#8519,.T.);
#17354=EDGE_CURVE('',#13501,#13499,#1252,.T.);
#17355=EDGE_CURVE('',#13502,#13500,#1253,.T.);
#17356=EDGE_CURVE('',#13502,#13503,#8520,.T.);
#17357=EDGE_CURVE('',#13503,#13501,#1254,.T.);
#17358=EDGE_CURVE('',#13504,#13502,#1255,.T.);
#17359=EDGE_CURVE('',#13504,#13505,#8521,.T.);
#17360=EDGE_CURVE('',#13505,#13503,#1256,.T.);
#17361=EDGE_CURVE('',#13506,#13504,#1257,.T.);
#17362=EDGE_CURVE('',#13506,#13507,#8522,.T.);
#17363=EDGE_CURVE('',#13507,#13505,#1258,.T.);
#17364=EDGE_CURVE('',#13508,#13506,#1259,.T.);
#17365=EDGE_CURVE('',#13508,#13509,#8523,.T.);
#17366=EDGE_CURVE('',#13509,#13507,#1260,.T.);
#17367=EDGE_CURVE('',#13510,#13508,#1261,.T.);
#17368=EDGE_CURVE('',#13510,#13511,#8524,.T.);
#17369=EDGE_CURVE('',#13511,#13509,#1262,.T.);
#17370=EDGE_CURVE('',#13512,#13510,#1263,.T.);
#17371=EDGE_CURVE('',#13512,#13513,#8525,.T.);
#17372=EDGE_CURVE('',#13513,#13511,#1264,.T.);
#17373=EDGE_CURVE('',#13514,#13512,#1265,.T.);
#17374=EDGE_CURVE('',#13514,#13515,#8526,.T.);
#17375=EDGE_CURVE('',#13515,#13513,#1266,.T.);
#17376=EDGE_CURVE('',#13516,#13514,#1267,.T.);
#17377=EDGE_CURVE('',#13516,#13517,#8527,.T.);
#17378=EDGE_CURVE('',#13517,#13515,#1268,.T.);
#17379=EDGE_CURVE('',#13518,#13516,#1269,.T.);
#17380=EDGE_CURVE('',#13518,#13519,#8528,.T.);
#17381=EDGE_CURVE('',#13519,#13517,#1270,.T.);
#17382=EDGE_CURVE('',#13520,#13518,#1271,.T.);
#17383=EDGE_CURVE('',#13520,#13521,#8529,.T.);
#17384=EDGE_CURVE('',#13521,#13519,#1272,.T.);
#17385=EDGE_CURVE('',#13491,#13520,#1273,.T.);
#17386=EDGE_CURVE('',#13493,#13521,#1274,.T.);
#17387=EDGE_CURVE('',#13522,#13523,#8530,.T.);
#17388=EDGE_CURVE('',#13522,#13524,#8531,.T.);
#17389=EDGE_CURVE('',#13524,#13525,#8532,.T.);
#17390=EDGE_CURVE('',#13523,#13525,#8533,.T.);
#17391=EDGE_CURVE('',#13526,#13522,#8534,.T.);
#17392=EDGE_CURVE('',#13526,#13527,#8535,.T.);
#17393=EDGE_CURVE('',#13527,#13524,#8536,.T.);
#17394=EDGE_CURVE('',#13528,#13526,#8537,.T.);
#17395=EDGE_CURVE('',#13528,#13529,#8538,.T.);
#17396=EDGE_CURVE('',#13529,#13527,#8539,.T.);
#17397=EDGE_CURVE('',#13523,#13528,#8540,.T.);
#17398=EDGE_CURVE('',#13525,#13529,#8541,.T.);
#17399=EDGE_CURVE('',#13530,#13531,#1275,.T.);
#17400=EDGE_CURVE('',#13530,#13532,#8542,.T.);
#17401=EDGE_CURVE('',#13532,#13533,#1276,.T.);
#17402=EDGE_CURVE('',#13531,#13533,#8543,.T.);
#17403=EDGE_CURVE('',#13534,#13530,#1277,.T.);
#17404=EDGE_CURVE('',#13534,#13535,#8544,.T.);
#17405=EDGE_CURVE('',#13535,#13532,#1278,.T.);
#17406=EDGE_CURVE('',#13536,#13534,#1279,.T.);
#17407=EDGE_CURVE('',#13536,#13537,#8545,.T.);
#17408=EDGE_CURVE('',#13537,#13535,#1280,.T.);
#17409=EDGE_CURVE('',#13538,#13536,#1281,.T.);
#17410=EDGE_CURVE('',#13538,#13539,#8546,.T.);
#17411=EDGE_CURVE('',#13539,#13537,#1282,.T.);
#17412=EDGE_CURVE('',#13540,#13538,#1283,.T.);
#17413=EDGE_CURVE('',#13540,#13541,#8547,.T.);
#17414=EDGE_CURVE('',#13541,#13539,#1284,.T.);
#17415=EDGE_CURVE('',#13542,#13540,#1285,.T.);
#17416=EDGE_CURVE('',#13542,#13543,#8548,.T.);
#17417=EDGE_CURVE('',#13543,#13541,#1286,.T.);
#17418=EDGE_CURVE('',#13544,#13542,#1287,.T.);
#17419=EDGE_CURVE('',#13544,#13545,#8549,.T.);
#17420=EDGE_CURVE('',#13545,#13543,#1288,.T.);
#17421=EDGE_CURVE('',#13546,#13544,#1289,.T.);
#17422=EDGE_CURVE('',#13546,#13547,#8550,.T.);
#17423=EDGE_CURVE('',#13547,#13545,#1290,.T.);
#17424=EDGE_CURVE('',#13531,#13546,#1291,.T.);
#17425=EDGE_CURVE('',#13533,#13547,#1292,.T.);
#17426=EDGE_CURVE('',#13548,#13549,#1293,.T.);
#17427=EDGE_CURVE('',#13548,#13550,#8551,.T.);
#17428=EDGE_CURVE('',#13550,#13551,#1294,.T.);
#17429=EDGE_CURVE('',#13549,#13551,#8552,.T.);
#17430=EDGE_CURVE('',#13552,#13548,#1295,.T.);
#17431=EDGE_CURVE('',#13552,#13553,#8553,.T.);
#17432=EDGE_CURVE('',#13553,#13550,#1296,.T.);
#17433=EDGE_CURVE('',#13554,#13552,#1297,.T.);
#17434=EDGE_CURVE('',#13554,#13555,#8554,.T.);
#17435=EDGE_CURVE('',#13555,#13553,#1298,.T.);
#17436=EDGE_CURVE('',#13556,#13554,#1299,.T.);
#17437=EDGE_CURVE('',#13556,#13557,#8555,.T.);
#17438=EDGE_CURVE('',#13557,#13555,#1300,.T.);
#17439=EDGE_CURVE('',#13558,#13556,#1301,.T.);
#17440=EDGE_CURVE('',#13558,#13559,#8556,.T.);
#17441=EDGE_CURVE('',#13559,#13557,#1302,.T.);
#17442=EDGE_CURVE('',#13560,#13558,#1303,.T.);
#17443=EDGE_CURVE('',#13560,#13561,#8557,.T.);
#17444=EDGE_CURVE('',#13561,#13559,#1304,.T.);
#17445=EDGE_CURVE('',#13562,#13560,#1305,.T.);
#17446=EDGE_CURVE('',#13562,#13563,#8558,.T.);
#17447=EDGE_CURVE('',#13563,#13561,#1306,.T.);
#17448=EDGE_CURVE('',#13549,#13562,#1307,.T.);
#17449=EDGE_CURVE('',#13551,#13563,#1308,.T.);
#17450=EDGE_CURVE('',#13564,#13565,#1309,.T.);
#17451=EDGE_CURVE('',#13564,#13566,#8559,.T.);
#17452=EDGE_CURVE('',#13566,#13567,#1310,.T.);
#17453=EDGE_CURVE('',#13565,#13567,#8560,.T.);
#17454=EDGE_CURVE('',#13568,#13564,#1311,.T.);
#17455=EDGE_CURVE('',#13568,#13569,#8561,.T.);
#17456=EDGE_CURVE('',#13569,#13566,#1312,.T.);
#17457=EDGE_CURVE('',#13570,#13568,#1313,.T.);
#17458=EDGE_CURVE('',#13570,#13571,#8562,.T.);
#17459=EDGE_CURVE('',#13571,#13569,#1314,.T.);
#17460=EDGE_CURVE('',#13572,#13570,#1315,.T.);
#17461=EDGE_CURVE('',#13572,#13573,#8563,.T.);
#17462=EDGE_CURVE('',#13573,#13571,#1316,.T.);
#17463=EDGE_CURVE('',#13574,#13572,#1317,.T.);
#17464=EDGE_CURVE('',#13574,#13575,#8564,.T.);
#17465=EDGE_CURVE('',#13575,#13573,#1318,.T.);
#17466=EDGE_CURVE('',#13576,#13574,#1319,.T.);
#17467=EDGE_CURVE('',#13576,#13577,#8565,.T.);
#17468=EDGE_CURVE('',#13577,#13575,#1320,.T.);
#17469=EDGE_CURVE('',#13578,#13576,#1321,.T.);
#17470=EDGE_CURVE('',#13578,#13579,#8566,.T.);
#17471=EDGE_CURVE('',#13579,#13577,#1322,.T.);
#17472=EDGE_CURVE('',#13580,#13578,#1323,.T.);
#17473=EDGE_CURVE('',#13580,#13581,#8567,.T.);
#17474=EDGE_CURVE('',#13581,#13579,#1324,.T.);
#17475=EDGE_CURVE('',#13582,#13580,#1325,.T.);
#17476=EDGE_CURVE('',#13582,#13583,#8568,.T.);
#17477=EDGE_CURVE('',#13583,#13581,#1326,.T.);
#17478=EDGE_CURVE('',#13584,#13582,#1327,.T.);
#17479=EDGE_CURVE('',#13584,#13585,#8569,.T.);
#17480=EDGE_CURVE('',#13585,#13583,#1328,.T.);
#17481=EDGE_CURVE('',#13586,#13584,#1329,.T.);
#17482=EDGE_CURVE('',#13586,#13587,#8570,.T.);
#17483=EDGE_CURVE('',#13587,#13585,#1330,.T.);
#17484=EDGE_CURVE('',#13588,#13586,#1331,.T.);
#17485=EDGE_CURVE('',#13588,#13589,#8571,.T.);
#17486=EDGE_CURVE('',#13589,#13587,#1332,.T.);
#17487=EDGE_CURVE('',#13590,#13588,#1333,.T.);
#17488=EDGE_CURVE('',#13590,#13591,#8572,.T.);
#17489=EDGE_CURVE('',#13591,#13589,#1334,.T.);
#17490=EDGE_CURVE('',#13592,#13590,#1335,.T.);
#17491=EDGE_CURVE('',#13592,#13593,#8573,.T.);
#17492=EDGE_CURVE('',#13593,#13591,#1336,.T.);
#17493=EDGE_CURVE('',#13594,#13592,#1337,.T.);
#17494=EDGE_CURVE('',#13594,#13595,#8574,.T.);
#17495=EDGE_CURVE('',#13595,#13593,#1338,.T.);
#17496=EDGE_CURVE('',#13565,#13594,#1339,.T.);
#17497=EDGE_CURVE('',#13567,#13595,#1340,.T.);
#17498=EDGE_CURVE('',#13338,#13335,#1341,.T.);
#17499=EDGE_CURVE('',#13596,#13335,#2553,.T.);
#17500=EDGE_CURVE('',#13597,#13596,#2554,.T.);
#17501=EDGE_CURVE('',#13597,#13339,#1342,.T.);
#17502=EDGE_CURVE('',#13334,#13597,#1343,.T.);
#17503=EDGE_CURVE('',#13598,#13216,#1344,.T.);
#17504=EDGE_CURVE('',#13598,#13455,#1345,.T.);
#17505=EDGE_CURVE('',#13216,#13599,#2555,.T.);
#17506=EDGE_CURVE('',#13599,#13215,#2556,.T.);
#17507=EDGE_CURVE('',#13215,#13600,#1346,.T.);
#17508=EDGE_CURVE('',#13600,#13598,#2557,.T.);
#17509=EDGE_CURVE('',#13600,#13454,#1347,.T.);
#17510=EDGE_CURVE('',#13601,#13601,#2558,.T.);
#17511=EDGE_CURVE('',#13601,#13596,#2559,.T.);
#17512=EDGE_CURVE('',#13333,#13597,#2560,.T.);
#17513=EDGE_CURVE('',#13602,#13603,#8575,.T.);
#17514=EDGE_CURVE('',#13604,#13602,#8576,.T.);
#17515=EDGE_CURVE('',#13605,#13604,#8577,.T.);
#17516=EDGE_CURVE('',#13606,#13605,#8578,.T.);
#17517=EDGE_CURVE('',#13607,#13606,#8579,.T.);
#17518=EDGE_CURVE('',#13603,#13607,#8580,.T.);
#17519=EDGE_CURVE('',#13608,#13609,#355,.T.);
#17520=EDGE_CURVE('',#13610,#13608,#356,.T.);
#17521=EDGE_CURVE('',#13611,#13610,#357,.T.);
#17522=EDGE_CURVE('',#13612,#13611,#358,.T.);
#17523=EDGE_CURVE('',#13613,#13612,#359,.T.);
#17524=EDGE_CURVE('',#13613,#13614,#8581,.T.);
#17525=EDGE_CURVE('',#13614,#13614,#2561,.T.);
#17526=EDGE_CURVE('',#13615,#13613,#360,.T.);
#17527=EDGE_CURVE('',#13609,#13615,#361,.T.);
#17528=EDGE_CURVE('',#13607,#13611,#8582,.T.);
#17529=EDGE_CURVE('',#13606,#13612,#8583,.T.);
#17530=EDGE_CURVE('',#13603,#13610,#8584,.T.);
#17531=EDGE_CURVE('',#13602,#13608,#8585,.T.);
#17532=EDGE_CURVE('',#13604,#13609,#8586,.T.);
#17533=EDGE_CURVE('',#13605,#13615,#8587,.T.);
#17534=EDGE_CURVE('',#13616,#13616,#2562,.T.);
#17535=EDGE_CURVE('',#13599,#13616,#8588,.T.);
#17536=EDGE_CURVE('',#13617,#13617,#2563,.T.);
#17537=EDGE_CURVE('',#13617,#13618,#8589,.T.);
#17538=EDGE_CURVE('',#13618,#13618,#2564,.T.);
#17539=EDGE_CURVE('',#13619,#13619,#2565,.T.);
#17540=EDGE_CURVE('',#13619,#13617,#8590,.T.);
#17541=EDGE_CURVE('',#13620,#13620,#2566,.T.);
#17542=EDGE_CURVE('',#13621,#13621,#2567,.T.);
#17543=EDGE_CURVE('',#13621,#13619,#8591,.T.);
#17544=EDGE_CURVE('',#13622,#13622,#2568,.T.);
#17545=EDGE_CURVE('',#13620,#13623,#8592,.T.);
#17546=EDGE_CURVE('',#13624,#13623,#362,.T.);
#17547=EDGE_CURVE('',#13625,#13624,#363,.T.);
#17548=EDGE_CURVE('',#13626,#13625,#364,.T.);
#17549=EDGE_CURVE('',#13627,#13626,#365,.T.);
#17550=EDGE_CURVE('',#13628,#13627,#366,.T.);
#17551=EDGE_CURVE('',#13629,#13628,#367,.T.);
#17552=EDGE_CURVE('',#13623,#13629,#368,.T.);
#17553=EDGE_CURVE('',#13627,#13630,#8593,.T.);
#17554=EDGE_CURVE('',#13630,#13631,#369,.T.);
#17555=EDGE_CURVE('',#13628,#13631,#8594,.T.);
#17556=EDGE_CURVE('',#13626,#13632,#8595,.T.);
#17557=EDGE_CURVE('',#13632,#13630,#370,.T.);
#17558=EDGE_CURVE('',#13625,#13633,#8596,.T.);
#17559=EDGE_CURVE('',#13633,#13632,#371,.T.);
#17560=EDGE_CURVE('',#13634,#13633,#372,.T.);
#17561=EDGE_CURVE('',#13635,#13634,#373,.T.);
#17562=EDGE_CURVE('',#13635,#13622,#8597,.T.);
#17563=EDGE_CURVE('',#13636,#13635,#374,.T.);
#17564=EDGE_CURVE('',#13631,#13636,#375,.T.);
#17565=EDGE_CURVE('',#13624,#13634,#8598,.T.);
#17566=EDGE_CURVE('',#13629,#13636,#8599,.T.);
#17567=EDGE_CURVE('',#13637,#13637,#2569,.T.);
#17568=EDGE_CURVE('',#13637,#13638,#8600,.T.);
#17569=EDGE_CURVE('',#13638,#13638,#2570,.T.);
#17570=EDGE_CURVE('',#13639,#13639,#2571,.T.);
#17571=EDGE_CURVE('',#13640,#13640,#2572,.T.);
#17572=EDGE_CURVE('',#13640,#13639,#8601,.T.);
#17573=EDGE_CURVE('',#13641,#13641,#2573,.T.);
#17574=EDGE_CURVE('',#13641,#13640,#8602,.T.);
#17575=EDGE_CURVE('',#13642,#13642,#2574,.T.);
#17576=EDGE_CURVE('',#13642,#13637,#8603,.T.);
#17577=EDGE_CURVE('',#13643,#13643,#2575,.T.);
#17578=EDGE_CURVE('',#13643,#13644,#8604,.T.);
#17579=EDGE_CURVE('',#13644,#13645,#2576,.T.);
#17580=EDGE_CURVE('',#13645,#13644,#2577,.T.);
#17581=EDGE_CURVE('',#13645,#13646,#8605,.T.);
#17582=EDGE_CURVE('',#13647,#13646,#2578,.T.);
#17583=EDGE_CURVE('',#13646,#13647,#2579,.T.);
#17584=EDGE_CURVE('',#13647,#13648,#8606,.T.);
#17585=EDGE_CURVE('',#13648,#13649,#2580,.T.);
#17586=EDGE_CURVE('',#13649,#13648,#2581,.T.);
#17587=EDGE_CURVE('',#13649,#13650,#8607,.T.);
#17588=EDGE_CURVE('',#13650,#13650,#2582,.T.);
#17589=EDGE_CURVE('',#13651,#13651,#2583,.T.);
#17590=EDGE_CURVE('',#13651,#13652,#8608,.T.);
#17591=EDGE_CURVE('',#13652,#13652,#2584,.T.);
#17592=EDGE_CURVE('',#13653,#13653,#2585,.T.);
#17593=EDGE_CURVE('',#13653,#13652,#8609,.T.);
#17594=EDGE_CURVE('',#13654,#13655,#8610,.T.);
#17595=EDGE_CURVE('',#13656,#13655,#8611,.T.);
#17596=EDGE_CURVE('',#13657,#13656,#2586,.T.);
#17597=EDGE_CURVE('',#13654,#13657,#8612,.T.);
#17598=EDGE_CURVE('',#13658,#13658,#2587,.T.);
#17599=EDGE_CURVE('',#13658,#13653,#8613,.T.);
#17600=EDGE_CURVE('',#13659,#13660,#8614,.T.);
#17601=EDGE_CURVE('',#13661,#13660,#8615,.T.);
#17602=EDGE_CURVE('',#13662,#13661,#2588,.T.);
#17603=EDGE_CURVE('',#13659,#13662,#8616,.T.);
#17604=EDGE_CURVE('',#13663,#13664,#2589,.T.);
#17605=EDGE_CURVE('',#13664,#13663,#2590,.T.);
#17606=EDGE_CURVE('',#13663,#13665,#8617,.T.);
#17607=EDGE_CURVE('',#13665,#13665,#2591,.T.);
#17608=EDGE_CURVE('',#13666,#13666,#2592,.T.);
#17609=EDGE_CURVE('',#13666,#13664,#8618,.T.);
#17610=EDGE_CURVE('',#13667,#13667,#2593,.T.);
#17611=EDGE_CURVE('',#13668,#13668,#2594,.T.);
#17612=EDGE_CURVE('',#13669,#13669,#2595,.T.);
#17613=EDGE_CURVE('',#13669,#13668,#8619,.T.);
#17614=EDGE_CURVE('',#13670,#13670,#2596,.T.);
#17615=EDGE_CURVE('',#13670,#13671,#8620,.T.);
#17616=EDGE_CURVE('',#13671,#13671,#2597,.T.);
#17617=EDGE_CURVE('',#13672,#13672,#2598,.T.);
#17618=EDGE_CURVE('',#13673,#13673,#2599,.T.);
#17619=EDGE_CURVE('',#13673,#13672,#8621,.T.);
#17620=EDGE_CURVE('',#13674,#13674,#2600,.T.);
#17621=EDGE_CURVE('',#13674,#13675,#8622,.T.);
#17622=EDGE_CURVE('',#13675,#13675,#2601,.T.);
#17623=EDGE_CURVE('',#13676,#13676,#2602,.T.);
#17624=EDGE_CURVE('',#13677,#13677,#2603,.T.);
#17625=EDGE_CURVE('',#13677,#13676,#8623,.T.);
#17626=EDGE_CURVE('',#13678,#13678,#2604,.T.);
#17627=EDGE_CURVE('',#13660,#13679,#8624,.T.);
#17628=EDGE_CURVE('',#13680,#13659,#8625,.T.);
#17629=EDGE_CURVE('',#13681,#13680,#8626,.T.);
#17630=EDGE_CURVE('',#13655,#13681,#8627,.T.);
#17631=EDGE_CURVE('',#13682,#13654,#8628,.T.);
#17632=EDGE_CURVE('',#13679,#13682,#8629,.T.);
#17633=EDGE_CURVE('',#13683,#13683,#2605,.T.);
#17634=EDGE_CURVE('',#13683,#13678,#8630,.T.);
#17635=EDGE_CURVE('',#13684,#13684,#2606,.T.);
#17636=EDGE_CURVE('',#13684,#13683,#8631,.T.);
#17637=EDGE_CURVE('',#13685,#13685,#2607,.T.);
#17638=EDGE_CURVE('',#13685,#13684,#8632,.T.);
#17639=EDGE_CURVE('',#13686,#13686,#2608,.T.);
#17640=EDGE_CURVE('',#13667,#13686,#8633,.T.);
#17641=EDGE_CURVE('',#13681,#13687,#8634,.T.);
#17642=EDGE_CURVE('',#13687,#13656,#8635,.T.);
#17643=EDGE_CURVE('',#13688,#13680,#8636,.T.);
#17644=EDGE_CURVE('',#13688,#13687,#8637,.T.);
#17645=EDGE_CURVE('',#13688,#13662,#8638,.T.);
#17646=EDGE_CURVE('',#13689,#13657,#8639,.T.);
#17647=EDGE_CURVE('',#13687,#13689,#2609,.T.);
#17648=EDGE_CURVE('',#13689,#13682,#8640,.T.);
#17649=EDGE_CURVE('',#13690,#13688,#2610,.T.);
#17650=EDGE_CURVE('',#13690,#13689,#8641,.T.);
#17651=EDGE_CURVE('',#13679,#13690,#8642,.T.);
#17652=EDGE_CURVE('',#13690,#13661,#8643,.T.);
#17653=EDGE_CURVE('',#13691,#13691,#2611,.T.);
#17654=EDGE_CURVE('',#13691,#13692,#8644,.T.);
#17655=EDGE_CURVE('',#13692,#13692,#2612,.T.);
#17656=EDGE_CURVE('',#13693,#13694,#8645,.T.);
#17657=EDGE_CURVE('',#13695,#13693,#8646,.T.);
#17658=EDGE_CURVE('',#13696,#13695,#8647,.T.);
#17659=EDGE_CURVE('',#13694,#13696,#8648,.T.);
#17660=EDGE_CURVE('',#13697,#13697,#2613,.T.);
#17661=EDGE_CURVE('',#13698,#13698,#2614,.T.);
#17662=EDGE_CURVE('',#13699,#13699,#2615,.T.);
#17663=EDGE_CURVE('',#13700,#13700,#2616,.T.);
#17664=EDGE_CURVE('',#13701,#13701,#2617,.T.);
#17665=EDGE_CURVE('',#13702,#13702,#2618,.T.);
#17666=EDGE_CURVE('',#13703,#13703,#2619,.T.);
#17667=EDGE_CURVE('',#13704,#13704,#2620,.T.);
#17668=EDGE_CURVE('',#13705,#13705,#2621,.T.);
#17669=EDGE_CURVE('',#13706,#13706,#2622,.T.);
#17670=EDGE_CURVE('',#13692,#13707,#8649,.T.);
#17671=EDGE_CURVE('',#13707,#13707,#2623,.T.);
#17672=EDGE_CURVE('',#13697,#13708,#8650,.T.);
#17673=EDGE_CURVE('',#13708,#13708,#2624,.T.);
#17674=EDGE_CURVE('',#13708,#13709,#8651,.T.);
#17675=EDGE_CURVE('',#13709,#13709,#2625,.T.);
#17676=EDGE_CURVE('',#13706,#13710,#8652,.T.);
#17677=EDGE_CURVE('',#13710,#13710,#2626,.T.);
#17678=EDGE_CURVE('',#13710,#13711,#8653,.T.);
#17679=EDGE_CURVE('',#13711,#13711,#2627,.T.);
#17680=EDGE_CURVE('',#13698,#13712,#8654,.T.);
#17681=EDGE_CURVE('',#13712,#13712,#2628,.T.);
#17682=EDGE_CURVE('',#13712,#13713,#8655,.T.);
#17683=EDGE_CURVE('',#13713,#13713,#2629,.T.);
#17684=EDGE_CURVE('',#13705,#13714,#8656,.T.);
#17685=EDGE_CURVE('',#13714,#13714,#2630,.T.);
#17686=EDGE_CURVE('',#13714,#13715,#8657,.T.);
#17687=EDGE_CURVE('',#13715,#13715,#2631,.T.);
#17688=EDGE_CURVE('',#13699,#13716,#8658,.T.);
#17689=EDGE_CURVE('',#13716,#13716,#2632,.T.);
#17690=EDGE_CURVE('',#13716,#13717,#8659,.T.);
#17691=EDGE_CURVE('',#13717,#13717,#2633,.T.);
#17692=EDGE_CURVE('',#13704,#13718,#8660,.T.);
#17693=EDGE_CURVE('',#13718,#13718,#2634,.T.);
#17694=EDGE_CURVE('',#13718,#13719,#8661,.T.);
#17695=EDGE_CURVE('',#13719,#13719,#2635,.T.);
#17696=EDGE_CURVE('',#13720,#13720,#2636,.T.);
#17697=EDGE_CURVE('',#13720,#13721,#8662,.T.);
#17698=EDGE_CURVE('',#13721,#13721,#2637,.T.);
#17699=EDGE_CURVE('',#13722,#13723,#8663,.T.);
#17700=EDGE_CURVE('',#13724,#13722,#8664,.T.);
#17701=EDGE_CURVE('',#13725,#13724,#8665,.T.);
#17702=EDGE_CURVE('',#13723,#13725,#8666,.T.);
#17703=EDGE_CURVE('',#13726,#13726,#2638,.T.);
#17704=EDGE_CURVE('',#13727,#13727,#2639,.T.);
#17705=EDGE_CURVE('',#13728,#13728,#2640,.T.);
#17706=EDGE_CURVE('',#13729,#13729,#2641,.T.);
#17707=EDGE_CURVE('',#13730,#13730,#2642,.T.);
#17708=EDGE_CURVE('',#13731,#13731,#2643,.T.);
#17709=EDGE_CURVE('',#13732,#13732,#2644,.T.);
#17710=EDGE_CURVE('',#13733,#13733,#2645,.T.);
#17711=EDGE_CURVE('',#13734,#13734,#2646,.T.);
#17712=EDGE_CURVE('',#13735,#13735,#2647,.T.);
#17713=EDGE_CURVE('',#13736,#13736,#2648,.T.);
#17714=EDGE_CURVE('',#13736,#13721,#8667,.T.);
#17715=EDGE_CURVE('',#13726,#13737,#8668,.T.);
#17716=EDGE_CURVE('',#13737,#13737,#2649,.T.);
#17717=EDGE_CURVE('',#13738,#13738,#2650,.T.);
#17718=EDGE_CURVE('',#13738,#13737,#8669,.T.);
#17719=EDGE_CURVE('',#13735,#13739,#8670,.T.);
#17720=EDGE_CURVE('',#13739,#13739,#2651,.T.);
#17721=EDGE_CURVE('',#13740,#13740,#2652,.T.);
#17722=EDGE_CURVE('',#13740,#13739,#8671,.T.);
#17723=EDGE_CURVE('',#13727,#13741,#8672,.T.);
#17724=EDGE_CURVE('',#13741,#13741,#2653,.T.);
#17725=EDGE_CURVE('',#13742,#13742,#2654,.T.);
#17726=EDGE_CURVE('',#13742,#13741,#8673,.T.);
#17727=EDGE_CURVE('',#13734,#13743,#8674,.T.);
#17728=EDGE_CURVE('',#13743,#13743,#2655,.T.);
#17729=EDGE_CURVE('',#13744,#13744,#2656,.T.);
#17730=EDGE_CURVE('',#13744,#13743,#8675,.T.);
#17731=EDGE_CURVE('',#13745,#13722,#8676,.T.);
#17732=EDGE_CURVE('',#13723,#13746,#8677,.T.);
#17733=EDGE_CURVE('',#13746,#13745,#8678,.T.);
#17734=EDGE_CURVE('',#13747,#13748,#8679,.T.);
#17735=EDGE_CURVE('',#13748,#13722,#2657,.T.);
#17736=EDGE_CURVE('',#13745,#13747,#2658,.T.);
#17737=EDGE_CURVE('',#13749,#13750,#8680,.T.);
#17738=EDGE_CURVE('',#13750,#13748,#8681,.T.);
#17739=EDGE_CURVE('',#13747,#13749,#8682,.T.);
#17740=EDGE_CURVE('',#13751,#13694,#8683,.T.);
#17741=EDGE_CURVE('',#13694,#13750,#2659,.T.);
#17742=EDGE_CURVE('',#13749,#13751,#2660,.T.);
#17743=EDGE_CURVE('',#13752,#13693,#8684,.T.);
#17744=EDGE_CURVE('',#13751,#13752,#8685,.T.);
#17745=EDGE_CURVE('',#13753,#13754,#8686,.T.);
#17746=EDGE_CURVE('',#13754,#13693,#2661,.T.);
#17747=EDGE_CURVE('',#13752,#13753,#2662,.T.);
#17748=EDGE_CURVE('',#13755,#13756,#8687,.T.);
#17749=EDGE_CURVE('',#13756,#13754,#8688,.T.);
#17750=EDGE_CURVE('',#13753,#13755,#8689,.T.);
#17751=EDGE_CURVE('',#13723,#13756,#2663,.T.);
#17752=EDGE_CURVE('',#13755,#13746,#2664,.T.);
#17753=EDGE_CURVE('',#13754,#13757,#8690,.T.);
#17754=EDGE_CURVE('',#13695,#13757,#2665,.T.);
#17755=EDGE_CURVE('',#13758,#13756,#8691,.T.);
#17756=EDGE_CURVE('',#13757,#13758,#8692,.T.);
#17757=EDGE_CURVE('',#13758,#13725,#2666,.T.);
#17758=EDGE_CURVE('',#13759,#13760,#8693,.T.);
#17759=EDGE_CURVE('',#13761,#13759,#2667,.T.);
#17760=EDGE_CURVE('',#13762,#13761,#8694,.T.);
#17761=EDGE_CURVE('',#13763,#13762,#2668,.T.);
#17762=EDGE_CURVE('',#13764,#13763,#8695,.T.);
#17763=EDGE_CURVE('',#13765,#13764,#2669,.T.);
#17764=EDGE_CURVE('',#13766,#13765,#8696,.T.);
#17765=EDGE_CURVE('',#13760,#13766,#2670,.T.);
#17766=EDGE_CURVE('',#13733,#13767,#8697,.T.);
#17767=EDGE_CURVE('',#13767,#13767,#2671,.T.);
#17768=EDGE_CURVE('',#13768,#13768,#2672,.T.);
#17769=EDGE_CURVE('',#13768,#13767,#8698,.T.);
#17770=EDGE_CURVE('',#13728,#13769,#8699,.T.);
#17771=EDGE_CURVE('',#13769,#13769,#2673,.T.);
#17772=EDGE_CURVE('',#13770,#13770,#2674,.T.);
#17773=EDGE_CURVE('',#13770,#13769,#8700,.T.);
#17774=EDGE_CURVE('',#13732,#13771,#8701,.T.);
#17775=EDGE_CURVE('',#13771,#13771,#2675,.T.);
#17776=EDGE_CURVE('',#13772,#13772,#2676,.T.);
#17777=EDGE_CURVE('',#13772,#13771,#8702,.T.);
#17778=EDGE_CURVE('',#13700,#13773,#8703,.T.);
#17779=EDGE_CURVE('',#13773,#13773,#2677,.T.);
#17780=EDGE_CURVE('',#13773,#13774,#8704,.T.);
#17781=EDGE_CURVE('',#13774,#13774,#2678,.T.);
#17782=EDGE_CURVE('',#13729,#13775,#8705,.T.);
#17783=EDGE_CURVE('',#13775,#13775,#2679,.T.);
#17784=EDGE_CURVE('',#13776,#13776,#2680,.T.);
#17785=EDGE_CURVE('',#13776,#13775,#8706,.T.);
#17786=EDGE_CURVE('',#13703,#13777,#8707,.T.);
#17787=EDGE_CURVE('',#13777,#13777,#2681,.T.);
#17788=EDGE_CURVE('',#13777,#13778,#8708,.T.);
#17789=EDGE_CURVE('',#13778,#13778,#2682,.T.);
#17790=EDGE_CURVE('',#13731,#13779,#8709,.T.);
#17791=EDGE_CURVE('',#13779,#13779,#2683,.T.);
#17792=EDGE_CURVE('',#13780,#13780,#2684,.T.);
#17793=EDGE_CURVE('',#13780,#13779,#8710,.T.);
#17794=EDGE_CURVE('',#13701,#13781,#8711,.T.);
#17795=EDGE_CURVE('',#13781,#13781,#2685,.T.);
#17796=EDGE_CURVE('',#13781,#13782,#8712,.T.);
#17797=EDGE_CURVE('',#13782,#13782,#2686,.T.);
#17798=EDGE_CURVE('',#13730,#13783,#8713,.T.);
#17799=EDGE_CURVE('',#13783,#13783,#2687,.T.);
#17800=EDGE_CURVE('',#13784,#13784,#2688,.T.);
#17801=EDGE_CURVE('',#13784,#13783,#8714,.T.);
#17802=EDGE_CURVE('',#13785,#13785,#2689,.T.);
#17803=EDGE_CURVE('',#13785,#13736,#8715,.T.);
#17804=EDGE_CURVE('',#13786,#13787,#8716,.T.);
#17805=EDGE_CURVE('',#13788,#13786,#8717,.T.);
#17806=EDGE_CURVE('',#13789,#13788,#8718,.T.);
#17807=EDGE_CURVE('',#13787,#13789,#8719,.T.);
#17808=EDGE_CURVE('',#13790,#13790,#2690,.T.);
#17809=EDGE_CURVE('',#13791,#13791,#2691,.T.);
#17810=EDGE_CURVE('',#13792,#13792,#2692,.T.);
#17811=EDGE_CURVE('',#13793,#13793,#2693,.T.);
#17812=EDGE_CURVE('',#13794,#13794,#2694,.T.);
#17813=EDGE_CURVE('',#13795,#13795,#2695,.T.);
#17814=EDGE_CURVE('',#13796,#13796,#2696,.T.);
#17815=EDGE_CURVE('',#13797,#13797,#2697,.T.);
#17816=EDGE_CURVE('',#13798,#13798,#2698,.T.);
#17817=EDGE_CURVE('',#13799,#13799,#2699,.T.);
#17818=EDGE_CURVE('',#13790,#13738,#8720,.T.);
#17819=EDGE_CURVE('',#13799,#13740,#8721,.T.);
#17820=EDGE_CURVE('',#13791,#13742,#8722,.T.);
#17821=EDGE_CURVE('',#13798,#13744,#8723,.T.);
#17822=EDGE_CURVE('',#13702,#13800,#8724,.T.);
#17823=EDGE_CURVE('',#13800,#13800,#2700,.T.);
#17824=EDGE_CURVE('',#13800,#13801,#8725,.T.);
#17825=EDGE_CURVE('',#13801,#13801,#2701,.T.);
#17826=EDGE_CURVE('',#13802,#13802,#2702,.T.);
#17827=EDGE_CURVE('',#13802,#13707,#8726,.T.);
#17828=EDGE_CURVE('',#13803,#13804,#8727,.T.);
#17829=EDGE_CURVE('',#13805,#13803,#8728,.T.);
#17830=EDGE_CURVE('',#13806,#13805,#8729,.T.);
#17831=EDGE_CURVE('',#13804,#13806,#8730,.T.);
#17832=EDGE_CURVE('',#13807,#13807,#2703,.T.);
#17833=EDGE_CURVE('',#13808,#13808,#2704,.T.);
#17834=EDGE_CURVE('',#13809,#13809,#2705,.T.);
#17835=EDGE_CURVE('',#13810,#13810,#2706,.T.);
#17836=EDGE_CURVE('',#13811,#13811,#2707,.T.);
#17837=EDGE_CURVE('',#13812,#13812,#2708,.T.);
#17838=EDGE_CURVE('',#13813,#13813,#2709,.T.);
#17839=EDGE_CURVE('',#13814,#13814,#2710,.T.);
#17840=EDGE_CURVE('',#13815,#13815,#2711,.T.);
#17841=EDGE_CURVE('',#13816,#13816,#2712,.T.);
#17842=EDGE_CURVE('',#13807,#13709,#8731,.T.);
#17843=EDGE_CURVE('',#13816,#13711,#8732,.T.);
#17844=EDGE_CURVE('',#13808,#13713,#8733,.T.);
#17845=EDGE_CURVE('',#13815,#13715,#8734,.T.);
#17846=EDGE_CURVE('',#13760,#13803,#8735,.T.);
#17847=EDGE_CURVE('',#13804,#13759,#8736,.T.);
#17848=EDGE_CURVE('',#13766,#13817,#8737,.T.);
#17849=EDGE_CURVE('',#13817,#13803,#2713,.T.);
#17850=EDGE_CURVE('',#13765,#13818,#8738,.T.);
#17851=EDGE_CURVE('',#13818,#13817,#8739,.T.);
#17852=EDGE_CURVE('',#13764,#13787,#8740,.T.);
#17853=EDGE_CURVE('',#13787,#13818,#2714,.T.);
#17854=EDGE_CURVE('',#13763,#13786,#8741,.T.);
#17855=EDGE_CURVE('',#13762,#13819,#8742,.T.);
#17856=EDGE_CURVE('',#13819,#13786,#2715,.T.);
#17857=EDGE_CURVE('',#13761,#13820,#8743,.T.);
#17858=EDGE_CURVE('',#13820,#13819,#8744,.T.);
#17859=EDGE_CURVE('',#13804,#13820,#2716,.T.);
#17860=EDGE_CURVE('',#13819,#13821,#8745,.T.);
#17861=EDGE_CURVE('',#13788,#13821,#2717,.T.);
#17862=EDGE_CURVE('',#13822,#13820,#8746,.T.);
#17863=EDGE_CURVE('',#13821,#13822,#8747,.T.);
#17864=EDGE_CURVE('',#13822,#13806,#2718,.T.);
#17865=EDGE_CURVE('',#13814,#13801,#8748,.T.);
#17866=EDGE_CURVE('',#13792,#13784,#8749,.T.);
#17867=EDGE_CURVE('',#13809,#13782,#8750,.T.);
#17868=EDGE_CURVE('',#13797,#13780,#8751,.T.);
#17869=EDGE_CURVE('',#13813,#13778,#8752,.T.);
#17870=EDGE_CURVE('',#13793,#13776,#8753,.T.);
#17871=EDGE_CURVE('',#13810,#13774,#8754,.T.);
#17872=EDGE_CURVE('',#13796,#13772,#8755,.T.);
#17873=EDGE_CURVE('',#13812,#13717,#8756,.T.);
#17874=EDGE_CURVE('',#13794,#13768,#8757,.T.);
#17875=EDGE_CURVE('',#13811,#13719,#8758,.T.);
#17876=EDGE_CURVE('',#13795,#13770,#8759,.T.);
#17877=EDGE_CURVE('',#13823,#13824,#8760,.T.);
#17878=EDGE_CURVE('',#13824,#13789,#2719,.T.);
#17879=EDGE_CURVE('',#13789,#13825,#8761,.T.);
#17880=EDGE_CURVE('',#13825,#13823,#2720,.T.);
#17881=EDGE_CURVE('',#13823,#13826,#8762,.T.);
#17882=EDGE_CURVE('',#13826,#13827,#8763,.T.);
#17883=EDGE_CURVE('',#13827,#13824,#8764,.T.);
#17884=EDGE_CURVE('',#13828,#13805,#8765,.T.);
#17885=EDGE_CURVE('',#13805,#13827,#2721,.T.);
#17886=EDGE_CURVE('',#13826,#13828,#2722,.T.);
#17887=EDGE_CURVE('',#13828,#13829,#8766,.T.);
#17888=EDGE_CURVE('',#13829,#13806,#8767,.T.);
#17889=EDGE_CURVE('',#13830,#13822,#8768,.T.);
#17890=EDGE_CURVE('',#13829,#13830,#2723,.T.);
#17891=EDGE_CURVE('',#13830,#13831,#8769,.T.);
#17892=EDGE_CURVE('',#13831,#13821,#8770,.T.);
#17893=EDGE_CURVE('',#13832,#13788,#8771,.T.);
#17894=EDGE_CURVE('',#13831,#13832,#2724,.T.);
#17895=EDGE_CURVE('',#13832,#13825,#8772,.T.);
#17896=EDGE_CURVE('',#13824,#13818,#8773,.T.);
#17897=EDGE_CURVE('',#13833,#13834,#2725,.T.);
#17898=EDGE_CURVE('',#13835,#13833,#8774,.T.);
#17899=EDGE_CURVE('',#13836,#13835,#2726,.T.);
#17900=EDGE_CURVE('',#13837,#13836,#8775,.T.);
#17901=EDGE_CURVE('',#13838,#13837,#2727,.T.);
#17902=EDGE_CURVE('',#13839,#13838,#8776,.T.);
#17903=EDGE_CURVE('',#13840,#13839,#2728,.T.);
#17904=EDGE_CURVE('',#13834,#13840,#8777,.T.);
#17905=EDGE_CURVE('',#13834,#13841,#8778,.T.);
#17906=EDGE_CURVE('',#13841,#13696,#2729,.T.);
#17907=EDGE_CURVE('',#13696,#13833,#8779,.T.);
#17908=EDGE_CURVE('',#13840,#13842,#8780,.T.);
#17909=EDGE_CURVE('',#13842,#13841,#8781,.T.);
#17910=EDGE_CURVE('',#13839,#13724,#8782,.T.);
#17911=EDGE_CURVE('',#13724,#13842,#2730,.T.);
#17912=EDGE_CURVE('',#13838,#13725,#8783,.T.);
#17913=EDGE_CURVE('',#13837,#13758,#8784,.T.);
#17914=EDGE_CURVE('',#13836,#13757,#8785,.T.);
#17915=EDGE_CURVE('',#13835,#13695,#8786,.T.);
#17916=EDGE_CURVE('',#13841,#13750,#8787,.T.);
#17917=EDGE_CURVE('',#13748,#13842,#8788,.T.);
#17918=EDGE_CURVE('',#13817,#13827,#8789,.T.);
#17919=ORIENTED_EDGE('',*,*,#13843,.T.);
#17920=ORIENTED_EDGE('',*,*,#13844,.T.);
#17921=ORIENTED_EDGE('',*,*,#13845,.T.);
#17922=ORIENTED_EDGE('',*,*,#13846,.T.);
#17923=ORIENTED_EDGE('',*,*,#13847,.T.);
#17924=ORIENTED_EDGE('',*,*,#13845,.F.);
#17925=ORIENTED_EDGE('',*,*,#13848,.T.);
#17926=ORIENTED_EDGE('',*,*,#13849,.F.);
#17927=ORIENTED_EDGE('',*,*,#13850,.F.);
#17928=ORIENTED_EDGE('',*,*,#13851,.T.);
#17929=ORIENTED_EDGE('',*,*,#13852,.F.);
#17930=ORIENTED_EDGE('',*,*,#13844,.F.);
#17931=ORIENTED_EDGE('',*,*,#13853,.F.);
#17932=ORIENTED_EDGE('',*,*,#13854,.F.);
#17933=ORIENTED_EDGE('',*,*,#13848,.F.);
#17934=ORIENTED_EDGE('',*,*,#13843,.F.);
#17935=ORIENTED_EDGE('',*,*,#13855,.T.);
#17936=ORIENTED_EDGE('',*,*,#13856,.T.);
#17937=ORIENTED_EDGE('',*,*,#13853,.T.);
#17938=ORIENTED_EDGE('',*,*,#13856,.F.);
#17939=ORIENTED_EDGE('',*,*,#13857,.T.);
#17940=ORIENTED_EDGE('',*,*,#13858,.T.);
#17941=ORIENTED_EDGE('',*,*,#13849,.T.);
#17942=ORIENTED_EDGE('',*,*,#13854,.T.);
#17943=ORIENTED_EDGE('',*,*,#13858,.F.);
#17944=ORIENTED_EDGE('',*,*,#13859,.T.);
#17945=ORIENTED_EDGE('',*,*,#13860,.F.);
#17946=ORIENTED_EDGE('',*,*,#13861,.F.);
#17947=ORIENTED_EDGE('',*,*,#13862,.T.);
#17948=ORIENTED_EDGE('',*,*,#13850,.T.);
#17949=ORIENTED_EDGE('',*,*,#13857,.F.);
#17950=ORIENTED_EDGE('',*,*,#13863,.F.);
#17951=ORIENTED_EDGE('',*,*,#13864,.F.);
#17952=ORIENTED_EDGE('',*,*,#13865,.F.);
#17953=ORIENTED_EDGE('',*,*,#13866,.F.);
#17954=ORIENTED_EDGE('',*,*,#13867,.F.);
#17955=ORIENTED_EDGE('',*,*,#13868,.F.);
#17956=ORIENTED_EDGE('',*,*,#13859,.F.);
#17957=ORIENTED_EDGE('',*,*,#13869,.T.);
#17958=ORIENTED_EDGE('',*,*,#13870,.T.);
#17959=ORIENTED_EDGE('',*,*,#13871,.T.);
#17960=ORIENTED_EDGE('',*,*,#13872,.T.);
#17961=ORIENTED_EDGE('',*,*,#13873,.T.);
#17962=ORIENTED_EDGE('',*,*,#13873,.F.);
#17963=ORIENTED_EDGE('',*,*,#13874,.F.);
#17964=ORIENTED_EDGE('',*,*,#13875,.F.);
#17965=ORIENTED_EDGE('',*,*,#13876,.F.);
#17966=ORIENTED_EDGE('',*,*,#13872,.F.);
#17967=ORIENTED_EDGE('',*,*,#13877,.F.);
#17968=ORIENTED_EDGE('',*,*,#13878,.T.);
#17969=ORIENTED_EDGE('',*,*,#13861,.T.);
#17970=ORIENTED_EDGE('',*,*,#13879,.F.);
#17971=ORIENTED_EDGE('',*,*,#13874,.T.);
#17972=ORIENTED_EDGE('',*,*,#13846,.F.);
#17973=ORIENTED_EDGE('',*,*,#13852,.T.);
#17974=ORIENTED_EDGE('',*,*,#13880,.T.);
#17975=ORIENTED_EDGE('',*,*,#13877,.T.);
#17976=ORIENTED_EDGE('',*,*,#13871,.F.);
#17977=ORIENTED_EDGE('',*,*,#13881,.T.);
#17978=ORIENTED_EDGE('',*,*,#13869,.F.);
#17979=ORIENTED_EDGE('',*,*,#13876,.T.);
#17980=ORIENTED_EDGE('',*,*,#13882,.T.);
#17981=ORIENTED_EDGE('',*,*,#13883,.T.);
#17982=ORIENTED_EDGE('',*,*,#13883,.F.);
#17983=ORIENTED_EDGE('',*,*,#13867,.T.);
#17984=ORIENTED_EDGE('',*,*,#13884,.F.);
#17985=ORIENTED_EDGE('',*,*,#13885,.T.);
#17986=ORIENTED_EDGE('',*,*,#13882,.F.);
#17987=ORIENTED_EDGE('',*,*,#13875,.T.);
#17988=ORIENTED_EDGE('',*,*,#13879,.T.);
#17989=ORIENTED_EDGE('',*,*,#13860,.T.);
#17990=ORIENTED_EDGE('',*,*,#13868,.T.);
#17991=ORIENTED_EDGE('',*,*,#13886,.T.);
#17992=ORIENTED_EDGE('',*,*,#13887,.T.);
#17993=ORIENTED_EDGE('',*,*,#13888,.T.);
#17994=ORIENTED_EDGE('',*,*,#13887,.F.);
#17995=ORIENTED_EDGE('',*,*,#13889,.F.);
#17996=ORIENTED_EDGE('',*,*,#13890,.F.);
#17997=ORIENTED_EDGE('',*,*,#13891,.F.);
#17998=ORIENTED_EDGE('',*,*,#13892,.F.);
#17999=ORIENTED_EDGE('',*,*,#13893,.F.);
#18000=ORIENTED_EDGE('',*,*,#13894,.F.);
#18001=ORIENTED_EDGE('',*,*,#13895,.F.);
#18002=ORIENTED_EDGE('',*,*,#13886,.F.);
#18003=ORIENTED_EDGE('',*,*,#13888,.F.);
#18004=ORIENTED_EDGE('',*,*,#13896,.T.);
#18005=ORIENTED_EDGE('',*,*,#13897,.F.);
#18006=ORIENTED_EDGE('',*,*,#13896,.F.);
#18007=ORIENTED_EDGE('',*,*,#13893,.T.);
#18008=ORIENTED_EDGE('',*,*,#13898,.T.);
#18009=ORIENTED_EDGE('',*,*,#13899,.T.);
#18010=ORIENTED_EDGE('',*,*,#13898,.F.);
#18011=ORIENTED_EDGE('',*,*,#13899,.F.);
#18012=ORIENTED_EDGE('',*,*,#13900,.T.);
#18013=ORIENTED_EDGE('',*,*,#13901,.F.);
#18014=ORIENTED_EDGE('',*,*,#13900,.F.);
#18015=ORIENTED_EDGE('',*,*,#13895,.T.);
#18016=ORIENTED_EDGE('',*,*,#13902,.T.);
#18017=ORIENTED_EDGE('',*,*,#13903,.T.);
#18018=ORIENTED_EDGE('',*,*,#13902,.F.);
#18019=ORIENTED_EDGE('',*,*,#13903,.F.);
#18020=ORIENTED_EDGE('',*,*,#13904,.T.);
#18021=ORIENTED_EDGE('',*,*,#13905,.F.);
#18022=ORIENTED_EDGE('',*,*,#13904,.F.);
#18023=ORIENTED_EDGE('',*,*,#13894,.T.);
#18024=ORIENTED_EDGE('',*,*,#13906,.T.);
#18025=ORIENTED_EDGE('',*,*,#13907,.T.);
#18026=ORIENTED_EDGE('',*,*,#13906,.F.);
#18027=ORIENTED_EDGE('',*,*,#13907,.F.);
#18028=ORIENTED_EDGE('',*,*,#13908,.T.);
#18029=ORIENTED_EDGE('',*,*,#13909,.F.);
#18030=ORIENTED_EDGE('',*,*,#13908,.F.);
#18031=ORIENTED_EDGE('',*,*,#13910,.T.);
#18032=ORIENTED_EDGE('',*,*,#13911,.T.);
#18033=ORIENTED_EDGE('',*,*,#13909,.T.);
#18034=ORIENTED_EDGE('',*,*,#13911,.F.);
#18035=ORIENTED_EDGE('',*,*,#13912,.F.);
#18036=ORIENTED_EDGE('',*,*,#13913,.F.);
#18037=ORIENTED_EDGE('',*,*,#13914,.F.);
#18038=ORIENTED_EDGE('',*,*,#13915,.F.);
#18039=ORIENTED_EDGE('',*,*,#13916,.F.);
#18040=ORIENTED_EDGE('',*,*,#13917,.F.);
#18041=ORIENTED_EDGE('',*,*,#13918,.F.);
#18042=ORIENTED_EDGE('',*,*,#13910,.F.);
#18043=ORIENTED_EDGE('',*,*,#13916,.T.);
#18044=ORIENTED_EDGE('',*,*,#13919,.T.);
#18045=ORIENTED_EDGE('',*,*,#13905,.T.);
#18046=ORIENTED_EDGE('',*,*,#13919,.F.);
#18047=ORIENTED_EDGE('',*,*,#13918,.T.);
#18048=ORIENTED_EDGE('',*,*,#13920,.T.);
#18049=ORIENTED_EDGE('',*,*,#13901,.T.);
#18050=ORIENTED_EDGE('',*,*,#13920,.F.);
#18051=ORIENTED_EDGE('',*,*,#13917,.T.);
#18052=ORIENTED_EDGE('',*,*,#13921,.T.);
#18053=ORIENTED_EDGE('',*,*,#13897,.T.);
#18054=ORIENTED_EDGE('',*,*,#13921,.F.);
#18055=ORIENTED_EDGE('',*,*,#13922,.T.);
#18056=ORIENTED_EDGE('',*,*,#13923,.T.);
#18057=ORIENTED_EDGE('',*,*,#13924,.T.);
#18058=ORIENTED_EDGE('',*,*,#13923,.F.);
#18059=ORIENTED_EDGE('',*,*,#13925,.F.);
#18060=ORIENTED_EDGE('',*,*,#13926,.F.);
#18061=ORIENTED_EDGE('',*,*,#13927,.F.);
#18062=ORIENTED_EDGE('',*,*,#13928,.F.);
#18063=ORIENTED_EDGE('',*,*,#13929,.F.);
#18064=ORIENTED_EDGE('',*,*,#13930,.F.);
#18065=ORIENTED_EDGE('',*,*,#13931,.F.);
#18066=ORIENTED_EDGE('',*,*,#13922,.F.);
#18067=ORIENTED_EDGE('',*,*,#13932,.F.);
#18068=ORIENTED_EDGE('',*,*,#13933,.T.);
#18069=ORIENTED_EDGE('',*,*,#13924,.F.);
#18070=ORIENTED_EDGE('',*,*,#13933,.F.);
#18071=ORIENTED_EDGE('',*,*,#13929,.T.);
#18072=ORIENTED_EDGE('',*,*,#13934,.T.);
#18073=ORIENTED_EDGE('',*,*,#13935,.T.);
#18074=ORIENTED_EDGE('',*,*,#13934,.F.);
#18075=ORIENTED_EDGE('',*,*,#13936,.F.);
#18076=ORIENTED_EDGE('',*,*,#13937,.T.);
#18077=ORIENTED_EDGE('',*,*,#13935,.F.);
#18078=ORIENTED_EDGE('',*,*,#13937,.F.);
#18079=ORIENTED_EDGE('',*,*,#13931,.T.);
#18080=ORIENTED_EDGE('',*,*,#13938,.T.);
#18081=ORIENTED_EDGE('',*,*,#13939,.T.);
#18082=ORIENTED_EDGE('',*,*,#13938,.F.);
#18083=ORIENTED_EDGE('',*,*,#13940,.F.);
#18084=ORIENTED_EDGE('',*,*,#13941,.T.);
#18085=ORIENTED_EDGE('',*,*,#13939,.F.);
#18086=ORIENTED_EDGE('',*,*,#13941,.F.);
#18087=ORIENTED_EDGE('',*,*,#13930,.T.);
#18088=ORIENTED_EDGE('',*,*,#13942,.T.);
#18089=ORIENTED_EDGE('',*,*,#13943,.T.);
#18090=ORIENTED_EDGE('',*,*,#13942,.F.);
#18091=ORIENTED_EDGE('',*,*,#13944,.F.);
#18092=ORIENTED_EDGE('',*,*,#13945,.T.);
#18093=ORIENTED_EDGE('',*,*,#13943,.F.);
#18094=ORIENTED_EDGE('',*,*,#13945,.F.);
#18095=ORIENTED_EDGE('',*,*,#13946,.T.);
#18096=ORIENTED_EDGE('',*,*,#13947,.T.);
#18097=ORIENTED_EDGE('',*,*,#13948,.T.);
#18098=ORIENTED_EDGE('',*,*,#13949,.T.);
#18099=ORIENTED_EDGE('',*,*,#13950,.T.);
#18100=ORIENTED_EDGE('',*,*,#13951,.T.);
#18101=ORIENTED_EDGE('',*,*,#13952,.T.);
#18102=ORIENTED_EDGE('',*,*,#13953,.T.);
#18103=ORIENTED_EDGE('',*,*,#13954,.T.);
#18104=ORIENTED_EDGE('',*,*,#13953,.F.);
#18105=ORIENTED_EDGE('',*,*,#13955,.T.);
#18106=ORIENTED_EDGE('',*,*,#13949,.F.);
#18107=ORIENTED_EDGE('',*,*,#13956,.T.);
#18108=ORIENTED_EDGE('',*,*,#13946,.F.);
#18109=ORIENTED_EDGE('',*,*,#13957,.T.);
#18110=ORIENTED_EDGE('',*,*,#13951,.F.);
#18111=ORIENTED_EDGE('',*,*,#13958,.T.);
#18112=ORIENTED_EDGE('',*,*,#13955,.F.);
#18113=ORIENTED_EDGE('',*,*,#13952,.F.);
#18114=ORIENTED_EDGE('',*,*,#13957,.F.);
#18115=ORIENTED_EDGE('',*,*,#13959,.T.);
#18116=ORIENTED_EDGE('',*,*,#13960,.F.);
#18117=ORIENTED_EDGE('',*,*,#13961,.T.);
#18118=ORIENTED_EDGE('',*,*,#13962,.F.);
#18119=ORIENTED_EDGE('',*,*,#13963,.T.);
#18120=ORIENTED_EDGE('',*,*,#13964,.F.);
#18121=ORIENTED_EDGE('',*,*,#13965,.F.);
#18122=ORIENTED_EDGE('',*,*,#13966,.F.);
#18123=ORIENTED_EDGE('',*,*,#13967,.T.);
#18124=ORIENTED_EDGE('',*,*,#13954,.F.);
#18125=ORIENTED_EDGE('',*,*,#13956,.F.);
#18126=ORIENTED_EDGE('',*,*,#13948,.F.);
#18127=ORIENTED_EDGE('',*,*,#13968,.T.);
#18128=ORIENTED_EDGE('',*,*,#13969,.F.);
#18129=ORIENTED_EDGE('',*,*,#13970,.F.);
#18130=ORIENTED_EDGE('',*,*,#13971,.F.);
#18131=ORIENTED_EDGE('',*,*,#13972,.F.);
#18132=ORIENTED_EDGE('',*,*,#13973,.F.);
#18133=ORIENTED_EDGE('',*,*,#13968,.F.);
#18134=ORIENTED_EDGE('',*,*,#13947,.F.);
#18135=ORIENTED_EDGE('',*,*,#13958,.F.);
#18136=ORIENTED_EDGE('',*,*,#13974,.T.);
#18137=ORIENTED_EDGE('',*,*,#13975,.T.);
#18138=ORIENTED_EDGE('',*,*,#13944,.T.);
#18139=ORIENTED_EDGE('',*,*,#13975,.F.);
#18140=ORIENTED_EDGE('',*,*,#13976,.F.);
#18141=ORIENTED_EDGE('',*,*,#13977,.F.);
#18142=ORIENTED_EDGE('',*,*,#13978,.F.);
#18143=ORIENTED_EDGE('',*,*,#13979,.F.);
#18144=ORIENTED_EDGE('',*,*,#13980,.F.);
#18145=ORIENTED_EDGE('',*,*,#13981,.F.);
#18146=ORIENTED_EDGE('',*,*,#13982,.F.);
#18147=ORIENTED_EDGE('',*,*,#13974,.F.);
#18148=ORIENTED_EDGE('',*,*,#13980,.T.);
#18149=ORIENTED_EDGE('',*,*,#13983,.T.);
#18150=ORIENTED_EDGE('',*,*,#13940,.T.);
#18151=ORIENTED_EDGE('',*,*,#13983,.F.);
#18152=ORIENTED_EDGE('',*,*,#13982,.T.);
#18153=ORIENTED_EDGE('',*,*,#13984,.T.);
#18154=ORIENTED_EDGE('',*,*,#13936,.T.);
#18155=ORIENTED_EDGE('',*,*,#13984,.F.);
#18156=ORIENTED_EDGE('',*,*,#13981,.T.);
#18157=ORIENTED_EDGE('',*,*,#13985,.T.);
#18158=ORIENTED_EDGE('',*,*,#13932,.T.);
#18159=ORIENTED_EDGE('',*,*,#13985,.F.);
#18160=ORIENTED_EDGE('',*,*,#13986,.T.);
#18161=ORIENTED_EDGE('',*,*,#13987,.T.);
#18162=ORIENTED_EDGE('',*,*,#13988,.T.);
#18163=ORIENTED_EDGE('',*,*,#13989,.T.);
#18164=ORIENTED_EDGE('',*,*,#13986,.F.);
#18165=ORIENTED_EDGE('',*,*,#13990,.T.);
#18166=ORIENTED_EDGE('',*,*,#13991,.T.);
#18167=ORIENTED_EDGE('',*,*,#13992,.T.);
#18168=ORIENTED_EDGE('',*,*,#13993,.T.);
#18169=ORIENTED_EDGE('',*,*,#13960,.T.);
#18170=ORIENTED_EDGE('',*,*,#13991,.F.);
#18171=ORIENTED_EDGE('',*,*,#13994,.T.);
#18172=ORIENTED_EDGE('',*,*,#13993,.F.);
#18173=ORIENTED_EDGE('',*,*,#13995,.T.);
#18174=ORIENTED_EDGE('',*,*,#13996,.T.);
#18175=ORIENTED_EDGE('',*,*,#13997,.T.);
#18176=ORIENTED_EDGE('',*,*,#13998,.T.);
#18177=ORIENTED_EDGE('',*,*,#13999,.T.);
#18178=ORIENTED_EDGE('',*,*,#13996,.F.);
#18179=ORIENTED_EDGE('',*,*,#14000,.T.);
#18180=ORIENTED_EDGE('',*,*,#13998,.F.);
#18181=ORIENTED_EDGE('',*,*,#14001,.T.);
#18182=ORIENTED_EDGE('',*,*,#14002,.T.);
#18183=ORIENTED_EDGE('',*,*,#13912,.T.);
#18184=ORIENTED_EDGE('',*,*,#14003,.T.);
#18185=ORIENTED_EDGE('',*,*,#14004,.T.);
#18186=ORIENTED_EDGE('',*,*,#14002,.F.);
#18187=ORIENTED_EDGE('',*,*,#14005,.T.);
#18188=ORIENTED_EDGE('',*,*,#14003,.F.);
#18189=ORIENTED_EDGE('',*,*,#14006,.T.);
#18190=ORIENTED_EDGE('',*,*,#13988,.F.);
#18191=ORIENTED_EDGE('',*,*,#14007,.T.);
#18192=ORIENTED_EDGE('',*,*,#14004,.F.);
#18193=ORIENTED_EDGE('',*,*,#14008,.T.);
#18194=ORIENTED_EDGE('',*,*,#14009,.T.);
#18195=ORIENTED_EDGE('',*,*,#14010,.T.);
#18196=ORIENTED_EDGE('',*,*,#14011,.F.);
#18197=ORIENTED_EDGE('',*,*,#13913,.T.);
#18198=ORIENTED_EDGE('',*,*,#14007,.F.);
#18199=ORIENTED_EDGE('',*,*,#14012,.F.);
#18200=ORIENTED_EDGE('',*,*,#13866,.T.);
#18201=ORIENTED_EDGE('',*,*,#14008,.F.);
#18202=ORIENTED_EDGE('',*,*,#13987,.F.);
#18203=ORIENTED_EDGE('',*,*,#14013,.T.);
#18204=ORIENTED_EDGE('',*,*,#14014,.F.);
#18205=ORIENTED_EDGE('',*,*,#14015,.F.);
#18206=ORIENTED_EDGE('',*,*,#14016,.F.);
#18207=ORIENTED_EDGE('',*,*,#14017,.T.);
#18208=ORIENTED_EDGE('',*,*,#14018,.F.);
#18209=ORIENTED_EDGE('',*,*,#14019,.F.);
#18210=ORIENTED_EDGE('',*,*,#14020,.F.);
#18211=ORIENTED_EDGE('',*,*,#14021,.T.);
#18212=ORIENTED_EDGE('',*,*,#14022,.F.);
#18213=ORIENTED_EDGE('',*,*,#14023,.T.);
#18214=ORIENTED_EDGE('',*,*,#13884,.T.);
#18215=ORIENTED_EDGE('',*,*,#14012,.T.);
#18216=ORIENTED_EDGE('',*,*,#13989,.F.);
#18217=ORIENTED_EDGE('',*,*,#14006,.F.);
#18218=ORIENTED_EDGE('',*,*,#14005,.F.);
#18219=ORIENTED_EDGE('',*,*,#14001,.F.);
#18220=ORIENTED_EDGE('',*,*,#14000,.F.);
#18221=ORIENTED_EDGE('',*,*,#13995,.F.);
#18222=ORIENTED_EDGE('',*,*,#13994,.F.);
#18223=ORIENTED_EDGE('',*,*,#13990,.F.);
#18224=ORIENTED_EDGE('',*,*,#14024,.F.);
#18225=ORIENTED_EDGE('',*,*,#14025,.F.);
#18226=ORIENTED_EDGE('',*,*,#14026,.F.);
#18227=ORIENTED_EDGE('',*,*,#14027,.F.);
#18228=ORIENTED_EDGE('',*,*,#14028,.F.);
#18229=ORIENTED_EDGE('',*,*,#14029,.F.);
#18230=ORIENTED_EDGE('',*,*,#14030,.F.);
#18231=ORIENTED_EDGE('',*,*,#14031,.F.);
#18232=ORIENTED_EDGE('',*,*,#14032,.T.);
#18233=ORIENTED_EDGE('',*,*,#14022,.T.);
#18234=ORIENTED_EDGE('',*,*,#14033,.T.);
#18235=ORIENTED_EDGE('',*,*,#14034,.T.);
#18236=ORIENTED_EDGE('',*,*,#14032,.F.);
#18237=ORIENTED_EDGE('',*,*,#14035,.T.);
#18238=ORIENTED_EDGE('',*,*,#14036,.T.);
#18239=ORIENTED_EDGE('',*,*,#14037,.T.);
#18240=ORIENTED_EDGE('',*,*,#14038,.T.);
#18241=ORIENTED_EDGE('',*,*,#14011,.T.);
#18242=ORIENTED_EDGE('',*,*,#14036,.F.);
#18243=ORIENTED_EDGE('',*,*,#14039,.T.);
#18244=ORIENTED_EDGE('',*,*,#14038,.F.);
#18245=ORIENTED_EDGE('',*,*,#14040,.T.);
#18246=ORIENTED_EDGE('',*,*,#14041,.T.);
#18247=ORIENTED_EDGE('',*,*,#13914,.T.);
#18248=ORIENTED_EDGE('',*,*,#14042,.T.);
#18249=ORIENTED_EDGE('',*,*,#14043,.T.);
#18250=ORIENTED_EDGE('',*,*,#14041,.F.);
#18251=ORIENTED_EDGE('',*,*,#14044,.T.);
#18252=ORIENTED_EDGE('',*,*,#14042,.F.);
#18253=ORIENTED_EDGE('',*,*,#14045,.T.);
#18254=ORIENTED_EDGE('',*,*,#14046,.T.);
#18255=ORIENTED_EDGE('',*,*,#14047,.T.);
#18256=ORIENTED_EDGE('',*,*,#14048,.T.);
#18257=ORIENTED_EDGE('',*,*,#13962,.T.);
#18258=ORIENTED_EDGE('',*,*,#14046,.F.);
#18259=ORIENTED_EDGE('',*,*,#14049,.T.);
#18260=ORIENTED_EDGE('',*,*,#14048,.F.);
#18261=ORIENTED_EDGE('',*,*,#14050,.T.);
#18262=ORIENTED_EDGE('',*,*,#14033,.F.);
#18263=ORIENTED_EDGE('',*,*,#14051,.T.);
#18264=ORIENTED_EDGE('',*,*,#13997,.F.);
#18265=ORIENTED_EDGE('',*,*,#14052,.F.);
#18266=ORIENTED_EDGE('',*,*,#14047,.F.);
#18267=ORIENTED_EDGE('',*,*,#13961,.F.);
#18268=ORIENTED_EDGE('',*,*,#13950,.F.);
#18269=ORIENTED_EDGE('',*,*,#13967,.F.);
#18270=ORIENTED_EDGE('',*,*,#14053,.F.);
#18271=ORIENTED_EDGE('',*,*,#13963,.F.);
#18272=ORIENTED_EDGE('',*,*,#14051,.F.);
#18273=ORIENTED_EDGE('',*,*,#14021,.F.);
#18274=ORIENTED_EDGE('',*,*,#14054,.F.);
#18275=ORIENTED_EDGE('',*,*,#14017,.F.);
#18276=ORIENTED_EDGE('',*,*,#14055,.F.);
#18277=ORIENTED_EDGE('',*,*,#14013,.F.);
#18278=ORIENTED_EDGE('',*,*,#13992,.F.);
#18279=ORIENTED_EDGE('',*,*,#13959,.F.);
#18280=ORIENTED_EDGE('',*,*,#14056,.T.);
#18281=ORIENTED_EDGE('',*,*,#14057,.T.);
#18282=ORIENTED_EDGE('',*,*,#14058,.T.);
#18283=ORIENTED_EDGE('',*,*,#14059,.T.);
#18284=ORIENTED_EDGE('',*,*,#14060,.T.);
#18285=ORIENTED_EDGE('',*,*,#14061,.T.);
#18286=ORIENTED_EDGE('',*,*,#14062,.T.);
#18287=ORIENTED_EDGE('',*,*,#14063,.T.);
#18288=ORIENTED_EDGE('',*,*,#14064,.T.);
#18289=ORIENTED_EDGE('',*,*,#14065,.T.);
#18290=ORIENTED_EDGE('',*,*,#14066,.T.);
#18291=ORIENTED_EDGE('',*,*,#14067,.T.);
#18292=ORIENTED_EDGE('',*,*,#14068,.T.);
#18293=ORIENTED_EDGE('',*,*,#14069,.T.);
#18294=ORIENTED_EDGE('',*,*,#14070,.T.);
#18295=ORIENTED_EDGE('',*,*,#14071,.T.);
#18296=ORIENTED_EDGE('',*,*,#14072,.T.);
#18297=ORIENTED_EDGE('',*,*,#14073,.T.);
#18298=ORIENTED_EDGE('',*,*,#14074,.T.);
#18299=ORIENTED_EDGE('',*,*,#14075,.T.);
#18300=ORIENTED_EDGE('',*,*,#14076,.T.);
#18301=ORIENTED_EDGE('',*,*,#14077,.T.);
#18302=ORIENTED_EDGE('',*,*,#14078,.T.);
#18303=ORIENTED_EDGE('',*,*,#14079,.T.);
#18304=ORIENTED_EDGE('',*,*,#14080,.T.);
#18305=ORIENTED_EDGE('',*,*,#14081,.T.);
#18306=ORIENTED_EDGE('',*,*,#14082,.T.);
#18307=ORIENTED_EDGE('',*,*,#14083,.T.);
#18308=ORIENTED_EDGE('',*,*,#14084,.T.);
#18309=ORIENTED_EDGE('',*,*,#14085,.T.);
#18310=ORIENTED_EDGE('',*,*,#14086,.T.);
#18311=ORIENTED_EDGE('',*,*,#14087,.T.);
#18312=ORIENTED_EDGE('',*,*,#14088,.T.);
#18313=ORIENTED_EDGE('',*,*,#14089,.T.);
#18314=ORIENTED_EDGE('',*,*,#14090,.T.);
#18315=ORIENTED_EDGE('',*,*,#14091,.T.);
#18316=ORIENTED_EDGE('',*,*,#14092,.T.);
#18317=ORIENTED_EDGE('',*,*,#14093,.T.);
#18318=ORIENTED_EDGE('',*,*,#14094,.T.);
#18319=ORIENTED_EDGE('',*,*,#14095,.T.);
#18320=ORIENTED_EDGE('',*,*,#14096,.T.);
#18321=ORIENTED_EDGE('',*,*,#14097,.T.);
#18322=ORIENTED_EDGE('',*,*,#14098,.T.);
#18323=ORIENTED_EDGE('',*,*,#14099,.T.);
#18324=ORIENTED_EDGE('',*,*,#14100,.T.);
#18325=ORIENTED_EDGE('',*,*,#14101,.T.);
#18326=ORIENTED_EDGE('',*,*,#14102,.T.);
#18327=ORIENTED_EDGE('',*,*,#14103,.T.);
#18328=ORIENTED_EDGE('',*,*,#14104,.T.);
#18329=ORIENTED_EDGE('',*,*,#14105,.T.);
#18330=ORIENTED_EDGE('',*,*,#14106,.T.);
#18331=ORIENTED_EDGE('',*,*,#14107,.T.);
#18332=ORIENTED_EDGE('',*,*,#14108,.T.);
#18333=ORIENTED_EDGE('',*,*,#14109,.T.);
#18334=ORIENTED_EDGE('',*,*,#14110,.T.);
#18335=ORIENTED_EDGE('',*,*,#14111,.T.);
#18336=ORIENTED_EDGE('',*,*,#14112,.T.);
#18337=ORIENTED_EDGE('',*,*,#14113,.T.);
#18338=ORIENTED_EDGE('',*,*,#14114,.T.);
#18339=ORIENTED_EDGE('',*,*,#14115,.T.);
#18340=ORIENTED_EDGE('',*,*,#14116,.T.);
#18341=ORIENTED_EDGE('',*,*,#14117,.T.);
#18342=ORIENTED_EDGE('',*,*,#14118,.T.);
#18343=ORIENTED_EDGE('',*,*,#14034,.F.);
#18344=ORIENTED_EDGE('',*,*,#14050,.F.);
#18345=ORIENTED_EDGE('',*,*,#14049,.F.);
#18346=ORIENTED_EDGE('',*,*,#14045,.F.);
#18347=ORIENTED_EDGE('',*,*,#14044,.F.);
#18348=ORIENTED_EDGE('',*,*,#14040,.F.);
#18349=ORIENTED_EDGE('',*,*,#14039,.F.);
#18350=ORIENTED_EDGE('',*,*,#14035,.F.);
#18351=ORIENTED_EDGE('',*,*,#14119,.F.);
#18352=ORIENTED_EDGE('',*,*,#14120,.F.);
#18353=ORIENTED_EDGE('',*,*,#14121,.F.);
#18354=ORIENTED_EDGE('',*,*,#14122,.F.);
#18355=ORIENTED_EDGE('',*,*,#14123,.F.);
#18356=ORIENTED_EDGE('',*,*,#14124,.F.);
#18357=ORIENTED_EDGE('',*,*,#14125,.F.);
#18358=ORIENTED_EDGE('',*,*,#14126,.F.);
#18359=ORIENTED_EDGE('',*,*,#14127,.T.);
#18360=ORIENTED_EDGE('',*,*,#14128,.T.);
#18361=ORIENTED_EDGE('',*,*,#14129,.T.);
#18362=ORIENTED_EDGE('',*,*,#14130,.T.);
#18363=ORIENTED_EDGE('',*,*,#14054,.T.);
#18364=ORIENTED_EDGE('',*,*,#14131,.T.);
#18365=ORIENTED_EDGE('',*,*,#14019,.T.);
#18366=ORIENTED_EDGE('',*,*,#14132,.T.);
#18367=ORIENTED_EDGE('',*,*,#14133,.T.);
#18368=ORIENTED_EDGE('',*,*,#14132,.F.);
#18369=ORIENTED_EDGE('',*,*,#14018,.T.);
#18370=ORIENTED_EDGE('',*,*,#14130,.F.);
#18371=ORIENTED_EDGE('',*,*,#14134,.T.);
#18372=ORIENTED_EDGE('',*,*,#14127,.F.);
#18373=ORIENTED_EDGE('',*,*,#14020,.T.);
#18374=ORIENTED_EDGE('',*,*,#14131,.F.);
#18375=ORIENTED_EDGE('',*,*,#14135,.T.);
#18376=ORIENTED_EDGE('',*,*,#14133,.F.);
#18377=ORIENTED_EDGE('',*,*,#14134,.F.);
#18378=ORIENTED_EDGE('',*,*,#14129,.F.);
#18379=ORIENTED_EDGE('',*,*,#14136,.T.);
#18380=ORIENTED_EDGE('',*,*,#14137,.F.);
#18381=ORIENTED_EDGE('',*,*,#14138,.F.);
#18382=ORIENTED_EDGE('',*,*,#14139,.F.);
#18383=ORIENTED_EDGE('',*,*,#14140,.F.);
#18384=ORIENTED_EDGE('',*,*,#14141,.F.);
#18385=ORIENTED_EDGE('',*,*,#14136,.F.);
#18386=ORIENTED_EDGE('',*,*,#14128,.F.);
#18387=ORIENTED_EDGE('',*,*,#14135,.F.);
#18388=ORIENTED_EDGE('',*,*,#14142,.T.);
#18389=ORIENTED_EDGE('',*,*,#14143,.T.);
#18390=ORIENTED_EDGE('',*,*,#14144,.T.);
#18391=ORIENTED_EDGE('',*,*,#14145,.T.);
#18392=ORIENTED_EDGE('',*,*,#14053,.T.);
#18393=ORIENTED_EDGE('',*,*,#14146,.T.);
#18394=ORIENTED_EDGE('',*,*,#13965,.T.);
#18395=ORIENTED_EDGE('',*,*,#14147,.T.);
#18396=ORIENTED_EDGE('',*,*,#14148,.T.);
#18397=ORIENTED_EDGE('',*,*,#14147,.F.);
#18398=ORIENTED_EDGE('',*,*,#13964,.T.);
#18399=ORIENTED_EDGE('',*,*,#14145,.F.);
#18400=ORIENTED_EDGE('',*,*,#14149,.T.);
#18401=ORIENTED_EDGE('',*,*,#14142,.F.);
#18402=ORIENTED_EDGE('',*,*,#13966,.T.);
#18403=ORIENTED_EDGE('',*,*,#14146,.F.);
#18404=ORIENTED_EDGE('',*,*,#14150,.T.);
#18405=ORIENTED_EDGE('',*,*,#14148,.F.);
#18406=ORIENTED_EDGE('',*,*,#14149,.F.);
#18407=ORIENTED_EDGE('',*,*,#14144,.F.);
#18408=ORIENTED_EDGE('',*,*,#14151,.T.);
#18409=ORIENTED_EDGE('',*,*,#14152,.F.);
#18410=ORIENTED_EDGE('',*,*,#14153,.F.);
#18411=ORIENTED_EDGE('',*,*,#14154,.F.);
#18412=ORIENTED_EDGE('',*,*,#14155,.F.);
#18413=ORIENTED_EDGE('',*,*,#14156,.F.);
#18414=ORIENTED_EDGE('',*,*,#14151,.F.);
#18415=ORIENTED_EDGE('',*,*,#14143,.F.);
#18416=ORIENTED_EDGE('',*,*,#14150,.F.);
#18417=ORIENTED_EDGE('',*,*,#14157,.T.);
#18418=ORIENTED_EDGE('',*,*,#14158,.T.);
#18419=ORIENTED_EDGE('',*,*,#14159,.T.);
#18420=ORIENTED_EDGE('',*,*,#14119,.T.);
#18421=ORIENTED_EDGE('',*,*,#14160,.T.);
#18422=ORIENTED_EDGE('',*,*,#14161,.T.);
#18423=ORIENTED_EDGE('',*,*,#14157,.F.);
#18424=ORIENTED_EDGE('',*,*,#14126,.T.);
#18425=ORIENTED_EDGE('',*,*,#14162,.T.);
#18426=ORIENTED_EDGE('',*,*,#14163,.T.);
#18427=ORIENTED_EDGE('',*,*,#14160,.F.);
#18428=ORIENTED_EDGE('',*,*,#14125,.T.);
#18429=ORIENTED_EDGE('',*,*,#14164,.T.);
#18430=ORIENTED_EDGE('',*,*,#14165,.T.);
#18431=ORIENTED_EDGE('',*,*,#14162,.F.);
#18432=ORIENTED_EDGE('',*,*,#14124,.T.);
#18433=ORIENTED_EDGE('',*,*,#14166,.T.);
#18434=ORIENTED_EDGE('',*,*,#13889,.T.);
#18435=ORIENTED_EDGE('',*,*,#14164,.F.);
#18436=ORIENTED_EDGE('',*,*,#14123,.T.);
#18437=ORIENTED_EDGE('',*,*,#14167,.T.);
#18438=ORIENTED_EDGE('',*,*,#14168,.T.);
#18439=ORIENTED_EDGE('',*,*,#14166,.F.);
#18440=ORIENTED_EDGE('',*,*,#14122,.T.);
#18441=ORIENTED_EDGE('',*,*,#14169,.T.);
#18442=ORIENTED_EDGE('',*,*,#14170,.T.);
#18443=ORIENTED_EDGE('',*,*,#14167,.F.);
#18444=ORIENTED_EDGE('',*,*,#14121,.T.);
#18445=ORIENTED_EDGE('',*,*,#14159,.F.);
#18446=ORIENTED_EDGE('',*,*,#14171,.T.);
#18447=ORIENTED_EDGE('',*,*,#14169,.F.);
#18448=ORIENTED_EDGE('',*,*,#14120,.T.);
#18449=ORIENTED_EDGE('',*,*,#14168,.F.);
#18450=ORIENTED_EDGE('',*,*,#14172,.T.);
#18451=ORIENTED_EDGE('',*,*,#14173,.F.);
#18452=ORIENTED_EDGE('',*,*,#13890,.T.);
#18453=ORIENTED_EDGE('',*,*,#14170,.F.);
#18454=ORIENTED_EDGE('',*,*,#14174,.F.);
#18455=ORIENTED_EDGE('',*,*,#14175,.F.);
#18456=ORIENTED_EDGE('',*,*,#14172,.F.);
#18457=ORIENTED_EDGE('',*,*,#14171,.F.);
#18458=ORIENTED_EDGE('',*,*,#14176,.T.);
#18459=ORIENTED_EDGE('',*,*,#14177,.F.);
#18460=ORIENTED_EDGE('',*,*,#14178,.F.);
#18461=ORIENTED_EDGE('',*,*,#14179,.F.);
#18462=ORIENTED_EDGE('',*,*,#14180,.F.);
#18463=ORIENTED_EDGE('',*,*,#14181,.F.);
#18464=ORIENTED_EDGE('',*,*,#14182,.F.);
#18465=ORIENTED_EDGE('',*,*,#14183,.T.);
#18466=ORIENTED_EDGE('',*,*,#14184,.F.);
#18467=ORIENTED_EDGE('',*,*,#14185,.F.);
#18468=ORIENTED_EDGE('',*,*,#14186,.F.);
#18469=ORIENTED_EDGE('',*,*,#14187,.F.);
#18470=ORIENTED_EDGE('',*,*,#14188,.F.);
#18471=ORIENTED_EDGE('',*,*,#14189,.F.);
#18472=ORIENTED_EDGE('',*,*,#14190,.T.);
#18473=ORIENTED_EDGE('',*,*,#14191,.F.);
#18474=ORIENTED_EDGE('',*,*,#14174,.T.);
#18475=ORIENTED_EDGE('',*,*,#14158,.F.);
#18476=ORIENTED_EDGE('',*,*,#14192,.F.);
#18477=ORIENTED_EDGE('',*,*,#14193,.F.);
#18478=ORIENTED_EDGE('',*,*,#14194,.F.);
#18479=ORIENTED_EDGE('',*,*,#14195,.F.);
#18480=ORIENTED_EDGE('',*,*,#14196,.F.);
#18481=ORIENTED_EDGE('',*,*,#14197,.F.);
#18482=ORIENTED_EDGE('',*,*,#14190,.F.);
#18483=ORIENTED_EDGE('',*,*,#14198,.F.);
#18484=ORIENTED_EDGE('',*,*,#14183,.F.);
#18485=ORIENTED_EDGE('',*,*,#14199,.F.);
#18486=ORIENTED_EDGE('',*,*,#14176,.F.);
#18487=ORIENTED_EDGE('',*,*,#14200,.T.);
#18488=ORIENTED_EDGE('',*,*,#14139,.T.);
#18489=ORIENTED_EDGE('',*,*,#14201,.F.);
#18490=ORIENTED_EDGE('',*,*,#14180,.T.);
#18491=ORIENTED_EDGE('',*,*,#14179,.T.);
#18492=ORIENTED_EDGE('',*,*,#14178,.T.);
#18493=ORIENTED_EDGE('',*,*,#14202,.T.);
#18494=ORIENTED_EDGE('',*,*,#14137,.T.);
#18495=ORIENTED_EDGE('',*,*,#14141,.T.);
#18496=ORIENTED_EDGE('',*,*,#14203,.T.);
#18497=ORIENTED_EDGE('',*,*,#14199,.T.);
#18498=ORIENTED_EDGE('',*,*,#14202,.F.);
#18499=ORIENTED_EDGE('',*,*,#14182,.T.);
#18500=ORIENTED_EDGE('',*,*,#14181,.T.);
#18501=ORIENTED_EDGE('',*,*,#14201,.T.);
#18502=ORIENTED_EDGE('',*,*,#14138,.T.);
#18503=ORIENTED_EDGE('',*,*,#14200,.F.);
#18504=ORIENTED_EDGE('',*,*,#14177,.T.);
#18505=ORIENTED_EDGE('',*,*,#14203,.F.);
#18506=ORIENTED_EDGE('',*,*,#14140,.T.);
#18507=ORIENTED_EDGE('',*,*,#14204,.T.);
#18508=ORIENTED_EDGE('',*,*,#14024,.T.);
#18509=ORIENTED_EDGE('',*,*,#14205,.T.);
#18510=ORIENTED_EDGE('',*,*,#14197,.T.);
#18511=ORIENTED_EDGE('',*,*,#14204,.F.);
#18512=ORIENTED_EDGE('',*,*,#14206,.T.);
#18513=ORIENTED_EDGE('',*,*,#14207,.T.);
#18514=ORIENTED_EDGE('',*,*,#14025,.T.);
#18515=ORIENTED_EDGE('',*,*,#14208,.T.);
#18516=ORIENTED_EDGE('',*,*,#14026,.T.);
#18517=ORIENTED_EDGE('',*,*,#14207,.F.);
#18518=ORIENTED_EDGE('',*,*,#14209,.T.);
#18519=ORIENTED_EDGE('',*,*,#14208,.F.);
#18520=ORIENTED_EDGE('',*,*,#14210,.T.);
#18521=ORIENTED_EDGE('',*,*,#14211,.T.);
#18522=ORIENTED_EDGE('',*,*,#14027,.T.);
#18523=ORIENTED_EDGE('',*,*,#14212,.T.);
#18524=ORIENTED_EDGE('',*,*,#14028,.T.);
#18525=ORIENTED_EDGE('',*,*,#14211,.F.);
#18526=ORIENTED_EDGE('',*,*,#13891,.T.);
#18527=ORIENTED_EDGE('',*,*,#14212,.F.);
#18528=ORIENTED_EDGE('',*,*,#14173,.T.);
#18529=ORIENTED_EDGE('',*,*,#14213,.T.);
#18530=ORIENTED_EDGE('',*,*,#14029,.T.);
#18531=ORIENTED_EDGE('',*,*,#14214,.T.);
#18532=ORIENTED_EDGE('',*,*,#14030,.T.);
#18533=ORIENTED_EDGE('',*,*,#14213,.F.);
#18534=ORIENTED_EDGE('',*,*,#14175,.T.);
#18535=ORIENTED_EDGE('',*,*,#14214,.F.);
#18536=ORIENTED_EDGE('',*,*,#14191,.T.);
#18537=ORIENTED_EDGE('',*,*,#14205,.F.);
#18538=ORIENTED_EDGE('',*,*,#14031,.T.);
#18539=ORIENTED_EDGE('',*,*,#14165,.F.);
#18540=ORIENTED_EDGE('',*,*,#13892,.T.);
#18541=ORIENTED_EDGE('',*,*,#14210,.F.);
#18542=ORIENTED_EDGE('',*,*,#14215,.T.);
#18543=ORIENTED_EDGE('',*,*,#14163,.F.);
#18544=ORIENTED_EDGE('',*,*,#14215,.F.);
#18545=ORIENTED_EDGE('',*,*,#14209,.F.);
#18546=ORIENTED_EDGE('',*,*,#14216,.F.);
#18547=ORIENTED_EDGE('',*,*,#14161,.F.);
#18548=ORIENTED_EDGE('',*,*,#14216,.T.);
#18549=ORIENTED_EDGE('',*,*,#14206,.F.);
#18550=ORIENTED_EDGE('',*,*,#14196,.T.);
#18551=ORIENTED_EDGE('',*,*,#14217,.F.);
#18552=ORIENTED_EDGE('',*,*,#14218,.F.);
#18553=ORIENTED_EDGE('',*,*,#14219,.F.);
#18554=ORIENTED_EDGE('',*,*,#14220,.F.);
#18555=ORIENTED_EDGE('',*,*,#14221,.F.);
#18556=ORIENTED_EDGE('',*,*,#14222,.F.);
#18557=ORIENTED_EDGE('',*,*,#14194,.T.);
#18558=ORIENTED_EDGE('',*,*,#14223,.F.);
#18559=ORIENTED_EDGE('',*,*,#14224,.F.);
#18560=ORIENTED_EDGE('',*,*,#14225,.F.);
#18561=ORIENTED_EDGE('',*,*,#14226,.F.);
#18562=ORIENTED_EDGE('',*,*,#14227,.F.);
#18563=ORIENTED_EDGE('',*,*,#14228,.F.);
#18564=ORIENTED_EDGE('',*,*,#14192,.T.);
#18565=ORIENTED_EDGE('',*,*,#14229,.T.);
#18566=ORIENTED_EDGE('',*,*,#13971,.T.);
#18567=ORIENTED_EDGE('',*,*,#14230,.F.);
#18568=ORIENTED_EDGE('',*,*,#14220,.T.);
#18569=ORIENTED_EDGE('',*,*,#14219,.T.);
#18570=ORIENTED_EDGE('',*,*,#14218,.T.);
#18571=ORIENTED_EDGE('',*,*,#14231,.T.);
#18572=ORIENTED_EDGE('',*,*,#13969,.T.);
#18573=ORIENTED_EDGE('',*,*,#13973,.T.);
#18574=ORIENTED_EDGE('',*,*,#14232,.T.);
#18575=ORIENTED_EDGE('',*,*,#14195,.T.);
#18576=ORIENTED_EDGE('',*,*,#14231,.F.);
#18577=ORIENTED_EDGE('',*,*,#14222,.T.);
#18578=ORIENTED_EDGE('',*,*,#14221,.T.);
#18579=ORIENTED_EDGE('',*,*,#14230,.T.);
#18580=ORIENTED_EDGE('',*,*,#13970,.T.);
#18581=ORIENTED_EDGE('',*,*,#14229,.F.);
#18582=ORIENTED_EDGE('',*,*,#14217,.T.);
#18583=ORIENTED_EDGE('',*,*,#14232,.F.);
#18584=ORIENTED_EDGE('',*,*,#13972,.T.);
#18585=ORIENTED_EDGE('',*,*,#14233,.T.);
#18586=ORIENTED_EDGE('',*,*,#14154,.T.);
#18587=ORIENTED_EDGE('',*,*,#14234,.F.);
#18588=ORIENTED_EDGE('',*,*,#14226,.T.);
#18589=ORIENTED_EDGE('',*,*,#14225,.T.);
#18590=ORIENTED_EDGE('',*,*,#14224,.T.);
#18591=ORIENTED_EDGE('',*,*,#14235,.T.);
#18592=ORIENTED_EDGE('',*,*,#14152,.T.);
#18593=ORIENTED_EDGE('',*,*,#14156,.T.);
#18594=ORIENTED_EDGE('',*,*,#14236,.T.);
#18595=ORIENTED_EDGE('',*,*,#14193,.T.);
#18596=ORIENTED_EDGE('',*,*,#14235,.F.);
#18597=ORIENTED_EDGE('',*,*,#14228,.T.);
#18598=ORIENTED_EDGE('',*,*,#14227,.T.);
#18599=ORIENTED_EDGE('',*,*,#14234,.T.);
#18600=ORIENTED_EDGE('',*,*,#14153,.T.);
#18601=ORIENTED_EDGE('',*,*,#14233,.F.);
#18602=ORIENTED_EDGE('',*,*,#14223,.T.);
#18603=ORIENTED_EDGE('',*,*,#14236,.F.);
#18604=ORIENTED_EDGE('',*,*,#14155,.T.);
#18605=ORIENTED_EDGE('',*,*,#14237,.T.);
#18606=ORIENTED_EDGE('',*,*,#14238,.T.);
#18607=ORIENTED_EDGE('',*,*,#14239,.T.);
#18608=ORIENTED_EDGE('',*,*,#14240,.T.);
#18609=ORIENTED_EDGE('',*,*,#14055,.T.);
#18610=ORIENTED_EDGE('',*,*,#14241,.T.);
#18611=ORIENTED_EDGE('',*,*,#14015,.T.);
#18612=ORIENTED_EDGE('',*,*,#14242,.T.);
#18613=ORIENTED_EDGE('',*,*,#14243,.T.);
#18614=ORIENTED_EDGE('',*,*,#14242,.F.);
#18615=ORIENTED_EDGE('',*,*,#14014,.T.);
#18616=ORIENTED_EDGE('',*,*,#14240,.F.);
#18617=ORIENTED_EDGE('',*,*,#14244,.T.);
#18618=ORIENTED_EDGE('',*,*,#14237,.F.);
#18619=ORIENTED_EDGE('',*,*,#14016,.T.);
#18620=ORIENTED_EDGE('',*,*,#14241,.F.);
#18621=ORIENTED_EDGE('',*,*,#14245,.T.);
#18622=ORIENTED_EDGE('',*,*,#14243,.F.);
#18623=ORIENTED_EDGE('',*,*,#14244,.F.);
#18624=ORIENTED_EDGE('',*,*,#14239,.F.);
#18625=ORIENTED_EDGE('',*,*,#14246,.T.);
#18626=ORIENTED_EDGE('',*,*,#14247,.F.);
#18627=ORIENTED_EDGE('',*,*,#14248,.F.);
#18628=ORIENTED_EDGE('',*,*,#14249,.F.);
#18629=ORIENTED_EDGE('',*,*,#14250,.F.);
#18630=ORIENTED_EDGE('',*,*,#14251,.F.);
#18631=ORIENTED_EDGE('',*,*,#14246,.F.);
#18632=ORIENTED_EDGE('',*,*,#14238,.F.);
#18633=ORIENTED_EDGE('',*,*,#14245,.F.);
#18634=ORIENTED_EDGE('',*,*,#14252,.T.);
#18635=ORIENTED_EDGE('',*,*,#14249,.T.);
#18636=ORIENTED_EDGE('',*,*,#14253,.F.);
#18637=ORIENTED_EDGE('',*,*,#14187,.T.);
#18638=ORIENTED_EDGE('',*,*,#14186,.T.);
#18639=ORIENTED_EDGE('',*,*,#14185,.T.);
#18640=ORIENTED_EDGE('',*,*,#14254,.T.);
#18641=ORIENTED_EDGE('',*,*,#14247,.T.);
#18642=ORIENTED_EDGE('',*,*,#14251,.T.);
#18643=ORIENTED_EDGE('',*,*,#14255,.T.);
#18644=ORIENTED_EDGE('',*,*,#14198,.T.);
#18645=ORIENTED_EDGE('',*,*,#14254,.F.);
#18646=ORIENTED_EDGE('',*,*,#14189,.T.);
#18647=ORIENTED_EDGE('',*,*,#14188,.T.);
#18648=ORIENTED_EDGE('',*,*,#14253,.T.);
#18649=ORIENTED_EDGE('',*,*,#14248,.T.);
#18650=ORIENTED_EDGE('',*,*,#14252,.F.);
#18651=ORIENTED_EDGE('',*,*,#14184,.T.);
#18652=ORIENTED_EDGE('',*,*,#14255,.F.);
#18653=ORIENTED_EDGE('',*,*,#14250,.T.);
#18654=ORIENTED_EDGE('',*,*,#14256,.T.);
#18655=ORIENTED_EDGE('',*,*,#14257,.T.);
#18656=ORIENTED_EDGE('',*,*,#14258,.T.);
#18657=ORIENTED_EDGE('',*,*,#14259,.T.);
#18658=ORIENTED_EDGE('',*,*,#14260,.T.);
#18659=ORIENTED_EDGE('',*,*,#14261,.T.);
#18660=ORIENTED_EDGE('',*,*,#14256,.F.);
#18661=ORIENTED_EDGE('',*,*,#14262,.T.);
#18662=ORIENTED_EDGE('',*,*,#14263,.T.);
#18663=ORIENTED_EDGE('',*,*,#14264,.T.);
#18664=ORIENTED_EDGE('',*,*,#14260,.F.);
#18665=ORIENTED_EDGE('',*,*,#14265,.T.);
#18666=ORIENTED_EDGE('',*,*,#14266,.T.);
#18667=ORIENTED_EDGE('',*,*,#14267,.T.);
#18668=ORIENTED_EDGE('',*,*,#14263,.F.);
#18669=ORIENTED_EDGE('',*,*,#14268,.T.);
#18670=ORIENTED_EDGE('',*,*,#14269,.T.);
#18671=ORIENTED_EDGE('',*,*,#14270,.T.);
#18672=ORIENTED_EDGE('',*,*,#14266,.F.);
#18673=ORIENTED_EDGE('',*,*,#14271,.T.);
#18674=ORIENTED_EDGE('',*,*,#14272,.T.);
#18675=ORIENTED_EDGE('',*,*,#13976,.T.);
#18676=ORIENTED_EDGE('',*,*,#14269,.F.);
#18677=ORIENTED_EDGE('',*,*,#14273,.T.);
#18678=ORIENTED_EDGE('',*,*,#14274,.T.);
#18679=ORIENTED_EDGE('',*,*,#14275,.T.);
#18680=ORIENTED_EDGE('',*,*,#14272,.F.);
#18681=ORIENTED_EDGE('',*,*,#14276,.T.);
#18682=ORIENTED_EDGE('',*,*,#14258,.F.);
#18683=ORIENTED_EDGE('',*,*,#14277,.T.);
#18684=ORIENTED_EDGE('',*,*,#14274,.F.);
#18685=ORIENTED_EDGE('',*,*,#14278,.T.);
#18686=ORIENTED_EDGE('',*,*,#14275,.F.);
#18687=ORIENTED_EDGE('',*,*,#14279,.T.);
#18688=ORIENTED_EDGE('',*,*,#14280,.T.);
#18689=ORIENTED_EDGE('',*,*,#14281,.T.);
#18690=ORIENTED_EDGE('',*,*,#14282,.F.);
#18691=ORIENTED_EDGE('',*,*,#13977,.T.);
#18692=ORIENTED_EDGE('',*,*,#14277,.F.);
#18693=ORIENTED_EDGE('',*,*,#14283,.F.);
#18694=ORIENTED_EDGE('',*,*,#14284,.T.);
#18695=ORIENTED_EDGE('',*,*,#14279,.F.);
#18696=ORIENTED_EDGE('',*,*,#14257,.F.);
#18697=ORIENTED_EDGE('',*,*,#14285,.T.);
#18698=ORIENTED_EDGE('',*,*,#14286,.F.);
#18699=ORIENTED_EDGE('',*,*,#14287,.F.);
#18700=ORIENTED_EDGE('',*,*,#14288,.F.);
#18701=ORIENTED_EDGE('',*,*,#14289,.T.);
#18702=ORIENTED_EDGE('',*,*,#14290,.F.);
#18703=ORIENTED_EDGE('',*,*,#14291,.F.);
#18704=ORIENTED_EDGE('',*,*,#14292,.F.);
#18705=ORIENTED_EDGE('',*,*,#14293,.T.);
#18706=ORIENTED_EDGE('',*,*,#14294,.F.);
#18707=ORIENTED_EDGE('',*,*,#14295,.T.);
#18708=ORIENTED_EDGE('',*,*,#14296,.T.);
#18709=ORIENTED_EDGE('',*,*,#14283,.T.);
#18710=ORIENTED_EDGE('',*,*,#14259,.F.);
#18711=ORIENTED_EDGE('',*,*,#14278,.F.);
#18712=ORIENTED_EDGE('',*,*,#14276,.F.);
#18713=ORIENTED_EDGE('',*,*,#14273,.F.);
#18714=ORIENTED_EDGE('',*,*,#14271,.F.);
#18715=ORIENTED_EDGE('',*,*,#14268,.F.);
#18716=ORIENTED_EDGE('',*,*,#14265,.F.);
#18717=ORIENTED_EDGE('',*,*,#14262,.F.);
#18718=ORIENTED_EDGE('',*,*,#14297,.F.);
#18719=ORIENTED_EDGE('',*,*,#14298,.F.);
#18720=ORIENTED_EDGE('',*,*,#14299,.F.);
#18721=ORIENTED_EDGE('',*,*,#14300,.F.);
#18722=ORIENTED_EDGE('',*,*,#14301,.F.);
#18723=ORIENTED_EDGE('',*,*,#14302,.F.);
#18724=ORIENTED_EDGE('',*,*,#14303,.F.);
#18725=ORIENTED_EDGE('',*,*,#14304,.F.);
#18726=ORIENTED_EDGE('',*,*,#14305,.T.);
#18727=ORIENTED_EDGE('',*,*,#14294,.T.);
#18728=ORIENTED_EDGE('',*,*,#14306,.T.);
#18729=ORIENTED_EDGE('',*,*,#14307,.T.);
#18730=ORIENTED_EDGE('',*,*,#14305,.F.);
#18731=ORIENTED_EDGE('',*,*,#14308,.T.);
#18732=ORIENTED_EDGE('',*,*,#14309,.T.);
#18733=ORIENTED_EDGE('',*,*,#14310,.T.);
#18734=ORIENTED_EDGE('',*,*,#14311,.T.);
#18735=ORIENTED_EDGE('',*,*,#14282,.T.);
#18736=ORIENTED_EDGE('',*,*,#14309,.F.);
#18737=ORIENTED_EDGE('',*,*,#14312,.T.);
#18738=ORIENTED_EDGE('',*,*,#14311,.F.);
#18739=ORIENTED_EDGE('',*,*,#14313,.T.);
#18740=ORIENTED_EDGE('',*,*,#14314,.T.);
#18741=ORIENTED_EDGE('',*,*,#13978,.T.);
#18742=ORIENTED_EDGE('',*,*,#14315,.T.);
#18743=ORIENTED_EDGE('',*,*,#14316,.T.);
#18744=ORIENTED_EDGE('',*,*,#14314,.F.);
#18745=ORIENTED_EDGE('',*,*,#14317,.T.);
#18746=ORIENTED_EDGE('',*,*,#14315,.F.);
#18747=ORIENTED_EDGE('',*,*,#14318,.T.);
#18748=ORIENTED_EDGE('',*,*,#14319,.T.);
#18749=ORIENTED_EDGE('',*,*,#14320,.T.);
#18750=ORIENTED_EDGE('',*,*,#14321,.T.);
#18751=ORIENTED_EDGE('',*,*,#14322,.T.);
#18752=ORIENTED_EDGE('',*,*,#14319,.F.);
#18753=ORIENTED_EDGE('',*,*,#14323,.T.);
#18754=ORIENTED_EDGE('',*,*,#14321,.F.);
#18755=ORIENTED_EDGE('',*,*,#14324,.T.);
#18756=ORIENTED_EDGE('',*,*,#14306,.F.);
#18757=ORIENTED_EDGE('',*,*,#14325,.T.);
#18758=ORIENTED_EDGE('',*,*,#14267,.F.);
#18759=ORIENTED_EDGE('',*,*,#14326,.F.);
#18760=ORIENTED_EDGE('',*,*,#14320,.F.);
#18761=ORIENTED_EDGE('',*,*,#14327,.F.);
#18762=ORIENTED_EDGE('',*,*,#14264,.F.);
#18763=ORIENTED_EDGE('',*,*,#14327,.T.);
#18764=ORIENTED_EDGE('',*,*,#14322,.F.);
#18765=ORIENTED_EDGE('',*,*,#14328,.T.);
#18766=ORIENTED_EDGE('',*,*,#14329,.F.);
#18767=ORIENTED_EDGE('',*,*,#14330,.F.);
#18768=ORIENTED_EDGE('',*,*,#14331,.F.);
#18769=ORIENTED_EDGE('',*,*,#14332,.T.);
#18770=ORIENTED_EDGE('',*,*,#14333,.F.);
#18771=ORIENTED_EDGE('',*,*,#14334,.F.);
#18772=ORIENTED_EDGE('',*,*,#14335,.F.);
#18773=ORIENTED_EDGE('',*,*,#14336,.T.);
#18774=ORIENTED_EDGE('',*,*,#14261,.F.);
#18775=ORIENTED_EDGE('',*,*,#14336,.F.);
#18776=ORIENTED_EDGE('',*,*,#14337,.F.);
#18777=ORIENTED_EDGE('',*,*,#14332,.F.);
#18778=ORIENTED_EDGE('',*,*,#14338,.F.);
#18779=ORIENTED_EDGE('',*,*,#14328,.F.);
#18780=ORIENTED_EDGE('',*,*,#14325,.F.);
#18781=ORIENTED_EDGE('',*,*,#14293,.F.);
#18782=ORIENTED_EDGE('',*,*,#14339,.F.);
#18783=ORIENTED_EDGE('',*,*,#14289,.F.);
#18784=ORIENTED_EDGE('',*,*,#14340,.F.);
#18785=ORIENTED_EDGE('',*,*,#14285,.F.);
#18786=ORIENTED_EDGE('',*,*,#14307,.F.);
#18787=ORIENTED_EDGE('',*,*,#14324,.F.);
#18788=ORIENTED_EDGE('',*,*,#14323,.F.);
#18789=ORIENTED_EDGE('',*,*,#14318,.F.);
#18790=ORIENTED_EDGE('',*,*,#14317,.F.);
#18791=ORIENTED_EDGE('',*,*,#14313,.F.);
#18792=ORIENTED_EDGE('',*,*,#14312,.F.);
#18793=ORIENTED_EDGE('',*,*,#14308,.F.);
#18794=ORIENTED_EDGE('',*,*,#14341,.F.);
#18795=ORIENTED_EDGE('',*,*,#14342,.F.);
#18796=ORIENTED_EDGE('',*,*,#14343,.F.);
#18797=ORIENTED_EDGE('',*,*,#14344,.F.);
#18798=ORIENTED_EDGE('',*,*,#14345,.F.);
#18799=ORIENTED_EDGE('',*,*,#14346,.F.);
#18800=ORIENTED_EDGE('',*,*,#14347,.F.);
#18801=ORIENTED_EDGE('',*,*,#14348,.F.);
#18802=ORIENTED_EDGE('',*,*,#14349,.T.);
#18803=ORIENTED_EDGE('',*,*,#14330,.T.);
#18804=ORIENTED_EDGE('',*,*,#14350,.T.);
#18805=ORIENTED_EDGE('',*,*,#14351,.T.);
#18806=ORIENTED_EDGE('',*,*,#14352,.T.);
#18807=ORIENTED_EDGE('',*,*,#14353,.T.);
#18808=ORIENTED_EDGE('',*,*,#14354,.T.);
#18809=ORIENTED_EDGE('',*,*,#14355,.T.);
#18810=ORIENTED_EDGE('',*,*,#14338,.T.);
#18811=ORIENTED_EDGE('',*,*,#14352,.F.);
#18812=ORIENTED_EDGE('',*,*,#14331,.T.);
#18813=ORIENTED_EDGE('',*,*,#14349,.F.);
#18814=ORIENTED_EDGE('',*,*,#14356,.T.);
#18815=ORIENTED_EDGE('',*,*,#14350,.F.);
#18816=ORIENTED_EDGE('',*,*,#14329,.T.);
#18817=ORIENTED_EDGE('',*,*,#14355,.F.);
#18818=ORIENTED_EDGE('',*,*,#14357,.T.);
#18819=ORIENTED_EDGE('',*,*,#14353,.F.);
#18820=ORIENTED_EDGE('',*,*,#14356,.F.);
#18821=ORIENTED_EDGE('',*,*,#14351,.F.);
#18822=ORIENTED_EDGE('',*,*,#14357,.F.);
#18823=ORIENTED_EDGE('',*,*,#14354,.F.);
#18824=ORIENTED_EDGE('',*,*,#14358,.T.);
#18825=ORIENTED_EDGE('',*,*,#14359,.F.);
#18826=ORIENTED_EDGE('',*,*,#14360,.F.);
#18827=ORIENTED_EDGE('',*,*,#14361,.F.);
#18828=ORIENTED_EDGE('',*,*,#14362,.F.);
#18829=ORIENTED_EDGE('',*,*,#14363,.F.);
#18830=ORIENTED_EDGE('',*,*,#14358,.F.);
#18831=ORIENTED_EDGE('',*,*,#14364,.T.);
#18832=ORIENTED_EDGE('',*,*,#14341,.T.);
#18833=ORIENTED_EDGE('',*,*,#14365,.T.);
#18834=ORIENTED_EDGE('',*,*,#14366,.T.);
#18835=ORIENTED_EDGE('',*,*,#14364,.F.);
#18836=ORIENTED_EDGE('',*,*,#14367,.T.);
#18837=ORIENTED_EDGE('',*,*,#14368,.T.);
#18838=ORIENTED_EDGE('',*,*,#14342,.T.);
#18839=ORIENTED_EDGE('',*,*,#14369,.T.);
#18840=ORIENTED_EDGE('',*,*,#14343,.T.);
#18841=ORIENTED_EDGE('',*,*,#14368,.F.);
#18842=ORIENTED_EDGE('',*,*,#14370,.T.);
#18843=ORIENTED_EDGE('',*,*,#14369,.F.);
#18844=ORIENTED_EDGE('',*,*,#14371,.T.);
#18845=ORIENTED_EDGE('',*,*,#14372,.T.);
#18846=ORIENTED_EDGE('',*,*,#14344,.T.);
#18847=ORIENTED_EDGE('',*,*,#14373,.T.);
#18848=ORIENTED_EDGE('',*,*,#14345,.T.);
#18849=ORIENTED_EDGE('',*,*,#14372,.F.);
#18850=ORIENTED_EDGE('',*,*,#13925,.T.);
#18851=ORIENTED_EDGE('',*,*,#14373,.F.);
#18852=ORIENTED_EDGE('',*,*,#14374,.T.);
#18853=ORIENTED_EDGE('',*,*,#14375,.T.);
#18854=ORIENTED_EDGE('',*,*,#14346,.T.);
#18855=ORIENTED_EDGE('',*,*,#14376,.T.);
#18856=ORIENTED_EDGE('',*,*,#14347,.T.);
#18857=ORIENTED_EDGE('',*,*,#14375,.F.);
#18858=ORIENTED_EDGE('',*,*,#14377,.T.);
#18859=ORIENTED_EDGE('',*,*,#14376,.F.);
#18860=ORIENTED_EDGE('',*,*,#14378,.T.);
#18861=ORIENTED_EDGE('',*,*,#14365,.F.);
#18862=ORIENTED_EDGE('',*,*,#14348,.T.);
#18863=ORIENTED_EDGE('',*,*,#14371,.F.);
#18864=ORIENTED_EDGE('',*,*,#14379,.T.);
#18865=ORIENTED_EDGE('',*,*,#14380,.F.);
#18866=ORIENTED_EDGE('',*,*,#13926,.T.);
#18867=ORIENTED_EDGE('',*,*,#14370,.F.);
#18868=ORIENTED_EDGE('',*,*,#14381,.F.);
#18869=ORIENTED_EDGE('',*,*,#14382,.F.);
#18870=ORIENTED_EDGE('',*,*,#14379,.F.);
#18871=ORIENTED_EDGE('',*,*,#14367,.F.);
#18872=ORIENTED_EDGE('',*,*,#14383,.T.);
#18873=ORIENTED_EDGE('',*,*,#14384,.F.);
#18874=ORIENTED_EDGE('',*,*,#14385,.F.);
#18875=ORIENTED_EDGE('',*,*,#14386,.F.);
#18876=ORIENTED_EDGE('',*,*,#14387,.F.);
#18877=ORIENTED_EDGE('',*,*,#14388,.F.);
#18878=ORIENTED_EDGE('',*,*,#14389,.T.);
#18879=ORIENTED_EDGE('',*,*,#14390,.F.);
#18880=ORIENTED_EDGE('',*,*,#14391,.F.);
#18881=ORIENTED_EDGE('',*,*,#14392,.F.);
#18882=ORIENTED_EDGE('',*,*,#14393,.F.);
#18883=ORIENTED_EDGE('',*,*,#14394,.F.);
#18884=ORIENTED_EDGE('',*,*,#14395,.F.);
#18885=ORIENTED_EDGE('',*,*,#14396,.T.);
#18886=ORIENTED_EDGE('',*,*,#14397,.F.);
#18887=ORIENTED_EDGE('',*,*,#14381,.T.);
#18888=ORIENTED_EDGE('',*,*,#14366,.F.);
#18889=ORIENTED_EDGE('',*,*,#14398,.F.);
#18890=ORIENTED_EDGE('',*,*,#14399,.F.);
#18891=ORIENTED_EDGE('',*,*,#14400,.F.);
#18892=ORIENTED_EDGE('',*,*,#14401,.F.);
#18893=ORIENTED_EDGE('',*,*,#14402,.F.);
#18894=ORIENTED_EDGE('',*,*,#14403,.F.);
#18895=ORIENTED_EDGE('',*,*,#14396,.F.);
#18896=ORIENTED_EDGE('',*,*,#14404,.F.);
#18897=ORIENTED_EDGE('',*,*,#14389,.F.);
#18898=ORIENTED_EDGE('',*,*,#14405,.F.);
#18899=ORIENTED_EDGE('',*,*,#14383,.F.);
#18900=ORIENTED_EDGE('',*,*,#14406,.T.);
#18901=ORIENTED_EDGE('',*,*,#14403,.T.);
#18902=ORIENTED_EDGE('',*,*,#14407,.T.);
#18903=ORIENTED_EDGE('',*,*,#14297,.T.);
#18904=ORIENTED_EDGE('',*,*,#14408,.T.);
#18905=ORIENTED_EDGE('',*,*,#14397,.T.);
#18906=ORIENTED_EDGE('',*,*,#14406,.F.);
#18907=ORIENTED_EDGE('',*,*,#14304,.T.);
#18908=ORIENTED_EDGE('',*,*,#14409,.T.);
#18909=ORIENTED_EDGE('',*,*,#14382,.T.);
#18910=ORIENTED_EDGE('',*,*,#14408,.F.);
#18911=ORIENTED_EDGE('',*,*,#14303,.T.);
#18912=ORIENTED_EDGE('',*,*,#14410,.T.);
#18913=ORIENTED_EDGE('',*,*,#14380,.T.);
#18914=ORIENTED_EDGE('',*,*,#14409,.F.);
#18915=ORIENTED_EDGE('',*,*,#14302,.T.);
#18916=ORIENTED_EDGE('',*,*,#14411,.T.);
#18917=ORIENTED_EDGE('',*,*,#13927,.T.);
#18918=ORIENTED_EDGE('',*,*,#14410,.F.);
#18919=ORIENTED_EDGE('',*,*,#14301,.T.);
#18920=ORIENTED_EDGE('',*,*,#14412,.T.);
#18921=ORIENTED_EDGE('',*,*,#14413,.T.);
#18922=ORIENTED_EDGE('',*,*,#14411,.F.);
#18923=ORIENTED_EDGE('',*,*,#14300,.T.);
#18924=ORIENTED_EDGE('',*,*,#14414,.T.);
#18925=ORIENTED_EDGE('',*,*,#14415,.T.);
#18926=ORIENTED_EDGE('',*,*,#14412,.F.);
#18927=ORIENTED_EDGE('',*,*,#14299,.T.);
#18928=ORIENTED_EDGE('',*,*,#14407,.F.);
#18929=ORIENTED_EDGE('',*,*,#14416,.T.);
#18930=ORIENTED_EDGE('',*,*,#14414,.F.);
#18931=ORIENTED_EDGE('',*,*,#14298,.T.);
#18932=ORIENTED_EDGE('',*,*,#14374,.F.);
#18933=ORIENTED_EDGE('',*,*,#13928,.T.);
#18934=ORIENTED_EDGE('',*,*,#14413,.F.);
#18935=ORIENTED_EDGE('',*,*,#14417,.T.);
#18936=ORIENTED_EDGE('',*,*,#14377,.F.);
#18937=ORIENTED_EDGE('',*,*,#14417,.F.);
#18938=ORIENTED_EDGE('',*,*,#14415,.F.);
#18939=ORIENTED_EDGE('',*,*,#14418,.F.);
#18940=ORIENTED_EDGE('',*,*,#14378,.F.);
#18941=ORIENTED_EDGE('',*,*,#14418,.T.);
#18942=ORIENTED_EDGE('',*,*,#14416,.F.);
#18943=ORIENTED_EDGE('',*,*,#14402,.T.);
#18944=ORIENTED_EDGE('',*,*,#14419,.F.);
#18945=ORIENTED_EDGE('',*,*,#14420,.F.);
#18946=ORIENTED_EDGE('',*,*,#14421,.F.);
#18947=ORIENTED_EDGE('',*,*,#14422,.F.);
#18948=ORIENTED_EDGE('',*,*,#14423,.F.);
#18949=ORIENTED_EDGE('',*,*,#14400,.T.);
#18950=ORIENTED_EDGE('',*,*,#14424,.F.);
#18951=ORIENTED_EDGE('',*,*,#14425,.F.);
#18952=ORIENTED_EDGE('',*,*,#14426,.F.);
#18953=ORIENTED_EDGE('',*,*,#14427,.F.);
#18954=ORIENTED_EDGE('',*,*,#14428,.F.);
#18955=ORIENTED_EDGE('',*,*,#14429,.F.);
#18956=ORIENTED_EDGE('',*,*,#14398,.T.);
#18957=ORIENTED_EDGE('',*,*,#14430,.T.);
#18958=ORIENTED_EDGE('',*,*,#14361,.T.);
#18959=ORIENTED_EDGE('',*,*,#14431,.F.);
#18960=ORIENTED_EDGE('',*,*,#14427,.T.);
#18961=ORIENTED_EDGE('',*,*,#14426,.T.);
#18962=ORIENTED_EDGE('',*,*,#14425,.T.);
#18963=ORIENTED_EDGE('',*,*,#14432,.T.);
#18964=ORIENTED_EDGE('',*,*,#14359,.T.);
#18965=ORIENTED_EDGE('',*,*,#14363,.T.);
#18966=ORIENTED_EDGE('',*,*,#14433,.T.);
#18967=ORIENTED_EDGE('',*,*,#14399,.T.);
#18968=ORIENTED_EDGE('',*,*,#14432,.F.);
#18969=ORIENTED_EDGE('',*,*,#14429,.T.);
#18970=ORIENTED_EDGE('',*,*,#14428,.T.);
#18971=ORIENTED_EDGE('',*,*,#14431,.T.);
#18972=ORIENTED_EDGE('',*,*,#14360,.T.);
#18973=ORIENTED_EDGE('',*,*,#14430,.F.);
#18974=ORIENTED_EDGE('',*,*,#14424,.T.);
#18975=ORIENTED_EDGE('',*,*,#14433,.F.);
#18976=ORIENTED_EDGE('',*,*,#14362,.T.);
#18977=ORIENTED_EDGE('',*,*,#14434,.T.);
#18978=ORIENTED_EDGE('',*,*,#14435,.T.);
#18979=ORIENTED_EDGE('',*,*,#14436,.T.);
#18980=ORIENTED_EDGE('',*,*,#14437,.T.);
#18981=ORIENTED_EDGE('',*,*,#14340,.T.);
#18982=ORIENTED_EDGE('',*,*,#14438,.T.);
#18983=ORIENTED_EDGE('',*,*,#14287,.T.);
#18984=ORIENTED_EDGE('',*,*,#14439,.T.);
#18985=ORIENTED_EDGE('',*,*,#14440,.T.);
#18986=ORIENTED_EDGE('',*,*,#14439,.F.);
#18987=ORIENTED_EDGE('',*,*,#14286,.T.);
#18988=ORIENTED_EDGE('',*,*,#14437,.F.);
#18989=ORIENTED_EDGE('',*,*,#14441,.T.);
#18990=ORIENTED_EDGE('',*,*,#14434,.F.);
#18991=ORIENTED_EDGE('',*,*,#14288,.T.);
#18992=ORIENTED_EDGE('',*,*,#14438,.F.);
#18993=ORIENTED_EDGE('',*,*,#14442,.T.);
#18994=ORIENTED_EDGE('',*,*,#14440,.F.);
#18995=ORIENTED_EDGE('',*,*,#14441,.F.);
#18996=ORIENTED_EDGE('',*,*,#14436,.F.);
#18997=ORIENTED_EDGE('',*,*,#14443,.T.);
#18998=ORIENTED_EDGE('',*,*,#14444,.F.);
#18999=ORIENTED_EDGE('',*,*,#14445,.F.);
#19000=ORIENTED_EDGE('',*,*,#14446,.F.);
#19001=ORIENTED_EDGE('',*,*,#14447,.F.);
#19002=ORIENTED_EDGE('',*,*,#14448,.F.);
#19003=ORIENTED_EDGE('',*,*,#14443,.F.);
#19004=ORIENTED_EDGE('',*,*,#14435,.F.);
#19005=ORIENTED_EDGE('',*,*,#14442,.F.);
#19006=ORIENTED_EDGE('',*,*,#14449,.T.);
#19007=ORIENTED_EDGE('',*,*,#14446,.T.);
#19008=ORIENTED_EDGE('',*,*,#14450,.F.);
#19009=ORIENTED_EDGE('',*,*,#14393,.T.);
#19010=ORIENTED_EDGE('',*,*,#14392,.T.);
#19011=ORIENTED_EDGE('',*,*,#14391,.T.);
#19012=ORIENTED_EDGE('',*,*,#14451,.T.);
#19013=ORIENTED_EDGE('',*,*,#14444,.T.);
#19014=ORIENTED_EDGE('',*,*,#14448,.T.);
#19015=ORIENTED_EDGE('',*,*,#14452,.T.);
#19016=ORIENTED_EDGE('',*,*,#14404,.T.);
#19017=ORIENTED_EDGE('',*,*,#14451,.F.);
#19018=ORIENTED_EDGE('',*,*,#14395,.T.);
#19019=ORIENTED_EDGE('',*,*,#14394,.T.);
#19020=ORIENTED_EDGE('',*,*,#14450,.T.);
#19021=ORIENTED_EDGE('',*,*,#14445,.T.);
#19022=ORIENTED_EDGE('',*,*,#14449,.F.);
#19023=ORIENTED_EDGE('',*,*,#14390,.T.);
#19024=ORIENTED_EDGE('',*,*,#14452,.F.);
#19025=ORIENTED_EDGE('',*,*,#14447,.T.);
#19026=ORIENTED_EDGE('',*,*,#14453,.T.);
#19027=ORIENTED_EDGE('',*,*,#14334,.T.);
#19028=ORIENTED_EDGE('',*,*,#14454,.T.);
#19029=ORIENTED_EDGE('',*,*,#14455,.T.);
#19030=ORIENTED_EDGE('',*,*,#14456,.T.);
#19031=ORIENTED_EDGE('',*,*,#14457,.T.);
#19032=ORIENTED_EDGE('',*,*,#14458,.T.);
#19033=ORIENTED_EDGE('',*,*,#14459,.T.);
#19034=ORIENTED_EDGE('',*,*,#14337,.T.);
#19035=ORIENTED_EDGE('',*,*,#14456,.F.);
#19036=ORIENTED_EDGE('',*,*,#14335,.T.);
#19037=ORIENTED_EDGE('',*,*,#14453,.F.);
#19038=ORIENTED_EDGE('',*,*,#14460,.T.);
#19039=ORIENTED_EDGE('',*,*,#14454,.F.);
#19040=ORIENTED_EDGE('',*,*,#14333,.T.);
#19041=ORIENTED_EDGE('',*,*,#14459,.F.);
#19042=ORIENTED_EDGE('',*,*,#14461,.T.);
#19043=ORIENTED_EDGE('',*,*,#14457,.F.);
#19044=ORIENTED_EDGE('',*,*,#14460,.F.);
#19045=ORIENTED_EDGE('',*,*,#14455,.F.);
#19046=ORIENTED_EDGE('',*,*,#14461,.F.);
#19047=ORIENTED_EDGE('',*,*,#14458,.F.);
#19048=ORIENTED_EDGE('',*,*,#14462,.T.);
#19049=ORIENTED_EDGE('',*,*,#14463,.F.);
#19050=ORIENTED_EDGE('',*,*,#14464,.F.);
#19051=ORIENTED_EDGE('',*,*,#14465,.F.);
#19052=ORIENTED_EDGE('',*,*,#14466,.F.);
#19053=ORIENTED_EDGE('',*,*,#14467,.F.);
#19054=ORIENTED_EDGE('',*,*,#14462,.F.);
#19055=ORIENTED_EDGE('',*,*,#14468,.T.);
#19056=ORIENTED_EDGE('',*,*,#14465,.T.);
#19057=ORIENTED_EDGE('',*,*,#14469,.F.);
#19058=ORIENTED_EDGE('',*,*,#14422,.T.);
#19059=ORIENTED_EDGE('',*,*,#14421,.T.);
#19060=ORIENTED_EDGE('',*,*,#14420,.T.);
#19061=ORIENTED_EDGE('',*,*,#14470,.T.);
#19062=ORIENTED_EDGE('',*,*,#14463,.T.);
#19063=ORIENTED_EDGE('',*,*,#14467,.T.);
#19064=ORIENTED_EDGE('',*,*,#14471,.T.);
#19065=ORIENTED_EDGE('',*,*,#14401,.T.);
#19066=ORIENTED_EDGE('',*,*,#14470,.F.);
#19067=ORIENTED_EDGE('',*,*,#14423,.T.);
#19068=ORIENTED_EDGE('',*,*,#14469,.T.);
#19069=ORIENTED_EDGE('',*,*,#14464,.T.);
#19070=ORIENTED_EDGE('',*,*,#14468,.F.);
#19071=ORIENTED_EDGE('',*,*,#14419,.T.);
#19072=ORIENTED_EDGE('',*,*,#14471,.F.);
#19073=ORIENTED_EDGE('',*,*,#14466,.T.);
#19074=ORIENTED_EDGE('',*,*,#14472,.T.);
#19075=ORIENTED_EDGE('',*,*,#14473,.T.);
#19076=ORIENTED_EDGE('',*,*,#14474,.T.);
#19077=ORIENTED_EDGE('',*,*,#14475,.T.);
#19078=ORIENTED_EDGE('',*,*,#14339,.T.);
#19079=ORIENTED_EDGE('',*,*,#14476,.T.);
#19080=ORIENTED_EDGE('',*,*,#14291,.T.);
#19081=ORIENTED_EDGE('',*,*,#14477,.T.);
#19082=ORIENTED_EDGE('',*,*,#14478,.T.);
#19083=ORIENTED_EDGE('',*,*,#14477,.F.);
#19084=ORIENTED_EDGE('',*,*,#14290,.T.);
#19085=ORIENTED_EDGE('',*,*,#14475,.F.);
#19086=ORIENTED_EDGE('',*,*,#14479,.T.);
#19087=ORIENTED_EDGE('',*,*,#14472,.F.);
#19088=ORIENTED_EDGE('',*,*,#14292,.T.);
#19089=ORIENTED_EDGE('',*,*,#14476,.F.);
#19090=ORIENTED_EDGE('',*,*,#14480,.T.);
#19091=ORIENTED_EDGE('',*,*,#14478,.F.);
#19092=ORIENTED_EDGE('',*,*,#14479,.F.);
#19093=ORIENTED_EDGE('',*,*,#14474,.F.);
#19094=ORIENTED_EDGE('',*,*,#14481,.T.);
#19095=ORIENTED_EDGE('',*,*,#14482,.F.);
#19096=ORIENTED_EDGE('',*,*,#14483,.F.);
#19097=ORIENTED_EDGE('',*,*,#14484,.F.);
#19098=ORIENTED_EDGE('',*,*,#14485,.F.);
#19099=ORIENTED_EDGE('',*,*,#14486,.F.);
#19100=ORIENTED_EDGE('',*,*,#14481,.F.);
#19101=ORIENTED_EDGE('',*,*,#14473,.F.);
#19102=ORIENTED_EDGE('',*,*,#14480,.F.);
#19103=ORIENTED_EDGE('',*,*,#14487,.T.);
#19104=ORIENTED_EDGE('',*,*,#14484,.T.);
#19105=ORIENTED_EDGE('',*,*,#14488,.F.);
#19106=ORIENTED_EDGE('',*,*,#14387,.T.);
#19107=ORIENTED_EDGE('',*,*,#14386,.T.);
#19108=ORIENTED_EDGE('',*,*,#14385,.T.);
#19109=ORIENTED_EDGE('',*,*,#14489,.T.);
#19110=ORIENTED_EDGE('',*,*,#14482,.T.);
#19111=ORIENTED_EDGE('',*,*,#14486,.T.);
#19112=ORIENTED_EDGE('',*,*,#14490,.T.);
#19113=ORIENTED_EDGE('',*,*,#14405,.T.);
#19114=ORIENTED_EDGE('',*,*,#14489,.F.);
#19115=ORIENTED_EDGE('',*,*,#14388,.T.);
#19116=ORIENTED_EDGE('',*,*,#14488,.T.);
#19117=ORIENTED_EDGE('',*,*,#14483,.T.);
#19118=ORIENTED_EDGE('',*,*,#14487,.F.);
#19119=ORIENTED_EDGE('',*,*,#14384,.T.);
#19120=ORIENTED_EDGE('',*,*,#14490,.F.);
#19121=ORIENTED_EDGE('',*,*,#14485,.T.);
#19122=ORIENTED_EDGE('',*,*,#14491,.T.);
#19123=ORIENTED_EDGE('',*,*,#14492,.T.);
#19124=ORIENTED_EDGE('',*,*,#14493,.T.);
#19125=ORIENTED_EDGE('',*,*,#14492,.F.);
#19126=ORIENTED_EDGE('',*,*,#14493,.F.);
#19127=ORIENTED_EDGE('',*,*,#14494,.T.);
#19128=ORIENTED_EDGE('',*,*,#14495,.F.);
#19129=ORIENTED_EDGE('',*,*,#14494,.F.);
#19130=ORIENTED_EDGE('',*,*,#13862,.F.);
#19131=ORIENTED_EDGE('',*,*,#13878,.F.);
#19132=ORIENTED_EDGE('',*,*,#13880,.F.);
#19133=ORIENTED_EDGE('',*,*,#13851,.F.);
#19134=ORIENTED_EDGE('',*,*,#14496,.F.);
#19135=ORIENTED_EDGE('',*,*,#14491,.F.);
#19136=ORIENTED_EDGE('',*,*,#14497,.T.);
#19137=ORIENTED_EDGE('',*,*,#14498,.T.);
#19138=ORIENTED_EDGE('',*,*,#14495,.T.);
#19139=ORIENTED_EDGE('',*,*,#14498,.F.);
#19140=ORIENTED_EDGE('',*,*,#14009,.F.);
#19141=ORIENTED_EDGE('',*,*,#13865,.T.);
#19142=ORIENTED_EDGE('',*,*,#14280,.F.);
#19143=ORIENTED_EDGE('',*,*,#14499,.T.);
#19144=ORIENTED_EDGE('',*,*,#14500,.F.);
#19145=ORIENTED_EDGE('',*,*,#14497,.F.);
#19146=ORIENTED_EDGE('',*,*,#14496,.T.);
#19147=ORIENTED_EDGE('',*,*,#14501,.T.);
#19148=ORIENTED_EDGE('',*,*,#14502,.T.);
#19149=ORIENTED_EDGE('',*,*,#14501,.F.);
#19150=ORIENTED_EDGE('',*,*,#14502,.F.);
#19151=ORIENTED_EDGE('',*,*,#14503,.T.);
#19152=ORIENTED_EDGE('',*,*,#14504,.F.);
#19153=ORIENTED_EDGE('',*,*,#14503,.F.);
#19154=ORIENTED_EDGE('',*,*,#14500,.T.);
#19155=ORIENTED_EDGE('',*,*,#14505,.T.);
#19156=ORIENTED_EDGE('',*,*,#14504,.T.);
#19157=ORIENTED_EDGE('',*,*,#14505,.F.);
#19158=ORIENTED_EDGE('',*,*,#14506,.F.);
#19159=ORIENTED_EDGE('',*,*,#14507,.T.);
#19160=ORIENTED_EDGE('',*,*,#14508,.T.);
#19161=ORIENTED_EDGE('',*,*,#14509,.F.);
#19162=ORIENTED_EDGE('',*,*,#14510,.F.);
#19163=ORIENTED_EDGE('',*,*,#14511,.T.);
#19164=ORIENTED_EDGE('',*,*,#14512,.T.);
#19165=ORIENTED_EDGE('',*,*,#14507,.F.);
#19166=ORIENTED_EDGE('',*,*,#14513,.F.);
#19167=ORIENTED_EDGE('',*,*,#14514,.T.);
#19168=ORIENTED_EDGE('',*,*,#14515,.T.);
#19169=ORIENTED_EDGE('',*,*,#14511,.F.);
#19170=ORIENTED_EDGE('',*,*,#14516,.F.);
#19171=ORIENTED_EDGE('',*,*,#14517,.T.);
#19172=ORIENTED_EDGE('',*,*,#14518,.T.);
#19173=ORIENTED_EDGE('',*,*,#14514,.F.);
#19174=ORIENTED_EDGE('',*,*,#14519,.F.);
#19175=ORIENTED_EDGE('',*,*,#14520,.T.);
#19176=ORIENTED_EDGE('',*,*,#14521,.T.);
#19177=ORIENTED_EDGE('',*,*,#14517,.F.);
#19178=ORIENTED_EDGE('',*,*,#14522,.F.);
#19179=ORIENTED_EDGE('',*,*,#14523,.T.);
#19180=ORIENTED_EDGE('',*,*,#14524,.T.);
#19181=ORIENTED_EDGE('',*,*,#14520,.F.);
#19182=ORIENTED_EDGE('',*,*,#14525,.F.);
#19183=ORIENTED_EDGE('',*,*,#14526,.T.);
#19184=ORIENTED_EDGE('',*,*,#14527,.T.);
#19185=ORIENTED_EDGE('',*,*,#14523,.F.);
#19186=ORIENTED_EDGE('',*,*,#14528,.F.);
#19187=ORIENTED_EDGE('',*,*,#14509,.T.);
#19188=ORIENTED_EDGE('',*,*,#14529,.T.);
#19189=ORIENTED_EDGE('',*,*,#14526,.F.);
#19190=ORIENTED_EDGE('',*,*,#14056,.F.);
#19191=ORIENTED_EDGE('',*,*,#14530,.T.);
#19192=ORIENTED_EDGE('',*,*,#14531,.T.);
#19193=ORIENTED_EDGE('',*,*,#14532,.F.);
#19194=ORIENTED_EDGE('',*,*,#14065,.F.);
#19195=ORIENTED_EDGE('',*,*,#14533,.T.);
#19196=ORIENTED_EDGE('',*,*,#14534,.T.);
#19197=ORIENTED_EDGE('',*,*,#14530,.F.);
#19198=ORIENTED_EDGE('',*,*,#14064,.F.);
#19199=ORIENTED_EDGE('',*,*,#14535,.T.);
#19200=ORIENTED_EDGE('',*,*,#14536,.T.);
#19201=ORIENTED_EDGE('',*,*,#14533,.F.);
#19202=ORIENTED_EDGE('',*,*,#14063,.F.);
#19203=ORIENTED_EDGE('',*,*,#14537,.T.);
#19204=ORIENTED_EDGE('',*,*,#14538,.T.);
#19205=ORIENTED_EDGE('',*,*,#14535,.F.);
#19206=ORIENTED_EDGE('',*,*,#14062,.F.);
#19207=ORIENTED_EDGE('',*,*,#14539,.T.);
#19208=ORIENTED_EDGE('',*,*,#14540,.T.);
#19209=ORIENTED_EDGE('',*,*,#14537,.F.);
#19210=ORIENTED_EDGE('',*,*,#14061,.F.);
#19211=ORIENTED_EDGE('',*,*,#14541,.T.);
#19212=ORIENTED_EDGE('',*,*,#14542,.T.);
#19213=ORIENTED_EDGE('',*,*,#14539,.F.);
#19214=ORIENTED_EDGE('',*,*,#14060,.F.);
#19215=ORIENTED_EDGE('',*,*,#14543,.T.);
#19216=ORIENTED_EDGE('',*,*,#14544,.T.);
#19217=ORIENTED_EDGE('',*,*,#14541,.F.);
#19218=ORIENTED_EDGE('',*,*,#14059,.F.);
#19219=ORIENTED_EDGE('',*,*,#14545,.T.);
#19220=ORIENTED_EDGE('',*,*,#14546,.T.);
#19221=ORIENTED_EDGE('',*,*,#14543,.F.);
#19222=ORIENTED_EDGE('',*,*,#14058,.F.);
#19223=ORIENTED_EDGE('',*,*,#14547,.T.);
#19224=ORIENTED_EDGE('',*,*,#14548,.T.);
#19225=ORIENTED_EDGE('',*,*,#14545,.F.);
#19226=ORIENTED_EDGE('',*,*,#14057,.F.);
#19227=ORIENTED_EDGE('',*,*,#14532,.T.);
#19228=ORIENTED_EDGE('',*,*,#14549,.T.);
#19229=ORIENTED_EDGE('',*,*,#14547,.F.);
#19230=ORIENTED_EDGE('',*,*,#14549,.F.);
#19231=ORIENTED_EDGE('',*,*,#14531,.F.);
#19232=ORIENTED_EDGE('',*,*,#14534,.F.);
#19233=ORIENTED_EDGE('',*,*,#14536,.F.);
#19234=ORIENTED_EDGE('',*,*,#14538,.F.);
#19235=ORIENTED_EDGE('',*,*,#14540,.F.);
#19236=ORIENTED_EDGE('',*,*,#14542,.F.);
#19237=ORIENTED_EDGE('',*,*,#14544,.F.);
#19238=ORIENTED_EDGE('',*,*,#14546,.F.);
#19239=ORIENTED_EDGE('',*,*,#14548,.F.);
#19240=ORIENTED_EDGE('',*,*,#14529,.F.);
#19241=ORIENTED_EDGE('',*,*,#14508,.F.);
#19242=ORIENTED_EDGE('',*,*,#14512,.F.);
#19243=ORIENTED_EDGE('',*,*,#14515,.F.);
#19244=ORIENTED_EDGE('',*,*,#14518,.F.);
#19245=ORIENTED_EDGE('',*,*,#14521,.F.);
#19246=ORIENTED_EDGE('',*,*,#14524,.F.);
#19247=ORIENTED_EDGE('',*,*,#14527,.F.);
#19248=ORIENTED_EDGE('',*,*,#14066,.F.);
#19249=ORIENTED_EDGE('',*,*,#14550,.T.);
#19250=ORIENTED_EDGE('',*,*,#14551,.T.);
#19251=ORIENTED_EDGE('',*,*,#14552,.F.);
#19252=ORIENTED_EDGE('',*,*,#14073,.F.);
#19253=ORIENTED_EDGE('',*,*,#14553,.T.);
#19254=ORIENTED_EDGE('',*,*,#14554,.T.);
#19255=ORIENTED_EDGE('',*,*,#14550,.F.);
#19256=ORIENTED_EDGE('',*,*,#14072,.F.);
#19257=ORIENTED_EDGE('',*,*,#14555,.T.);
#19258=ORIENTED_EDGE('',*,*,#14556,.T.);
#19259=ORIENTED_EDGE('',*,*,#14553,.F.);
#19260=ORIENTED_EDGE('',*,*,#14071,.F.);
#19261=ORIENTED_EDGE('',*,*,#14557,.T.);
#19262=ORIENTED_EDGE('',*,*,#14558,.T.);
#19263=ORIENTED_EDGE('',*,*,#14555,.F.);
#19264=ORIENTED_EDGE('',*,*,#14070,.F.);
#19265=ORIENTED_EDGE('',*,*,#14559,.T.);
#19266=ORIENTED_EDGE('',*,*,#14560,.T.);
#19267=ORIENTED_EDGE('',*,*,#14557,.F.);
#19268=ORIENTED_EDGE('',*,*,#14069,.F.);
#19269=ORIENTED_EDGE('',*,*,#14561,.T.);
#19270=ORIENTED_EDGE('',*,*,#14562,.T.);
#19271=ORIENTED_EDGE('',*,*,#14559,.F.);
#19272=ORIENTED_EDGE('',*,*,#14068,.F.);
#19273=ORIENTED_EDGE('',*,*,#14563,.T.);
#19274=ORIENTED_EDGE('',*,*,#14564,.T.);
#19275=ORIENTED_EDGE('',*,*,#14561,.F.);
#19276=ORIENTED_EDGE('',*,*,#14067,.F.);
#19277=ORIENTED_EDGE('',*,*,#14552,.T.);
#19278=ORIENTED_EDGE('',*,*,#14565,.T.);
#19279=ORIENTED_EDGE('',*,*,#14563,.F.);
#19280=ORIENTED_EDGE('',*,*,#14565,.F.);
#19281=ORIENTED_EDGE('',*,*,#14551,.F.);
#19282=ORIENTED_EDGE('',*,*,#14554,.F.);
#19283=ORIENTED_EDGE('',*,*,#14556,.F.);
#19284=ORIENTED_EDGE('',*,*,#14558,.F.);
#19285=ORIENTED_EDGE('',*,*,#14560,.F.);
#19286=ORIENTED_EDGE('',*,*,#14562,.F.);
#19287=ORIENTED_EDGE('',*,*,#14564,.F.);
#19288=ORIENTED_EDGE('',*,*,#14566,.F.);
#19289=ORIENTED_EDGE('',*,*,#14567,.T.);
#19290=ORIENTED_EDGE('',*,*,#14568,.T.);
#19291=ORIENTED_EDGE('',*,*,#14569,.F.);
#19292=ORIENTED_EDGE('',*,*,#14570,.F.);
#19293=ORIENTED_EDGE('',*,*,#14571,.T.);
#19294=ORIENTED_EDGE('',*,*,#14572,.T.);
#19295=ORIENTED_EDGE('',*,*,#14567,.F.);
#19296=ORIENTED_EDGE('',*,*,#14573,.F.);
#19297=ORIENTED_EDGE('',*,*,#14574,.T.);
#19298=ORIENTED_EDGE('',*,*,#14575,.T.);
#19299=ORIENTED_EDGE('',*,*,#14571,.F.);
#19300=ORIENTED_EDGE('',*,*,#14576,.F.);
#19301=ORIENTED_EDGE('',*,*,#14577,.T.);
#19302=ORIENTED_EDGE('',*,*,#14578,.T.);
#19303=ORIENTED_EDGE('',*,*,#14574,.F.);
#19304=ORIENTED_EDGE('',*,*,#14579,.F.);
#19305=ORIENTED_EDGE('',*,*,#14580,.T.);
#19306=ORIENTED_EDGE('',*,*,#14581,.T.);
#19307=ORIENTED_EDGE('',*,*,#14577,.F.);
#19308=ORIENTED_EDGE('',*,*,#14582,.F.);
#19309=ORIENTED_EDGE('',*,*,#14583,.T.);
#19310=ORIENTED_EDGE('',*,*,#14584,.T.);
#19311=ORIENTED_EDGE('',*,*,#14580,.F.);
#19312=ORIENTED_EDGE('',*,*,#14585,.F.);
#19313=ORIENTED_EDGE('',*,*,#14586,.T.);
#19314=ORIENTED_EDGE('',*,*,#14587,.T.);
#19315=ORIENTED_EDGE('',*,*,#14583,.F.);
#19316=ORIENTED_EDGE('',*,*,#14588,.F.);
#19317=ORIENTED_EDGE('',*,*,#14589,.T.);
#19318=ORIENTED_EDGE('',*,*,#14590,.T.);
#19319=ORIENTED_EDGE('',*,*,#14586,.F.);
#19320=ORIENTED_EDGE('',*,*,#14591,.F.);
#19321=ORIENTED_EDGE('',*,*,#14569,.T.);
#19322=ORIENTED_EDGE('',*,*,#14592,.T.);
#19323=ORIENTED_EDGE('',*,*,#14589,.F.);
#19324=ORIENTED_EDGE('',*,*,#14074,.F.);
#19325=ORIENTED_EDGE('',*,*,#14593,.T.);
#19326=ORIENTED_EDGE('',*,*,#14594,.T.);
#19327=ORIENTED_EDGE('',*,*,#14595,.F.);
#19328=ORIENTED_EDGE('',*,*,#14086,.F.);
#19329=ORIENTED_EDGE('',*,*,#14596,.T.);
#19330=ORIENTED_EDGE('',*,*,#14597,.T.);
#19331=ORIENTED_EDGE('',*,*,#14593,.F.);
#19332=ORIENTED_EDGE('',*,*,#14085,.F.);
#19333=ORIENTED_EDGE('',*,*,#14598,.T.);
#19334=ORIENTED_EDGE('',*,*,#14599,.T.);
#19335=ORIENTED_EDGE('',*,*,#14596,.F.);
#19336=ORIENTED_EDGE('',*,*,#14084,.F.);
#19337=ORIENTED_EDGE('',*,*,#14600,.T.);
#19338=ORIENTED_EDGE('',*,*,#14601,.T.);
#19339=ORIENTED_EDGE('',*,*,#14598,.F.);
#19340=ORIENTED_EDGE('',*,*,#14083,.F.);
#19341=ORIENTED_EDGE('',*,*,#14602,.T.);
#19342=ORIENTED_EDGE('',*,*,#14603,.T.);
#19343=ORIENTED_EDGE('',*,*,#14600,.F.);
#19344=ORIENTED_EDGE('',*,*,#14082,.F.);
#19345=ORIENTED_EDGE('',*,*,#14604,.T.);
#19346=ORIENTED_EDGE('',*,*,#14605,.T.);
#19347=ORIENTED_EDGE('',*,*,#14602,.F.);
#19348=ORIENTED_EDGE('',*,*,#14081,.F.);
#19349=ORIENTED_EDGE('',*,*,#14606,.T.);
#19350=ORIENTED_EDGE('',*,*,#14607,.T.);
#19351=ORIENTED_EDGE('',*,*,#14604,.F.);
#19352=ORIENTED_EDGE('',*,*,#14080,.F.);
#19353=ORIENTED_EDGE('',*,*,#14608,.T.);
#19354=ORIENTED_EDGE('',*,*,#14609,.T.);
#19355=ORIENTED_EDGE('',*,*,#14606,.F.);
#19356=ORIENTED_EDGE('',*,*,#14079,.F.);
#19357=ORIENTED_EDGE('',*,*,#14610,.T.);
#19358=ORIENTED_EDGE('',*,*,#14611,.T.);
#19359=ORIENTED_EDGE('',*,*,#14608,.F.);
#19360=ORIENTED_EDGE('',*,*,#14078,.F.);
#19361=ORIENTED_EDGE('',*,*,#14612,.T.);
#19362=ORIENTED_EDGE('',*,*,#14613,.T.);
#19363=ORIENTED_EDGE('',*,*,#14610,.F.);
#19364=ORIENTED_EDGE('',*,*,#14077,.F.);
#19365=ORIENTED_EDGE('',*,*,#14614,.T.);
#19366=ORIENTED_EDGE('',*,*,#14615,.T.);
#19367=ORIENTED_EDGE('',*,*,#14612,.F.);
#19368=ORIENTED_EDGE('',*,*,#14076,.F.);
#19369=ORIENTED_EDGE('',*,*,#14616,.T.);
#19370=ORIENTED_EDGE('',*,*,#14617,.T.);
#19371=ORIENTED_EDGE('',*,*,#14614,.F.);
#19372=ORIENTED_EDGE('',*,*,#14075,.F.);
#19373=ORIENTED_EDGE('',*,*,#14595,.T.);
#19374=ORIENTED_EDGE('',*,*,#14618,.T.);
#19375=ORIENTED_EDGE('',*,*,#14616,.F.);
#19376=ORIENTED_EDGE('',*,*,#14618,.F.);
#19377=ORIENTED_EDGE('',*,*,#14594,.F.);
#19378=ORIENTED_EDGE('',*,*,#14597,.F.);
#19379=ORIENTED_EDGE('',*,*,#14599,.F.);
#19380=ORIENTED_EDGE('',*,*,#14601,.F.);
#19381=ORIENTED_EDGE('',*,*,#14603,.F.);
#19382=ORIENTED_EDGE('',*,*,#14605,.F.);
#19383=ORIENTED_EDGE('',*,*,#14607,.F.);
#19384=ORIENTED_EDGE('',*,*,#14609,.F.);
#19385=ORIENTED_EDGE('',*,*,#14611,.F.);
#19386=ORIENTED_EDGE('',*,*,#14613,.F.);
#19387=ORIENTED_EDGE('',*,*,#14615,.F.);
#19388=ORIENTED_EDGE('',*,*,#14617,.F.);
#19389=ORIENTED_EDGE('',*,*,#14592,.F.);
#19390=ORIENTED_EDGE('',*,*,#14568,.F.);
#19391=ORIENTED_EDGE('',*,*,#14572,.F.);
#19392=ORIENTED_EDGE('',*,*,#14575,.F.);
#19393=ORIENTED_EDGE('',*,*,#14578,.F.);
#19394=ORIENTED_EDGE('',*,*,#14581,.F.);
#19395=ORIENTED_EDGE('',*,*,#14584,.F.);
#19396=ORIENTED_EDGE('',*,*,#14587,.F.);
#19397=ORIENTED_EDGE('',*,*,#14590,.F.);
#19398=ORIENTED_EDGE('',*,*,#14087,.F.);
#19399=ORIENTED_EDGE('',*,*,#14619,.T.);
#19400=ORIENTED_EDGE('',*,*,#14620,.T.);
#19401=ORIENTED_EDGE('',*,*,#14621,.F.);
#19402=ORIENTED_EDGE('',*,*,#14108,.F.);
#19403=ORIENTED_EDGE('',*,*,#14622,.T.);
#19404=ORIENTED_EDGE('',*,*,#14623,.T.);
#19405=ORIENTED_EDGE('',*,*,#14619,.F.);
#19406=ORIENTED_EDGE('',*,*,#14107,.F.);
#19407=ORIENTED_EDGE('',*,*,#14624,.T.);
#19408=ORIENTED_EDGE('',*,*,#14625,.T.);
#19409=ORIENTED_EDGE('',*,*,#14622,.F.);
#19410=ORIENTED_EDGE('',*,*,#14106,.F.);
#19411=ORIENTED_EDGE('',*,*,#14626,.T.);
#19412=ORIENTED_EDGE('',*,*,#14627,.T.);
#19413=ORIENTED_EDGE('',*,*,#14624,.F.);
#19414=ORIENTED_EDGE('',*,*,#14105,.F.);
#19415=ORIENTED_EDGE('',*,*,#14628,.T.);
#19416=ORIENTED_EDGE('',*,*,#14629,.T.);
#19417=ORIENTED_EDGE('',*,*,#14626,.F.);
#19418=ORIENTED_EDGE('',*,*,#14104,.F.);
#19419=ORIENTED_EDGE('',*,*,#14630,.T.);
#19420=ORIENTED_EDGE('',*,*,#14631,.T.);
#19421=ORIENTED_EDGE('',*,*,#14628,.F.);
#19422=ORIENTED_EDGE('',*,*,#14103,.F.);
#19423=ORIENTED_EDGE('',*,*,#14632,.T.);
#19424=ORIENTED_EDGE('',*,*,#14633,.T.);
#19425=ORIENTED_EDGE('',*,*,#14630,.F.);
#19426=ORIENTED_EDGE('',*,*,#14102,.F.);
#19427=ORIENTED_EDGE('',*,*,#14634,.T.);
#19428=ORIENTED_EDGE('',*,*,#14635,.T.);
#19429=ORIENTED_EDGE('',*,*,#14632,.F.);
#19430=ORIENTED_EDGE('',*,*,#14101,.F.);
#19431=ORIENTED_EDGE('',*,*,#14636,.T.);
#19432=ORIENTED_EDGE('',*,*,#14637,.T.);
#19433=ORIENTED_EDGE('',*,*,#14634,.F.);
#19434=ORIENTED_EDGE('',*,*,#14100,.F.);
#19435=ORIENTED_EDGE('',*,*,#14638,.T.);
#19436=ORIENTED_EDGE('',*,*,#14639,.T.);
#19437=ORIENTED_EDGE('',*,*,#14636,.F.);
#19438=ORIENTED_EDGE('',*,*,#14099,.F.);
#19439=ORIENTED_EDGE('',*,*,#14640,.T.);
#19440=ORIENTED_EDGE('',*,*,#14641,.T.);
#19441=ORIENTED_EDGE('',*,*,#14638,.F.);
#19442=ORIENTED_EDGE('',*,*,#14098,.F.);
#19443=ORIENTED_EDGE('',*,*,#14642,.T.);
#19444=ORIENTED_EDGE('',*,*,#14643,.T.);
#19445=ORIENTED_EDGE('',*,*,#14640,.F.);
#19446=ORIENTED_EDGE('',*,*,#14097,.F.);
#19447=ORIENTED_EDGE('',*,*,#14644,.T.);
#19448=ORIENTED_EDGE('',*,*,#14645,.T.);
#19449=ORIENTED_EDGE('',*,*,#14642,.F.);
#19450=ORIENTED_EDGE('',*,*,#14096,.F.);
#19451=ORIENTED_EDGE('',*,*,#14646,.T.);
#19452=ORIENTED_EDGE('',*,*,#14647,.T.);
#19453=ORIENTED_EDGE('',*,*,#14644,.F.);
#19454=ORIENTED_EDGE('',*,*,#14095,.F.);
#19455=ORIENTED_EDGE('',*,*,#14648,.T.);
#19456=ORIENTED_EDGE('',*,*,#14649,.T.);
#19457=ORIENTED_EDGE('',*,*,#14646,.F.);
#19458=ORIENTED_EDGE('',*,*,#14094,.F.);
#19459=ORIENTED_EDGE('',*,*,#14650,.T.);
#19460=ORIENTED_EDGE('',*,*,#14651,.T.);
#19461=ORIENTED_EDGE('',*,*,#14648,.F.);
#19462=ORIENTED_EDGE('',*,*,#14093,.F.);
#19463=ORIENTED_EDGE('',*,*,#14652,.T.);
#19464=ORIENTED_EDGE('',*,*,#14653,.T.);
#19465=ORIENTED_EDGE('',*,*,#14650,.F.);
#19466=ORIENTED_EDGE('',*,*,#14092,.F.);
#19467=ORIENTED_EDGE('',*,*,#14654,.T.);
#19468=ORIENTED_EDGE('',*,*,#14655,.T.);
#19469=ORIENTED_EDGE('',*,*,#14652,.F.);
#19470=ORIENTED_EDGE('',*,*,#14091,.F.);
#19471=ORIENTED_EDGE('',*,*,#14656,.T.);
#19472=ORIENTED_EDGE('',*,*,#14657,.T.);
#19473=ORIENTED_EDGE('',*,*,#14654,.F.);
#19474=ORIENTED_EDGE('',*,*,#14090,.F.);
#19475=ORIENTED_EDGE('',*,*,#14658,.T.);
#19476=ORIENTED_EDGE('',*,*,#14659,.T.);
#19477=ORIENTED_EDGE('',*,*,#14656,.F.);
#19478=ORIENTED_EDGE('',*,*,#14089,.F.);
#19479=ORIENTED_EDGE('',*,*,#14660,.T.);
#19480=ORIENTED_EDGE('',*,*,#14661,.T.);
#19481=ORIENTED_EDGE('',*,*,#14658,.F.);
#19482=ORIENTED_EDGE('',*,*,#14088,.F.);
#19483=ORIENTED_EDGE('',*,*,#14621,.T.);
#19484=ORIENTED_EDGE('',*,*,#14662,.T.);
#19485=ORIENTED_EDGE('',*,*,#14660,.F.);
#19486=ORIENTED_EDGE('',*,*,#14662,.F.);
#19487=ORIENTED_EDGE('',*,*,#14620,.F.);
#19488=ORIENTED_EDGE('',*,*,#14623,.F.);
#19489=ORIENTED_EDGE('',*,*,#14625,.F.);
#19490=ORIENTED_EDGE('',*,*,#14627,.F.);
#19491=ORIENTED_EDGE('',*,*,#14629,.F.);
#19492=ORIENTED_EDGE('',*,*,#14631,.F.);
#19493=ORIENTED_EDGE('',*,*,#14633,.F.);
#19494=ORIENTED_EDGE('',*,*,#14635,.F.);
#19495=ORIENTED_EDGE('',*,*,#14637,.F.);
#19496=ORIENTED_EDGE('',*,*,#14639,.F.);
#19497=ORIENTED_EDGE('',*,*,#14641,.F.);
#19498=ORIENTED_EDGE('',*,*,#14643,.F.);
#19499=ORIENTED_EDGE('',*,*,#14645,.F.);
#19500=ORIENTED_EDGE('',*,*,#14647,.F.);
#19501=ORIENTED_EDGE('',*,*,#14649,.F.);
#19502=ORIENTED_EDGE('',*,*,#14651,.F.);
#19503=ORIENTED_EDGE('',*,*,#14653,.F.);
#19504=ORIENTED_EDGE('',*,*,#14655,.F.);
#19505=ORIENTED_EDGE('',*,*,#14657,.F.);
#19506=ORIENTED_EDGE('',*,*,#14659,.F.);
#19507=ORIENTED_EDGE('',*,*,#14661,.F.);
#19508=ORIENTED_EDGE('',*,*,#14109,.F.);
#19509=ORIENTED_EDGE('',*,*,#14663,.T.);
#19510=ORIENTED_EDGE('',*,*,#14664,.T.);
#19511=ORIENTED_EDGE('',*,*,#14665,.F.);
#19512=ORIENTED_EDGE('',*,*,#14118,.F.);
#19513=ORIENTED_EDGE('',*,*,#14666,.T.);
#19514=ORIENTED_EDGE('',*,*,#14667,.T.);
#19515=ORIENTED_EDGE('',*,*,#14663,.F.);
#19516=ORIENTED_EDGE('',*,*,#14117,.F.);
#19517=ORIENTED_EDGE('',*,*,#14668,.T.);
#19518=ORIENTED_EDGE('',*,*,#14669,.T.);
#19519=ORIENTED_EDGE('',*,*,#14666,.F.);
#19520=ORIENTED_EDGE('',*,*,#14116,.F.);
#19521=ORIENTED_EDGE('',*,*,#14670,.T.);
#19522=ORIENTED_EDGE('',*,*,#14671,.T.);
#19523=ORIENTED_EDGE('',*,*,#14668,.F.);
#19524=ORIENTED_EDGE('',*,*,#14115,.F.);
#19525=ORIENTED_EDGE('',*,*,#14672,.T.);
#19526=ORIENTED_EDGE('',*,*,#14673,.T.);
#19527=ORIENTED_EDGE('',*,*,#14670,.F.);
#19528=ORIENTED_EDGE('',*,*,#14114,.F.);
#19529=ORIENTED_EDGE('',*,*,#14674,.T.);
#19530=ORIENTED_EDGE('',*,*,#14675,.T.);
#19531=ORIENTED_EDGE('',*,*,#14672,.F.);
#19532=ORIENTED_EDGE('',*,*,#14113,.F.);
#19533=ORIENTED_EDGE('',*,*,#14676,.T.);
#19534=ORIENTED_EDGE('',*,*,#14677,.T.);
#19535=ORIENTED_EDGE('',*,*,#14674,.F.);
#19536=ORIENTED_EDGE('',*,*,#14112,.F.);
#19537=ORIENTED_EDGE('',*,*,#14678,.T.);
#19538=ORIENTED_EDGE('',*,*,#14679,.T.);
#19539=ORIENTED_EDGE('',*,*,#14676,.F.);
#19540=ORIENTED_EDGE('',*,*,#14111,.F.);
#19541=ORIENTED_EDGE('',*,*,#14680,.T.);
#19542=ORIENTED_EDGE('',*,*,#14681,.T.);
#19543=ORIENTED_EDGE('',*,*,#14678,.F.);
#19544=ORIENTED_EDGE('',*,*,#14110,.F.);
#19545=ORIENTED_EDGE('',*,*,#14665,.T.);
#19546=ORIENTED_EDGE('',*,*,#14682,.T.);
#19547=ORIENTED_EDGE('',*,*,#14680,.F.);
#19548=ORIENTED_EDGE('',*,*,#14682,.F.);
#19549=ORIENTED_EDGE('',*,*,#14664,.F.);
#19550=ORIENTED_EDGE('',*,*,#14667,.F.);
#19551=ORIENTED_EDGE('',*,*,#14669,.F.);
#19552=ORIENTED_EDGE('',*,*,#14671,.F.);
#19553=ORIENTED_EDGE('',*,*,#14673,.F.);
#19554=ORIENTED_EDGE('',*,*,#14675,.F.);
#19555=ORIENTED_EDGE('',*,*,#14677,.F.);
#19556=ORIENTED_EDGE('',*,*,#14679,.F.);
#19557=ORIENTED_EDGE('',*,*,#14681,.F.);
#19558=ORIENTED_EDGE('',*,*,#14566,.T.);
#19559=ORIENTED_EDGE('',*,*,#14591,.T.);
#19560=ORIENTED_EDGE('',*,*,#14588,.T.);
#19561=ORIENTED_EDGE('',*,*,#14585,.T.);
#19562=ORIENTED_EDGE('',*,*,#14582,.T.);
#19563=ORIENTED_EDGE('',*,*,#14579,.T.);
#19564=ORIENTED_EDGE('',*,*,#14576,.T.);
#19565=ORIENTED_EDGE('',*,*,#14573,.T.);
#19566=ORIENTED_EDGE('',*,*,#14570,.T.);
#19567=ORIENTED_EDGE('',*,*,#14506,.T.);
#19568=ORIENTED_EDGE('',*,*,#14528,.T.);
#19569=ORIENTED_EDGE('',*,*,#14525,.T.);
#19570=ORIENTED_EDGE('',*,*,#14522,.T.);
#19571=ORIENTED_EDGE('',*,*,#14519,.T.);
#19572=ORIENTED_EDGE('',*,*,#14516,.T.);
#19573=ORIENTED_EDGE('',*,*,#14513,.T.);
#19574=ORIENTED_EDGE('',*,*,#14510,.T.);
#19575=ORIENTED_EDGE('',*,*,#13855,.F.);
#19576=ORIENTED_EDGE('',*,*,#14683,.T.);
#19577=ORIENTED_EDGE('',*,*,#14296,.F.);
#19578=ORIENTED_EDGE('',*,*,#13863,.T.);
#19579=ORIENTED_EDGE('',*,*,#13847,.F.);
#19580=ORIENTED_EDGE('',*,*,#13881,.F.);
#19581=ORIENTED_EDGE('',*,*,#13870,.F.);
#19582=ORIENTED_EDGE('',*,*,#13885,.F.);
#19583=ORIENTED_EDGE('',*,*,#14684,.F.);
#19584=ORIENTED_EDGE('',*,*,#14499,.F.);
#19585=ORIENTED_EDGE('',*,*,#14284,.F.);
#19586=ORIENTED_EDGE('',*,*,#14683,.F.);
#19587=ORIENTED_EDGE('',*,*,#14310,.F.);
#19588=ORIENTED_EDGE('',*,*,#14281,.F.);
#19589=ORIENTED_EDGE('',*,*,#13864,.T.);
#19590=ORIENTED_EDGE('',*,*,#14295,.F.);
#19591=ORIENTED_EDGE('',*,*,#14270,.F.);
#19592=ORIENTED_EDGE('',*,*,#13979,.T.);
#19593=ORIENTED_EDGE('',*,*,#14316,.F.);
#19594=ORIENTED_EDGE('',*,*,#14326,.T.);
#19595=ORIENTED_EDGE('',*,*,#14037,.F.);
#19596=ORIENTED_EDGE('',*,*,#14010,.F.);
#19597=ORIENTED_EDGE('',*,*,#14684,.T.);
#19598=ORIENTED_EDGE('',*,*,#14023,.F.);
#19599=ORIENTED_EDGE('',*,*,#13999,.F.);
#19600=ORIENTED_EDGE('',*,*,#13915,.T.);
#19601=ORIENTED_EDGE('',*,*,#14043,.F.);
#19602=ORIENTED_EDGE('',*,*,#14052,.T.);
#19603=ORIENTED_EDGE('',*,*,#14685,.T.);
#19604=ORIENTED_EDGE('',*,*,#14686,.T.);
#19605=ORIENTED_EDGE('',*,*,#14687,.T.);
#19606=ORIENTED_EDGE('',*,*,#14688,.T.);
#19607=ORIENTED_EDGE('',*,*,#14689,.T.);
#19608=ORIENTED_EDGE('',*,*,#14690,.T.);
#19609=ORIENTED_EDGE('',*,*,#14691,.T.);
#19610=ORIENTED_EDGE('',*,*,#14692,.T.);
#19611=ORIENTED_EDGE('',*,*,#14688,.F.);
#19612=ORIENTED_EDGE('',*,*,#14685,.F.);
#19613=ORIENTED_EDGE('',*,*,#14693,.T.);
#19614=ORIENTED_EDGE('',*,*,#14694,.F.);
#19615=ORIENTED_EDGE('',*,*,#14695,.F.);
#19616=ORIENTED_EDGE('',*,*,#14692,.F.);
#19617=ORIENTED_EDGE('',*,*,#14696,.F.);
#19618=ORIENTED_EDGE('',*,*,#14697,.F.);
#19619=ORIENTED_EDGE('',*,*,#14693,.F.);
#19620=ORIENTED_EDGE('',*,*,#14691,.F.);
#19621=ORIENTED_EDGE('',*,*,#14698,.T.);
#19622=ORIENTED_EDGE('',*,*,#14699,.T.);
#19623=ORIENTED_EDGE('',*,*,#14700,.T.);
#19624=ORIENTED_EDGE('',*,*,#14701,.F.);
#19625=ORIENTED_EDGE('',*,*,#14696,.T.);
#19626=ORIENTED_EDGE('',*,*,#14702,.T.);
#19627=ORIENTED_EDGE('',*,*,#14703,.T.);
#19628=ORIENTED_EDGE('',*,*,#14704,.T.);
#19629=ORIENTED_EDGE('',*,*,#14705,.T.);
#19630=ORIENTED_EDGE('',*,*,#14706,.T.);
#19631=ORIENTED_EDGE('',*,*,#14707,.T.);
#19632=ORIENTED_EDGE('',*,*,#14706,.F.);
#19633=ORIENTED_EDGE('',*,*,#14708,.T.);
#19634=ORIENTED_EDGE('',*,*,#14709,.T.);
#19635=ORIENTED_EDGE('',*,*,#14710,.T.);
#19636=ORIENTED_EDGE('',*,*,#14711,.T.);
#19637=ORIENTED_EDGE('',*,*,#14712,.T.);
#19638=ORIENTED_EDGE('',*,*,#14713,.T.);
#19639=ORIENTED_EDGE('',*,*,#14709,.F.);
#19640=ORIENTED_EDGE('',*,*,#14703,.F.);
#19641=ORIENTED_EDGE('',*,*,#14714,.T.);
#19642=ORIENTED_EDGE('',*,*,#14715,.T.);
#19643=ORIENTED_EDGE('',*,*,#14716,.T.);
#19644=ORIENTED_EDGE('',*,*,#14717,.T.);
#19645=ORIENTED_EDGE('',*,*,#14718,.T.);
#19646=ORIENTED_EDGE('',*,*,#14702,.F.);
#19647=ORIENTED_EDGE('',*,*,#14719,.T.);
#19648=ORIENTED_EDGE('',*,*,#14720,.F.);
#19649=ORIENTED_EDGE('',*,*,#14714,.F.);
#19650=ORIENTED_EDGE('',*,*,#14707,.F.);
#19651=ORIENTED_EDGE('',*,*,#14721,.T.);
#19652=ORIENTED_EDGE('',*,*,#14722,.F.);
#19653=ORIENTED_EDGE('',*,*,#14719,.F.);
#19654=ORIENTED_EDGE('',*,*,#14713,.F.);
#19655=ORIENTED_EDGE('',*,*,#14723,.F.);
#19656=ORIENTED_EDGE('',*,*,#14724,.F.);
#19657=ORIENTED_EDGE('',*,*,#14721,.F.);
#19658=ORIENTED_EDGE('',*,*,#14712,.F.);
#19659=ORIENTED_EDGE('',*,*,#14725,.T.);
#19660=ORIENTED_EDGE('',*,*,#14726,.T.);
#19661=ORIENTED_EDGE('',*,*,#14727,.T.);
#19662=ORIENTED_EDGE('',*,*,#14728,.F.);
#19663=ORIENTED_EDGE('',*,*,#14723,.T.);
#19664=ORIENTED_EDGE('',*,*,#14729,.T.);
#19665=ORIENTED_EDGE('',*,*,#14730,.T.);
#19666=ORIENTED_EDGE('',*,*,#14731,.T.);
#19667=ORIENTED_EDGE('',*,*,#14732,.T.);
#19668=ORIENTED_EDGE('',*,*,#14733,.T.);
#19669=ORIENTED_EDGE('',*,*,#14734,.T.);
#19670=ORIENTED_EDGE('',*,*,#14729,.F.);
#19671=ORIENTED_EDGE('',*,*,#14735,.T.);
#19672=ORIENTED_EDGE('',*,*,#14736,.T.);
#19673=ORIENTED_EDGE('',*,*,#14737,.T.);
#19674=ORIENTED_EDGE('',*,*,#14738,.T.);
#19675=ORIENTED_EDGE('',*,*,#14734,.F.);
#19676=ORIENTED_EDGE('',*,*,#14739,.T.);
#19677=ORIENTED_EDGE('',*,*,#14740,.F.);
#19678=ORIENTED_EDGE('',*,*,#14741,.F.);
#19679=ORIENTED_EDGE('',*,*,#14742,.T.);
#19680=ORIENTED_EDGE('',*,*,#14735,.F.);
#19681=ORIENTED_EDGE('',*,*,#14743,.F.);
#19682=ORIENTED_EDGE('',*,*,#14739,.F.);
#19683=ORIENTED_EDGE('',*,*,#14733,.F.);
#19684=ORIENTED_EDGE('',*,*,#14744,.F.);
#19685=ORIENTED_EDGE('',*,*,#14745,.F.);
#19686=ORIENTED_EDGE('',*,*,#14746,.F.);
#19687=ORIENTED_EDGE('',*,*,#14689,.F.);
#19688=ORIENTED_EDGE('',*,*,#14687,.F.);
#19689=ORIENTED_EDGE('',*,*,#14747,.T.);
#19690=ORIENTED_EDGE('',*,*,#14748,.T.);
#19691=ORIENTED_EDGE('',*,*,#14749,.T.);
#19692=ORIENTED_EDGE('',*,*,#14750,.T.);
#19693=ORIENTED_EDGE('',*,*,#14751,.T.);
#19694=ORIENTED_EDGE('',*,*,#14752,.T.);
#19695=ORIENTED_EDGE('',*,*,#14753,.T.);
#19696=ORIENTED_EDGE('',*,*,#14754,.T.);
#19697=ORIENTED_EDGE('',*,*,#14755,.T.);
#19698=ORIENTED_EDGE('',*,*,#14751,.F.);
#19699=ORIENTED_EDGE('',*,*,#14747,.F.);
#19700=ORIENTED_EDGE('',*,*,#14755,.F.);
#19701=ORIENTED_EDGE('',*,*,#14756,.F.);
#19702=ORIENTED_EDGE('',*,*,#14757,.F.);
#19703=ORIENTED_EDGE('',*,*,#14736,.F.);
#19704=ORIENTED_EDGE('',*,*,#14742,.F.);
#19705=ORIENTED_EDGE('',*,*,#14758,.F.);
#19706=ORIENTED_EDGE('',*,*,#14759,.F.);
#19707=ORIENTED_EDGE('',*,*,#14754,.F.);
#19708=ORIENTED_EDGE('',*,*,#14760,.F.);
#19709=ORIENTED_EDGE('',*,*,#14761,.T.);
#19710=ORIENTED_EDGE('',*,*,#14762,.T.);
#19711=ORIENTED_EDGE('',*,*,#14763,.F.);
#19712=ORIENTED_EDGE('',*,*,#14756,.T.);
#19713=ORIENTED_EDGE('',*,*,#14753,.F.);
#19714=ORIENTED_EDGE('',*,*,#14764,.T.);
#19715=ORIENTED_EDGE('',*,*,#14765,.F.);
#19716=ORIENTED_EDGE('',*,*,#14766,.F.);
#19717=ORIENTED_EDGE('',*,*,#14767,.T.);
#19718=ORIENTED_EDGE('',*,*,#14760,.T.);
#19719=ORIENTED_EDGE('',*,*,#14740,.T.);
#19720=ORIENTED_EDGE('',*,*,#14743,.T.);
#19721=ORIENTED_EDGE('',*,*,#14686,.F.);
#19722=ORIENTED_EDGE('',*,*,#14768,.T.);
#19723=ORIENTED_EDGE('',*,*,#14769,.T.);
#19724=ORIENTED_EDGE('',*,*,#14769,.F.);
#19725=ORIENTED_EDGE('',*,*,#14770,.T.);
#19726=ORIENTED_EDGE('',*,*,#14771,.T.);
#19727=ORIENTED_EDGE('',*,*,#14772,.T.);
#19728=ORIENTED_EDGE('',*,*,#14758,.T.);
#19729=ORIENTED_EDGE('',*,*,#14741,.T.);
#19730=ORIENTED_EDGE('',*,*,#14748,.F.);
#19731=ORIENTED_EDGE('',*,*,#14759,.T.);
#19732=ORIENTED_EDGE('',*,*,#14772,.F.);
#19733=ORIENTED_EDGE('',*,*,#14773,.F.);
#19734=ORIENTED_EDGE('',*,*,#14774,.T.);
#19735=ORIENTED_EDGE('',*,*,#14775,.F.);
#19736=ORIENTED_EDGE('',*,*,#14771,.F.);
#19737=ORIENTED_EDGE('',*,*,#14776,.T.);
#19738=ORIENTED_EDGE('',*,*,#14777,.F.);
#19739=ORIENTED_EDGE('',*,*,#14778,.T.);
#19740=ORIENTED_EDGE('',*,*,#14773,.T.);
#19741=ORIENTED_EDGE('',*,*,#14704,.F.);
#19742=ORIENTED_EDGE('',*,*,#14718,.F.);
#19743=ORIENTED_EDGE('',*,*,#14779,.T.);
#19744=ORIENTED_EDGE('',*,*,#14780,.F.);
#19745=ORIENTED_EDGE('',*,*,#14781,.F.);
#19746=ORIENTED_EDGE('',*,*,#14782,.T.);
#19747=ORIENTED_EDGE('',*,*,#14717,.F.);
#19748=ORIENTED_EDGE('',*,*,#14783,.F.);
#19749=ORIENTED_EDGE('',*,*,#14784,.F.);
#19750=ORIENTED_EDGE('',*,*,#14785,.F.);
#19751=ORIENTED_EDGE('',*,*,#14786,.F.);
#19752=ORIENTED_EDGE('',*,*,#14787,.F.);
#19753=ORIENTED_EDGE('',*,*,#14788,.F.);
#19754=ORIENTED_EDGE('',*,*,#14779,.F.);
#19755=ORIENTED_EDGE('',*,*,#14780,.T.);
#19756=ORIENTED_EDGE('',*,*,#14788,.T.);
#19757=ORIENTED_EDGE('',*,*,#14789,.T.);
#19758=ORIENTED_EDGE('',*,*,#14790,.T.);
#19759=ORIENTED_EDGE('',*,*,#14791,.T.);
#19760=ORIENTED_EDGE('',*,*,#14791,.F.);
#19761=ORIENTED_EDGE('',*,*,#14792,.T.);
#19762=ORIENTED_EDGE('',*,*,#14793,.T.);
#19763=ORIENTED_EDGE('',*,*,#14794,.T.);
#19764=ORIENTED_EDGE('',*,*,#14781,.T.);
#19765=ORIENTED_EDGE('',*,*,#14757,.T.);
#19766=ORIENTED_EDGE('',*,*,#14763,.T.);
#19767=ORIENTED_EDGE('',*,*,#14795,.T.);
#19768=ORIENTED_EDGE('',*,*,#14796,.T.);
#19769=ORIENTED_EDGE('',*,*,#14737,.F.);
#19770=ORIENTED_EDGE('',*,*,#14730,.F.);
#19771=ORIENTED_EDGE('',*,*,#14738,.F.);
#19772=ORIENTED_EDGE('',*,*,#14797,.T.);
#19773=ORIENTED_EDGE('',*,*,#14798,.F.);
#19774=ORIENTED_EDGE('',*,*,#14796,.F.);
#19775=ORIENTED_EDGE('',*,*,#14799,.F.);
#19776=ORIENTED_EDGE('',*,*,#14800,.F.);
#19777=ORIENTED_EDGE('',*,*,#14801,.F.);
#19778=ORIENTED_EDGE('',*,*,#14802,.F.);
#19779=ORIENTED_EDGE('',*,*,#14803,.F.);
#19780=ORIENTED_EDGE('',*,*,#14804,.F.);
#19781=ORIENTED_EDGE('',*,*,#14805,.T.);
#19782=ORIENTED_EDGE('',*,*,#14806,.T.);
#19783=ORIENTED_EDGE('',*,*,#14797,.F.);
#19784=ORIENTED_EDGE('',*,*,#14795,.F.);
#19785=ORIENTED_EDGE('',*,*,#14762,.F.);
#19786=ORIENTED_EDGE('',*,*,#14807,.T.);
#19787=ORIENTED_EDGE('',*,*,#14808,.T.);
#19788=ORIENTED_EDGE('',*,*,#14809,.F.);
#19789=ORIENTED_EDGE('',*,*,#14799,.T.);
#19790=ORIENTED_EDGE('',*,*,#14810,.F.);
#19791=ORIENTED_EDGE('',*,*,#14811,.F.);
#19792=ORIENTED_EDGE('',*,*,#14793,.F.);
#19793=ORIENTED_EDGE('',*,*,#14812,.T.);
#19794=ORIENTED_EDGE('',*,*,#14813,.T.);
#19795=ORIENTED_EDGE('',*,*,#14811,.T.);
#19796=ORIENTED_EDGE('',*,*,#14814,.T.);
#19797=ORIENTED_EDGE('',*,*,#14815,.T.);
#19798=ORIENTED_EDGE('',*,*,#14816,.T.);
#19799=ORIENTED_EDGE('',*,*,#14817,.T.);
#19800=ORIENTED_EDGE('',*,*,#14810,.T.);
#19801=ORIENTED_EDGE('',*,*,#14818,.T.);
#19802=ORIENTED_EDGE('',*,*,#14705,.F.);
#19803=ORIENTED_EDGE('',*,*,#14782,.F.);
#19804=ORIENTED_EDGE('',*,*,#14794,.F.);
#19805=ORIENTED_EDGE('',*,*,#14813,.F.);
#19806=ORIENTED_EDGE('',*,*,#14819,.F.);
#19807=ORIENTED_EDGE('',*,*,#14820,.F.);
#19808=ORIENTED_EDGE('',*,*,#14710,.F.);
#19809=ORIENTED_EDGE('',*,*,#14708,.F.);
#19810=ORIENTED_EDGE('',*,*,#14812,.F.);
#19811=ORIENTED_EDGE('',*,*,#14821,.T.);
#19812=ORIENTED_EDGE('',*,*,#14822,.T.);
#19813=ORIENTED_EDGE('',*,*,#14823,.F.);
#19814=ORIENTED_EDGE('',*,*,#14824,.T.);
#19815=ORIENTED_EDGE('',*,*,#14819,.T.);
#19816=ORIENTED_EDGE('',*,*,#14815,.F.);
#19817=ORIENTED_EDGE('',*,*,#14825,.T.);
#19818=ORIENTED_EDGE('',*,*,#14802,.T.);
#19819=ORIENTED_EDGE('',*,*,#14826,.T.);
#19820=ORIENTED_EDGE('',*,*,#14821,.F.);
#19821=ORIENTED_EDGE('',*,*,#14814,.F.);
#19822=ORIENTED_EDGE('',*,*,#14817,.F.);
#19823=ORIENTED_EDGE('',*,*,#14827,.T.);
#19824=ORIENTED_EDGE('',*,*,#14828,.T.);
#19825=ORIENTED_EDGE('',*,*,#14829,.T.);
#19826=ORIENTED_EDGE('',*,*,#14830,.F.);
#19827=ORIENTED_EDGE('',*,*,#14831,.F.);
#19828=ORIENTED_EDGE('',*,*,#14832,.F.);
#19829=ORIENTED_EDGE('',*,*,#14833,.F.);
#19830=ORIENTED_EDGE('',*,*,#14834,.F.);
#19831=ORIENTED_EDGE('',*,*,#14835,.T.);
#19832=ORIENTED_EDGE('',*,*,#14836,.T.);
#19833=ORIENTED_EDGE('',*,*,#14837,.F.);
#19834=ORIENTED_EDGE('',*,*,#14838,.F.);
#19835=ORIENTED_EDGE('',*,*,#14803,.T.);
#19836=ORIENTED_EDGE('',*,*,#14825,.F.);
#19837=ORIENTED_EDGE('',*,*,#14839,.T.);
#19838=ORIENTED_EDGE('',*,*,#14840,.T.);
#19839=ORIENTED_EDGE('',*,*,#14841,.T.);
#19840=ORIENTED_EDGE('',*,*,#14834,.T.);
#19841=ORIENTED_EDGE('',*,*,#14842,.T.);
#19842=ORIENTED_EDGE('',*,*,#14839,.F.);
#19843=ORIENTED_EDGE('',*,*,#14843,.F.);
#19844=ORIENTED_EDGE('',*,*,#14844,.T.);
#19845=ORIENTED_EDGE('',*,*,#14845,.T.);
#19846=ORIENTED_EDGE('',*,*,#14846,.T.);
#19847=ORIENTED_EDGE('',*,*,#14847,.T.);
#19848=ORIENTED_EDGE('',*,*,#14842,.F.);
#19849=ORIENTED_EDGE('',*,*,#14833,.T.);
#19850=ORIENTED_EDGE('',*,*,#14848,.F.);
#19851=ORIENTED_EDGE('',*,*,#14849,.F.);
#19852=ORIENTED_EDGE('',*,*,#14850,.T.);
#19853=ORIENTED_EDGE('',*,*,#14843,.T.);
#19854=ORIENTED_EDGE('',*,*,#14784,.T.);
#19855=ORIENTED_EDGE('',*,*,#14851,.T.);
#19856=ORIENTED_EDGE('',*,*,#14852,.T.);
#19857=ORIENTED_EDGE('',*,*,#14853,.T.);
#19858=ORIENTED_EDGE('',*,*,#14854,.T.);
#19859=ORIENTED_EDGE('',*,*,#14855,.T.);
#19860=ORIENTED_EDGE('',*,*,#14856,.T.);
#19861=ORIENTED_EDGE('',*,*,#14857,.T.);
#19862=ORIENTED_EDGE('',*,*,#14785,.T.);
#19863=ORIENTED_EDGE('',*,*,#14854,.F.);
#19864=ORIENTED_EDGE('',*,*,#14716,.F.);
#19865=ORIENTED_EDGE('',*,*,#14858,.F.);
#19866=ORIENTED_EDGE('',*,*,#14859,.T.);
#19867=ORIENTED_EDGE('',*,*,#14860,.F.);
#19868=ORIENTED_EDGE('',*,*,#14851,.F.);
#19869=ORIENTED_EDGE('',*,*,#14783,.T.);
#19870=ORIENTED_EDGE('',*,*,#14857,.F.);
#19871=ORIENTED_EDGE('',*,*,#14861,.F.);
#19872=ORIENTED_EDGE('',*,*,#14862,.T.);
#19873=ORIENTED_EDGE('',*,*,#14863,.F.);
#19874=ORIENTED_EDGE('',*,*,#14864,.F.);
#19875=ORIENTED_EDGE('',*,*,#14786,.T.);
#19876=ORIENTED_EDGE('',*,*,#14865,.T.);
#19877=ORIENTED_EDGE('',*,*,#14866,.T.);
#19878=ORIENTED_EDGE('',*,*,#14830,.T.);
#19879=ORIENTED_EDGE('',*,*,#14867,.T.);
#19880=ORIENTED_EDGE('',*,*,#14855,.F.);
#19881=ORIENTED_EDGE('',*,*,#14868,.F.);
#19882=ORIENTED_EDGE('',*,*,#14869,.F.);
#19883=ORIENTED_EDGE('',*,*,#14831,.T.);
#19884=ORIENTED_EDGE('',*,*,#14866,.F.);
#19885=ORIENTED_EDGE('',*,*,#14870,.T.);
#19886=ORIENTED_EDGE('',*,*,#14871,.T.);
#19887=ORIENTED_EDGE('',*,*,#14872,.F.);
#19888=ORIENTED_EDGE('',*,*,#14873,.F.);
#19889=ORIENTED_EDGE('',*,*,#14874,.F.);
#19890=ORIENTED_EDGE('',*,*,#14848,.T.);
#19891=ORIENTED_EDGE('',*,*,#14832,.T.);
#19892=ORIENTED_EDGE('',*,*,#14869,.T.);
#19893=ORIENTED_EDGE('',*,*,#14875,.T.);
#19894=ORIENTED_EDGE('',*,*,#14876,.T.);
#19895=ORIENTED_EDGE('',*,*,#14852,.F.);
#19896=ORIENTED_EDGE('',*,*,#14860,.T.);
#19897=ORIENTED_EDGE('',*,*,#14877,.T.);
#19898=ORIENTED_EDGE('',*,*,#14849,.T.);
#19899=ORIENTED_EDGE('',*,*,#14876,.F.);
#19900=ORIENTED_EDGE('',*,*,#14878,.T.);
#19901=ORIENTED_EDGE('',*,*,#14724,.T.);
#19902=ORIENTED_EDGE('',*,*,#14728,.T.);
#19903=ORIENTED_EDGE('',*,*,#14879,.T.);
#19904=ORIENTED_EDGE('',*,*,#14880,.T.);
#19905=ORIENTED_EDGE('',*,*,#14881,.T.);
#19906=ORIENTED_EDGE('',*,*,#14882,.T.);
#19907=ORIENTED_EDGE('',*,*,#14883,.T.);
#19908=ORIENTED_EDGE('',*,*,#14722,.T.);
#19909=ORIENTED_EDGE('',*,*,#14881,.F.);
#19910=ORIENTED_EDGE('',*,*,#14715,.F.);
#19911=ORIENTED_EDGE('',*,*,#14720,.T.);
#19912=ORIENTED_EDGE('',*,*,#14883,.F.);
#19913=ORIENTED_EDGE('',*,*,#14884,.T.);
#19914=ORIENTED_EDGE('',*,*,#14858,.T.);
#19915=ORIENTED_EDGE('',*,*,#14884,.F.);
#19916=ORIENTED_EDGE('',*,*,#14882,.F.);
#19917=ORIENTED_EDGE('',*,*,#14880,.F.);
#19918=ORIENTED_EDGE('',*,*,#14885,.F.);
#19919=ORIENTED_EDGE('',*,*,#14844,.F.);
#19920=ORIENTED_EDGE('',*,*,#14850,.F.);
#19921=ORIENTED_EDGE('',*,*,#14877,.F.);
#19922=ORIENTED_EDGE('',*,*,#14859,.F.);
#19923=ORIENTED_EDGE('',*,*,#14879,.F.);
#19924=ORIENTED_EDGE('',*,*,#14727,.F.);
#19925=ORIENTED_EDGE('',*,*,#14886,.T.);
#19926=ORIENTED_EDGE('',*,*,#14887,.F.);
#19927=ORIENTED_EDGE('',*,*,#14845,.F.);
#19928=ORIENTED_EDGE('',*,*,#14885,.T.);
#19929=ORIENTED_EDGE('',*,*,#14853,.F.);
#19930=ORIENTED_EDGE('',*,*,#14878,.F.);
#19931=ORIENTED_EDGE('',*,*,#14875,.F.);
#19932=ORIENTED_EDGE('',*,*,#14868,.T.);
#19933=ORIENTED_EDGE('',*,*,#14840,.F.);
#19934=ORIENTED_EDGE('',*,*,#14847,.F.);
#19935=ORIENTED_EDGE('',*,*,#14888,.F.);
#19936=ORIENTED_EDGE('',*,*,#14889,.T.);
#19937=ORIENTED_EDGE('',*,*,#14846,.F.);
#19938=ORIENTED_EDGE('',*,*,#14887,.T.);
#19939=ORIENTED_EDGE('',*,*,#14890,.T.);
#19940=ORIENTED_EDGE('',*,*,#14891,.T.);
#19941=ORIENTED_EDGE('',*,*,#14888,.T.);
#19942=ORIENTED_EDGE('',*,*,#14726,.F.);
#19943=ORIENTED_EDGE('',*,*,#14892,.F.);
#19944=ORIENTED_EDGE('',*,*,#14893,.F.);
#19945=ORIENTED_EDGE('',*,*,#14894,.F.);
#19946=ORIENTED_EDGE('',*,*,#14895,.F.);
#19947=ORIENTED_EDGE('',*,*,#14896,.F.);
#19948=ORIENTED_EDGE('',*,*,#14890,.F.);
#19949=ORIENTED_EDGE('',*,*,#14886,.F.);
#19950=ORIENTED_EDGE('',*,*,#14896,.T.);
#19951=ORIENTED_EDGE('',*,*,#14897,.T.);
#19952=ORIENTED_EDGE('',*,*,#14765,.T.);
#19953=ORIENTED_EDGE('',*,*,#14898,.T.);
#19954=ORIENTED_EDGE('',*,*,#14891,.F.);
#19955=ORIENTED_EDGE('',*,*,#14897,.F.);
#19956=ORIENTED_EDGE('',*,*,#14895,.T.);
#19957=ORIENTED_EDGE('',*,*,#14899,.F.);
#19958=ORIENTED_EDGE('',*,*,#14808,.F.);
#19959=ORIENTED_EDGE('',*,*,#14900,.T.);
#19960=ORIENTED_EDGE('',*,*,#14766,.T.);
#19961=ORIENTED_EDGE('',*,*,#14800,.T.);
#19962=ORIENTED_EDGE('',*,*,#14809,.T.);
#19963=ORIENTED_EDGE('',*,*,#14899,.T.);
#19964=ORIENTED_EDGE('',*,*,#14894,.T.);
#19965=ORIENTED_EDGE('',*,*,#14901,.T.);
#19966=ORIENTED_EDGE('',*,*,#14893,.T.);
#19967=ORIENTED_EDGE('',*,*,#14902,.T.);
#19968=ORIENTED_EDGE('',*,*,#14823,.T.);
#19969=ORIENTED_EDGE('',*,*,#14903,.T.);
#19970=ORIENTED_EDGE('',*,*,#14901,.F.);
#19971=ORIENTED_EDGE('',*,*,#14903,.F.);
#19972=ORIENTED_EDGE('',*,*,#14822,.F.);
#19973=ORIENTED_EDGE('',*,*,#14826,.F.);
#19974=ORIENTED_EDGE('',*,*,#14801,.T.);
#19975=ORIENTED_EDGE('',*,*,#14904,.T.);
#19976=ORIENTED_EDGE('',*,*,#14905,.T.);
#19977=ORIENTED_EDGE('',*,*,#14789,.F.);
#19978=ORIENTED_EDGE('',*,*,#14787,.T.);
#19979=ORIENTED_EDGE('',*,*,#14864,.T.);
#19980=ORIENTED_EDGE('',*,*,#14828,.F.);
#19981=ORIENTED_EDGE('',*,*,#14906,.T.);
#19982=ORIENTED_EDGE('',*,*,#14907,.T.);
#19983=ORIENTED_EDGE('',*,*,#14908,.T.);
#19984=ORIENTED_EDGE('',*,*,#14905,.F.);
#19985=ORIENTED_EDGE('',*,*,#14909,.F.);
#19986=ORIENTED_EDGE('',*,*,#14910,.F.);
#19987=ORIENTED_EDGE('',*,*,#14911,.F.);
#19988=ORIENTED_EDGE('',*,*,#14912,.F.);
#19989=ORIENTED_EDGE('',*,*,#14913,.T.);
#19990=ORIENTED_EDGE('',*,*,#14906,.F.);
#19991=ORIENTED_EDGE('',*,*,#14827,.F.);
#19992=ORIENTED_EDGE('',*,*,#14816,.F.);
#19993=ORIENTED_EDGE('',*,*,#14914,.F.);
#19994=ORIENTED_EDGE('',*,*,#14836,.F.);
#19995=ORIENTED_EDGE('',*,*,#14915,.T.);
#19996=ORIENTED_EDGE('',*,*,#14916,.T.);
#19997=ORIENTED_EDGE('',*,*,#14917,.T.);
#19998=ORIENTED_EDGE('',*,*,#14917,.F.);
#19999=ORIENTED_EDGE('',*,*,#14918,.F.);
#20000=ORIENTED_EDGE('',*,*,#14919,.F.);
#20001=ORIENTED_EDGE('',*,*,#14837,.T.);
#20002=ORIENTED_EDGE('',*,*,#14920,.F.);
#20003=ORIENTED_EDGE('',*,*,#14921,.F.);
#20004=ORIENTED_EDGE('',*,*,#14922,.T.);
#20005=ORIENTED_EDGE('',*,*,#14923,.T.);
#20006=ORIENTED_EDGE('',*,*,#14924,.T.);
#20007=ORIENTED_EDGE('',*,*,#14925,.T.);
#20008=ORIENTED_EDGE('',*,*,#14926,.T.);
#20009=ORIENTED_EDGE('',*,*,#14927,.F.);
#20010=ORIENTED_EDGE('',*,*,#14923,.F.);
#20011=ORIENTED_EDGE('',*,*,#14928,.F.);
#20012=ORIENTED_EDGE('',*,*,#14929,.F.);
#20013=ORIENTED_EDGE('',*,*,#14870,.F.);
#20014=ORIENTED_EDGE('',*,*,#14865,.F.);
#20015=ORIENTED_EDGE('',*,*,#14930,.F.);
#20016=ORIENTED_EDGE('',*,*,#14907,.F.);
#20017=ORIENTED_EDGE('',*,*,#14913,.F.);
#20018=ORIENTED_EDGE('',*,*,#14931,.F.);
#20019=ORIENTED_EDGE('',*,*,#14932,.F.);
#20020=ORIENTED_EDGE('',*,*,#14933,.F.);
#20021=ORIENTED_EDGE('',*,*,#14805,.F.);
#20022=ORIENTED_EDGE('',*,*,#14934,.F.);
#20023=ORIENTED_EDGE('',*,*,#14918,.T.);
#20024=ORIENTED_EDGE('',*,*,#14916,.F.);
#20025=ORIENTED_EDGE('',*,*,#14922,.F.);
#20026=ORIENTED_EDGE('',*,*,#14935,.F.);
#20027=ORIENTED_EDGE('',*,*,#14936,.T.);
#20028=ORIENTED_EDGE('',*,*,#14937,.T.);
#20029=ORIENTED_EDGE('',*,*,#14928,.T.);
#20030=ORIENTED_EDGE('',*,*,#14749,.F.);
#20031=ORIENTED_EDGE('',*,*,#14775,.T.);
#20032=ORIENTED_EDGE('',*,*,#14938,.T.);
#20033=ORIENTED_EDGE('',*,*,#14935,.T.);
#20034=ORIENTED_EDGE('',*,*,#14926,.F.);
#20035=ORIENTED_EDGE('',*,*,#14939,.T.);
#20036=ORIENTED_EDGE('',*,*,#14711,.F.);
#20037=ORIENTED_EDGE('',*,*,#14820,.T.);
#20038=ORIENTED_EDGE('',*,*,#14824,.F.);
#20039=ORIENTED_EDGE('',*,*,#14902,.F.);
#20040=ORIENTED_EDGE('',*,*,#14892,.T.);
#20041=ORIENTED_EDGE('',*,*,#14725,.F.);
#20042=ORIENTED_EDGE('',*,*,#14838,.T.);
#20043=ORIENTED_EDGE('',*,*,#14919,.T.);
#20044=ORIENTED_EDGE('',*,*,#14934,.T.);
#20045=ORIENTED_EDGE('',*,*,#14804,.T.);
#20046=ORIENTED_EDGE('',*,*,#14732,.F.);
#20047=ORIENTED_EDGE('',*,*,#14940,.T.);
#20048=ORIENTED_EDGE('',*,*,#14932,.T.);
#20049=ORIENTED_EDGE('',*,*,#14941,.T.);
#20050=ORIENTED_EDGE('',*,*,#14942,.T.);
#20051=ORIENTED_EDGE('',*,*,#14744,.T.);
#20052=ORIENTED_EDGE('',*,*,#14731,.F.);
#20053=ORIENTED_EDGE('',*,*,#14798,.T.);
#20054=ORIENTED_EDGE('',*,*,#14806,.F.);
#20055=ORIENTED_EDGE('',*,*,#14933,.T.);
#20056=ORIENTED_EDGE('',*,*,#14940,.F.);
#20057=ORIENTED_EDGE('',*,*,#14941,.F.);
#20058=ORIENTED_EDGE('',*,*,#14931,.T.);
#20059=ORIENTED_EDGE('',*,*,#14912,.T.);
#20060=ORIENTED_EDGE('',*,*,#14943,.T.);
#20061=ORIENTED_EDGE('',*,*,#14944,.F.);
#20062=ORIENTED_EDGE('',*,*,#14697,.T.);
#20063=ORIENTED_EDGE('',*,*,#14701,.T.);
#20064=ORIENTED_EDGE('',*,*,#14945,.T.);
#20065=ORIENTED_EDGE('',*,*,#14946,.T.);
#20066=ORIENTED_EDGE('',*,*,#14947,.T.);
#20067=ORIENTED_EDGE('',*,*,#14948,.T.);
#20068=ORIENTED_EDGE('',*,*,#14777,.T.);
#20069=ORIENTED_EDGE('',*,*,#14694,.T.);
#20070=ORIENTED_EDGE('',*,*,#14947,.F.);
#20071=ORIENTED_EDGE('',*,*,#14778,.F.);
#20072=ORIENTED_EDGE('',*,*,#14948,.F.);
#20073=ORIENTED_EDGE('',*,*,#14946,.F.);
#20074=ORIENTED_EDGE('',*,*,#14949,.F.);
#20075=ORIENTED_EDGE('',*,*,#14950,.F.);
#20076=ORIENTED_EDGE('',*,*,#14936,.F.);
#20077=ORIENTED_EDGE('',*,*,#14938,.F.);
#20078=ORIENTED_EDGE('',*,*,#14774,.F.);
#20079=ORIENTED_EDGE('',*,*,#14945,.F.);
#20080=ORIENTED_EDGE('',*,*,#14700,.F.);
#20081=ORIENTED_EDGE('',*,*,#14951,.T.);
#20082=ORIENTED_EDGE('',*,*,#14952,.F.);
#20083=ORIENTED_EDGE('',*,*,#14953,.F.);
#20084=ORIENTED_EDGE('',*,*,#14949,.T.);
#20085=ORIENTED_EDGE('',*,*,#14954,.F.);
#20086=ORIENTED_EDGE('',*,*,#14955,.F.);
#20087=ORIENTED_EDGE('',*,*,#14937,.F.);
#20088=ORIENTED_EDGE('',*,*,#14871,.F.);
#20089=ORIENTED_EDGE('',*,*,#14929,.T.);
#20090=ORIENTED_EDGE('',*,*,#14955,.T.);
#20091=ORIENTED_EDGE('',*,*,#14956,.T.);
#20092=ORIENTED_EDGE('',*,*,#14957,.T.);
#20093=ORIENTED_EDGE('',*,*,#14958,.T.);
#20094=ORIENTED_EDGE('',*,*,#14954,.T.);
#20095=ORIENTED_EDGE('',*,*,#14950,.T.);
#20096=ORIENTED_EDGE('',*,*,#14953,.T.);
#20097=ORIENTED_EDGE('',*,*,#14956,.F.);
#20098=ORIENTED_EDGE('',*,*,#14958,.F.);
#20099=ORIENTED_EDGE('',*,*,#14959,.F.);
#20100=ORIENTED_EDGE('',*,*,#14872,.T.);
#20101=ORIENTED_EDGE('',*,*,#14957,.F.);
#20102=ORIENTED_EDGE('',*,*,#14952,.T.);
#20103=ORIENTED_EDGE('',*,*,#14960,.T.);
#20104=ORIENTED_EDGE('',*,*,#14961,.T.);
#20105=ORIENTED_EDGE('',*,*,#14959,.T.);
#20106=ORIENTED_EDGE('',*,*,#14942,.F.);
#20107=ORIENTED_EDGE('',*,*,#14944,.T.);
#20108=ORIENTED_EDGE('',*,*,#14962,.T.);
#20109=ORIENTED_EDGE('',*,*,#14963,.T.);
#20110=ORIENTED_EDGE('',*,*,#14964,.T.);
#20111=ORIENTED_EDGE('',*,*,#14745,.T.);
#20112=ORIENTED_EDGE('',*,*,#14963,.F.);
#20113=ORIENTED_EDGE('',*,*,#14965,.T.);
#20114=ORIENTED_EDGE('',*,*,#14966,.F.);
#20115=ORIENTED_EDGE('',*,*,#14967,.T.);
#20116=ORIENTED_EDGE('',*,*,#14968,.T.);
#20117=ORIENTED_EDGE('',*,*,#14962,.F.);
#20118=ORIENTED_EDGE('',*,*,#14943,.F.);
#20119=ORIENTED_EDGE('',*,*,#14911,.T.);
#20120=ORIENTED_EDGE('',*,*,#14965,.F.);
#20121=ORIENTED_EDGE('',*,*,#14699,.F.);
#20122=ORIENTED_EDGE('',*,*,#14969,.F.);
#20123=ORIENTED_EDGE('',*,*,#14967,.F.);
#20124=ORIENTED_EDGE('',*,*,#14970,.F.);
#20125=ORIENTED_EDGE('',*,*,#14971,.F.);
#20126=ORIENTED_EDGE('',*,*,#14972,.F.);
#20127=ORIENTED_EDGE('',*,*,#14960,.F.);
#20128=ORIENTED_EDGE('',*,*,#14951,.F.);
#20129=ORIENTED_EDGE('',*,*,#14972,.T.);
#20130=ORIENTED_EDGE('',*,*,#14973,.T.);
#20131=ORIENTED_EDGE('',*,*,#14974,.T.);
#20132=ORIENTED_EDGE('',*,*,#14873,.T.);
#20133=ORIENTED_EDGE('',*,*,#14961,.F.);
#20134=ORIENTED_EDGE('',*,*,#14856,.F.);
#20135=ORIENTED_EDGE('',*,*,#14874,.T.);
#20136=ORIENTED_EDGE('',*,*,#14974,.F.);
#20137=ORIENTED_EDGE('',*,*,#14975,.F.);
#20138=ORIENTED_EDGE('',*,*,#14976,.T.);
#20139=ORIENTED_EDGE('',*,*,#14861,.T.);
#20140=ORIENTED_EDGE('',*,*,#14973,.F.);
#20141=ORIENTED_EDGE('',*,*,#14971,.T.);
#20142=ORIENTED_EDGE('',*,*,#14977,.F.);
#20143=ORIENTED_EDGE('',*,*,#14978,.F.);
#20144=ORIENTED_EDGE('',*,*,#14979,.T.);
#20145=ORIENTED_EDGE('',*,*,#14975,.T.);
#20146=ORIENTED_EDGE('',*,*,#14910,.T.);
#20147=ORIENTED_EDGE('',*,*,#14980,.T.);
#20148=ORIENTED_EDGE('',*,*,#14977,.T.);
#20149=ORIENTED_EDGE('',*,*,#14970,.T.);
#20150=ORIENTED_EDGE('',*,*,#14966,.T.);
#20151=ORIENTED_EDGE('',*,*,#14904,.F.);
#20152=ORIENTED_EDGE('',*,*,#14863,.T.);
#20153=ORIENTED_EDGE('',*,*,#14981,.T.);
#20154=ORIENTED_EDGE('',*,*,#14978,.T.);
#20155=ORIENTED_EDGE('',*,*,#14980,.F.);
#20156=ORIENTED_EDGE('',*,*,#14909,.T.);
#20157=ORIENTED_EDGE('',*,*,#14690,.F.);
#20158=ORIENTED_EDGE('',*,*,#14746,.T.);
#20159=ORIENTED_EDGE('',*,*,#14964,.F.);
#20160=ORIENTED_EDGE('',*,*,#14968,.F.);
#20161=ORIENTED_EDGE('',*,*,#14969,.T.);
#20162=ORIENTED_EDGE('',*,*,#14698,.F.);
#20163=ORIENTED_EDGE('',*,*,#14982,.T.);
#20164=ORIENTED_EDGE('',*,*,#14983,.T.);
#20165=ORIENTED_EDGE('',*,*,#14984,.T.);
#20166=ORIENTED_EDGE('',*,*,#14985,.T.);
#20167=ORIENTED_EDGE('',*,*,#14986,.T.);
#20168=ORIENTED_EDGE('',*,*,#14984,.F.);
#20169=ORIENTED_EDGE('',*,*,#14985,.F.);
#20170=ORIENTED_EDGE('',*,*,#14986,.F.);
#20171=ORIENTED_EDGE('',*,*,#14987,.T.);
#20172=ORIENTED_EDGE('',*,*,#14988,.F.);
#20173=ORIENTED_EDGE('',*,*,#14989,.F.);
#20174=ORIENTED_EDGE('',*,*,#14987,.F.);
#20175=ORIENTED_EDGE('',*,*,#14990,.F.);
#20176=ORIENTED_EDGE('',*,*,#14991,.T.);
#20177=ORIENTED_EDGE('',*,*,#14982,.F.);
#20178=ORIENTED_EDGE('',*,*,#14983,.F.);
#20179=ORIENTED_EDGE('',*,*,#14991,.F.);
#20180=ORIENTED_EDGE('',*,*,#14988,.T.);
#20181=ORIENTED_EDGE('',*,*,#14989,.T.);
#20182=ORIENTED_EDGE('',*,*,#14992,.T.);
#20183=ORIENTED_EDGE('',*,*,#14993,.T.);
#20184=ORIENTED_EDGE('',*,*,#14992,.F.);
#20185=ORIENTED_EDGE('',*,*,#14993,.F.);
#20186=ORIENTED_EDGE('',*,*,#14921,.T.);
#20187=ORIENTED_EDGE('',*,*,#14994,.T.);
#20188=ORIENTED_EDGE('',*,*,#14995,.T.);
#20189=ORIENTED_EDGE('',*,*,#14994,.F.);
#20190=ORIENTED_EDGE('',*,*,#14995,.F.);
#20191=ORIENTED_EDGE('',*,*,#14996,.T.);
#20192=ORIENTED_EDGE('',*,*,#14997,.F.);
#20193=ORIENTED_EDGE('',*,*,#14996,.F.);
#20194=ORIENTED_EDGE('',*,*,#14998,.T.);
#20195=ORIENTED_EDGE('',*,*,#14999,.T.);
#20196=ORIENTED_EDGE('',*,*,#14997,.T.);
#20197=ORIENTED_EDGE('',*,*,#14999,.F.);
#20198=ORIENTED_EDGE('',*,*,#14807,.F.);
#20199=ORIENTED_EDGE('',*,*,#14761,.F.);
#20200=ORIENTED_EDGE('',*,*,#14767,.F.);
#20201=ORIENTED_EDGE('',*,*,#14900,.F.);
#20202=ORIENTED_EDGE('',*,*,#15000,.F.);
#20203=ORIENTED_EDGE('',*,*,#14998,.F.);
#20204=ORIENTED_EDGE('',*,*,#14920,.T.);
#20205=ORIENTED_EDGE('',*,*,#15001,.T.);
#20206=ORIENTED_EDGE('',*,*,#15002,.T.);
#20207=ORIENTED_EDGE('',*,*,#15001,.F.);
#20208=ORIENTED_EDGE('',*,*,#15002,.F.);
#20209=ORIENTED_EDGE('',*,*,#15003,.T.);
#20210=ORIENTED_EDGE('',*,*,#15004,.F.);
#20211=ORIENTED_EDGE('',*,*,#15003,.F.);
#20212=ORIENTED_EDGE('',*,*,#15000,.T.);
#20213=ORIENTED_EDGE('',*,*,#15005,.T.);
#20214=ORIENTED_EDGE('',*,*,#15004,.T.);
#20215=ORIENTED_EDGE('',*,*,#15005,.F.);
#20216=ORIENTED_EDGE('',*,*,#15006,.F.);
#20217=ORIENTED_EDGE('',*,*,#15007,.T.);
#20218=ORIENTED_EDGE('',*,*,#14990,.T.);
#20219=ORIENTED_EDGE('',*,*,#15007,.F.);
#20220=ORIENTED_EDGE('',*,*,#14768,.F.);
#20221=ORIENTED_EDGE('',*,*,#14695,.T.);
#20222=ORIENTED_EDGE('',*,*,#14776,.F.);
#20223=ORIENTED_EDGE('',*,*,#14770,.F.);
#20224=ORIENTED_EDGE('',*,*,#14790,.F.);
#20225=ORIENTED_EDGE('',*,*,#14914,.T.);
#20226=ORIENTED_EDGE('',*,*,#14818,.F.);
#20227=ORIENTED_EDGE('',*,*,#14792,.F.);
#20228=ORIENTED_EDGE('',*,*,#14981,.F.);
#20229=ORIENTED_EDGE('',*,*,#14862,.F.);
#20230=ORIENTED_EDGE('',*,*,#14976,.F.);
#20231=ORIENTED_EDGE('',*,*,#14979,.F.);
#20232=ORIENTED_EDGE('',*,*,#15006,.T.);
#20233=ORIENTED_EDGE('',*,*,#14867,.F.);
#20234=ORIENTED_EDGE('',*,*,#14829,.F.);
#20235=ORIENTED_EDGE('',*,*,#14908,.F.);
#20236=ORIENTED_EDGE('',*,*,#14930,.T.);
#20237=ORIENTED_EDGE('',*,*,#14752,.F.);
#20238=ORIENTED_EDGE('',*,*,#15008,.F.);
#20239=ORIENTED_EDGE('',*,*,#14924,.F.);
#20240=ORIENTED_EDGE('',*,*,#14927,.T.);
#20241=ORIENTED_EDGE('',*,*,#14915,.F.);
#20242=ORIENTED_EDGE('',*,*,#14835,.F.);
#20243=ORIENTED_EDGE('',*,*,#14841,.F.);
#20244=ORIENTED_EDGE('',*,*,#14889,.F.);
#20245=ORIENTED_EDGE('',*,*,#14898,.F.);
#20246=ORIENTED_EDGE('',*,*,#14764,.F.);
#20247=ORIENTED_EDGE('',*,*,#14750,.F.);
#20248=ORIENTED_EDGE('',*,*,#14939,.F.);
#20249=ORIENTED_EDGE('',*,*,#14925,.F.);
#20250=ORIENTED_EDGE('',*,*,#15008,.T.);
#20251=ORIENTED_EDGE('',*,*,#15009,.T.);
#20252=ORIENTED_EDGE('',*,*,#15010,.T.);
#20253=ORIENTED_EDGE('',*,*,#15011,.T.);
#20254=ORIENTED_EDGE('',*,*,#15012,.T.);
#20255=ORIENTED_EDGE('',*,*,#15010,.F.);
#20256=ORIENTED_EDGE('',*,*,#15013,.F.);
#20257=ORIENTED_EDGE('',*,*,#15014,.F.);
#20258=ORIENTED_EDGE('',*,*,#15015,.F.);
#20259=ORIENTED_EDGE('',*,*,#15016,.T.);
#20260=ORIENTED_EDGE('',*,*,#15017,.T.);
#20261=ORIENTED_EDGE('',*,*,#15018,.T.);
#20262=ORIENTED_EDGE('',*,*,#15019,.T.);
#20263=ORIENTED_EDGE('',*,*,#15020,.T.);
#20264=ORIENTED_EDGE('',*,*,#15021,.T.);
#20265=ORIENTED_EDGE('',*,*,#15020,.F.);
#20266=ORIENTED_EDGE('',*,*,#15022,.F.);
#20267=ORIENTED_EDGE('',*,*,#15023,.F.);
#20268=ORIENTED_EDGE('',*,*,#15024,.F.);
#20269=ORIENTED_EDGE('',*,*,#15019,.F.);
#20270=ORIENTED_EDGE('',*,*,#15025,.F.);
#20271=ORIENTED_EDGE('',*,*,#15026,.T.);
#20272=ORIENTED_EDGE('',*,*,#15027,.F.);
#20273=ORIENTED_EDGE('',*,*,#15028,.F.);
#20274=ORIENTED_EDGE('',*,*,#15022,.T.);
#20275=ORIENTED_EDGE('',*,*,#15018,.F.);
#20276=ORIENTED_EDGE('',*,*,#15029,.T.);
#20277=ORIENTED_EDGE('',*,*,#15030,.F.);
#20278=ORIENTED_EDGE('',*,*,#15031,.F.);
#20279=ORIENTED_EDGE('',*,*,#15032,.T.);
#20280=ORIENTED_EDGE('',*,*,#15025,.T.);
#20281=ORIENTED_EDGE('',*,*,#15033,.T.);
#20282=ORIENTED_EDGE('',*,*,#15034,.T.);
#20283=ORIENTED_EDGE('',*,*,#15035,.T.);
#20284=ORIENTED_EDGE('',*,*,#15036,.T.);
#20285=ORIENTED_EDGE('',*,*,#15012,.F.);
#20286=ORIENTED_EDGE('',*,*,#15037,.F.);
#20287=ORIENTED_EDGE('',*,*,#15034,.F.);
#20288=ORIENTED_EDGE('',*,*,#15038,.F.);
#20289=ORIENTED_EDGE('',*,*,#15039,.T.);
#20290=ORIENTED_EDGE('',*,*,#15040,.T.);
#20291=ORIENTED_EDGE('',*,*,#15041,.T.);
#20292=ORIENTED_EDGE('',*,*,#15042,.T.);
#20293=ORIENTED_EDGE('',*,*,#15040,.F.);
#20294=ORIENTED_EDGE('',*,*,#15043,.F.);
#20295=ORIENTED_EDGE('',*,*,#15044,.F.);
#20296=ORIENTED_EDGE('',*,*,#15045,.F.);
#20297=ORIENTED_EDGE('',*,*,#15046,.T.);
#20298=ORIENTED_EDGE('',*,*,#15047,.T.);
#20299=ORIENTED_EDGE('',*,*,#15048,.T.);
#20300=ORIENTED_EDGE('',*,*,#15049,.T.);
#20301=ORIENTED_EDGE('',*,*,#15050,.T.);
#20302=ORIENTED_EDGE('',*,*,#15051,.T.);
#20303=ORIENTED_EDGE('',*,*,#15051,.F.);
#20304=ORIENTED_EDGE('',*,*,#15052,.T.);
#20305=ORIENTED_EDGE('',*,*,#15053,.F.);
#20306=ORIENTED_EDGE('',*,*,#15054,.F.);
#20307=ORIENTED_EDGE('',*,*,#15055,.T.);
#20308=ORIENTED_EDGE('',*,*,#15056,.F.);
#20309=ORIENTED_EDGE('',*,*,#15050,.F.);
#20310=ORIENTED_EDGE('',*,*,#15057,.F.);
#20311=ORIENTED_EDGE('',*,*,#15058,.F.);
#20312=ORIENTED_EDGE('',*,*,#15052,.F.);
#20313=ORIENTED_EDGE('',*,*,#15049,.F.);
#20314=ORIENTED_EDGE('',*,*,#15059,.F.);
#20315=ORIENTED_EDGE('',*,*,#15060,.T.);
#20316=ORIENTED_EDGE('',*,*,#15061,.F.);
#20317=ORIENTED_EDGE('',*,*,#15062,.F.);
#20318=ORIENTED_EDGE('',*,*,#15057,.T.);
#20319=ORIENTED_EDGE('',*,*,#15053,.T.);
#20320=ORIENTED_EDGE('',*,*,#15058,.T.);
#20321=ORIENTED_EDGE('',*,*,#15062,.T.);
#20322=ORIENTED_EDGE('',*,*,#15063,.T.);
#20323=ORIENTED_EDGE('',*,*,#15064,.T.);
#20324=ORIENTED_EDGE('',*,*,#15065,.T.);
#20325=ORIENTED_EDGE('',*,*,#15065,.F.);
#20326=ORIENTED_EDGE('',*,*,#15066,.T.);
#20327=ORIENTED_EDGE('',*,*,#15067,.T.);
#20328=ORIENTED_EDGE('',*,*,#15068,.T.);
#20329=ORIENTED_EDGE('',*,*,#15054,.T.);
#20330=ORIENTED_EDGE('',*,*,#15064,.F.);
#20331=ORIENTED_EDGE('',*,*,#15069,.F.);
#20332=ORIENTED_EDGE('',*,*,#15070,.F.);
#20333=ORIENTED_EDGE('',*,*,#15066,.F.);
#20334=ORIENTED_EDGE('',*,*,#15063,.F.);
#20335=ORIENTED_EDGE('',*,*,#15061,.T.);
#20336=ORIENTED_EDGE('',*,*,#15071,.T.);
#20337=ORIENTED_EDGE('',*,*,#15072,.T.);
#20338=ORIENTED_EDGE('',*,*,#15073,.F.);
#20339=ORIENTED_EDGE('',*,*,#15069,.T.);
#20340=ORIENTED_EDGE('',*,*,#15046,.F.);
#20341=ORIENTED_EDGE('',*,*,#15056,.T.);
#20342=ORIENTED_EDGE('',*,*,#15074,.T.);
#20343=ORIENTED_EDGE('',*,*,#15075,.T.);
#20344=ORIENTED_EDGE('',*,*,#15076,.T.);
#20345=ORIENTED_EDGE('',*,*,#15077,.T.);
#20346=ORIENTED_EDGE('',*,*,#15078,.T.);
#20347=ORIENTED_EDGE('',*,*,#15079,.T.);
#20348=ORIENTED_EDGE('',*,*,#15075,.F.);
#20349=ORIENTED_EDGE('',*,*,#15047,.F.);
#20350=ORIENTED_EDGE('',*,*,#15076,.F.);
#20351=ORIENTED_EDGE('',*,*,#15080,.F.);
#20352=ORIENTED_EDGE('',*,*,#15081,.F.);
#20353=ORIENTED_EDGE('',*,*,#15079,.F.);
#20354=ORIENTED_EDGE('',*,*,#15082,.F.);
#20355=ORIENTED_EDGE('',*,*,#15083,.F.);
#20356=ORIENTED_EDGE('',*,*,#15080,.T.);
#20357=ORIENTED_EDGE('',*,*,#15084,.T.);
#20358=ORIENTED_EDGE('',*,*,#15085,.T.);
#20359=ORIENTED_EDGE('',*,*,#15086,.T.);
#20360=ORIENTED_EDGE('',*,*,#15087,.T.);
#20361=ORIENTED_EDGE('',*,*,#15042,.F.);
#20362=ORIENTED_EDGE('',*,*,#15088,.F.);
#20363=ORIENTED_EDGE('',*,*,#15085,.F.);
#20364=ORIENTED_EDGE('',*,*,#15089,.F.);
#20365=ORIENTED_EDGE('',*,*,#15067,.F.);
#20366=ORIENTED_EDGE('',*,*,#15090,.F.);
#20367=ORIENTED_EDGE('',*,*,#15091,.F.);
#20368=ORIENTED_EDGE('',*,*,#15092,.T.);
#20369=ORIENTED_EDGE('',*,*,#15093,.T.);
#20370=ORIENTED_EDGE('',*,*,#15090,.T.);
#20371=ORIENTED_EDGE('',*,*,#15070,.T.);
#20372=ORIENTED_EDGE('',*,*,#15073,.T.);
#20373=ORIENTED_EDGE('',*,*,#15094,.F.);
#20374=ORIENTED_EDGE('',*,*,#15095,.F.);
#20375=ORIENTED_EDGE('',*,*,#15096,.F.);
#20376=ORIENTED_EDGE('',*,*,#15030,.T.);
#20377=ORIENTED_EDGE('',*,*,#15097,.T.);
#20378=ORIENTED_EDGE('',*,*,#15095,.T.);
#20379=ORIENTED_EDGE('',*,*,#15098,.T.);
#20380=ORIENTED_EDGE('',*,*,#15099,.T.);
#20381=ORIENTED_EDGE('',*,*,#15016,.F.);
#20382=ORIENTED_EDGE('',*,*,#15100,.T.);
#20383=ORIENTED_EDGE('',*,*,#15101,.T.);
#20384=ORIENTED_EDGE('',*,*,#15096,.T.);
#20385=ORIENTED_EDGE('',*,*,#15102,.T.);
#20386=ORIENTED_EDGE('',*,*,#15103,.T.);
#20387=ORIENTED_EDGE('',*,*,#15094,.T.);
#20388=ORIENTED_EDGE('',*,*,#15104,.T.);
#20389=ORIENTED_EDGE('',*,*,#15105,.T.);
#20390=ORIENTED_EDGE('',*,*,#15014,.T.);
#20391=ORIENTED_EDGE('',*,*,#15105,.F.);
#20392=ORIENTED_EDGE('',*,*,#15106,.T.);
#20393=ORIENTED_EDGE('',*,*,#15107,.T.);
#20394=ORIENTED_EDGE('',*,*,#15108,.T.);
#20395=ORIENTED_EDGE('',*,*,#15091,.T.);
#20396=ORIENTED_EDGE('',*,*,#15109,.T.);
#20397=ORIENTED_EDGE('',*,*,#15107,.F.);
#20398=ORIENTED_EDGE('',*,*,#15092,.F.);
#20399=ORIENTED_EDGE('',*,*,#15072,.F.);
#20400=ORIENTED_EDGE('',*,*,#15110,.T.);
#20401=ORIENTED_EDGE('',*,*,#15111,.T.);
#20402=ORIENTED_EDGE('',*,*,#15112,.T.);
#20403=ORIENTED_EDGE('',*,*,#15074,.F.);
#20404=ORIENTED_EDGE('',*,*,#15055,.F.);
#20405=ORIENTED_EDGE('',*,*,#15068,.F.);
#20406=ORIENTED_EDGE('',*,*,#15108,.F.);
#20407=ORIENTED_EDGE('',*,*,#15106,.F.);
#20408=ORIENTED_EDGE('',*,*,#15104,.F.);
#20409=ORIENTED_EDGE('',*,*,#15101,.F.);
#20410=ORIENTED_EDGE('',*,*,#15113,.F.);
#20411=ORIENTED_EDGE('',*,*,#15114,.F.);
#20412=ORIENTED_EDGE('',*,*,#15115,.F.);
#20413=ORIENTED_EDGE('',*,*,#15116,.F.);
#20414=ORIENTED_EDGE('',*,*,#15117,.F.);
#20415=ORIENTED_EDGE('',*,*,#15118,.F.);
#20416=ORIENTED_EDGE('',*,*,#15119,.F.);
#20417=ORIENTED_EDGE('',*,*,#15120,.F.);
#20418=ORIENTED_EDGE('',*,*,#15121,.F.);
#20419=ORIENTED_EDGE('',*,*,#15122,.F.);
#20420=ORIENTED_EDGE('',*,*,#15123,.F.);
#20421=ORIENTED_EDGE('',*,*,#15124,.F.);
#20422=ORIENTED_EDGE('',*,*,#15077,.F.);
#20423=ORIENTED_EDGE('',*,*,#15125,.T.);
#20424=ORIENTED_EDGE('',*,*,#15023,.T.);
#20425=ORIENTED_EDGE('',*,*,#15028,.T.);
#20426=ORIENTED_EDGE('',*,*,#15126,.T.);
#20427=ORIENTED_EDGE('',*,*,#15127,.T.);
#20428=ORIENTED_EDGE('',*,*,#15128,.T.);
#20429=ORIENTED_EDGE('',*,*,#15128,.F.);
#20430=ORIENTED_EDGE('',*,*,#15129,.T.);
#20431=ORIENTED_EDGE('',*,*,#15130,.F.);
#20432=ORIENTED_EDGE('',*,*,#15114,.T.);
#20433=ORIENTED_EDGE('',*,*,#15131,.T.);
#20434=ORIENTED_EDGE('',*,*,#15127,.F.);
#20435=ORIENTED_EDGE('',*,*,#15132,.F.);
#20436=ORIENTED_EDGE('',*,*,#15133,.T.);
#20437=ORIENTED_EDGE('',*,*,#15129,.F.);
#20438=ORIENTED_EDGE('',*,*,#15126,.F.);
#20439=ORIENTED_EDGE('',*,*,#15027,.T.);
#20440=ORIENTED_EDGE('',*,*,#15134,.T.);
#20441=ORIENTED_EDGE('',*,*,#15135,.T.);
#20442=ORIENTED_EDGE('',*,*,#15132,.T.);
#20443=ORIENTED_EDGE('',*,*,#15136,.T.);
#20444=ORIENTED_EDGE('',*,*,#15137,.T.);
#20445=ORIENTED_EDGE('',*,*,#15115,.T.);
#20446=ORIENTED_EDGE('',*,*,#15130,.T.);
#20447=ORIENTED_EDGE('',*,*,#15138,.T.);
#20448=ORIENTED_EDGE('',*,*,#15139,.T.);
#20449=ORIENTED_EDGE('',*,*,#15140,.T.);
#20450=ORIENTED_EDGE('',*,*,#15121,.T.);
#20451=ORIENTED_EDGE('',*,*,#15141,.T.);
#20452=ORIENTED_EDGE('',*,*,#15120,.T.);
#20453=ORIENTED_EDGE('',*,*,#15142,.T.);
#20454=ORIENTED_EDGE('',*,*,#15143,.T.);
#20455=ORIENTED_EDGE('',*,*,#15141,.F.);
#20456=ORIENTED_EDGE('',*,*,#15144,.F.);
#20457=ORIENTED_EDGE('',*,*,#15145,.F.);
#20458=ORIENTED_EDGE('',*,*,#15146,.F.);
#20459=ORIENTED_EDGE('',*,*,#15147,.T.);
#20460=ORIENTED_EDGE('',*,*,#15148,.T.);
#20461=ORIENTED_EDGE('',*,*,#15145,.T.);
#20462=ORIENTED_EDGE('',*,*,#15149,.T.);
#20463=ORIENTED_EDGE('',*,*,#15150,.T.);
#20464=ORIENTED_EDGE('',*,*,#15119,.T.);
#20465=ORIENTED_EDGE('',*,*,#15146,.T.);
#20466=ORIENTED_EDGE('',*,*,#15151,.T.);
#20467=ORIENTED_EDGE('',*,*,#15142,.F.);
#20468=ORIENTED_EDGE('',*,*,#15152,.T.);
#20469=ORIENTED_EDGE('',*,*,#15153,.T.);
#20470=ORIENTED_EDGE('',*,*,#15144,.T.);
#20471=ORIENTED_EDGE('',*,*,#15118,.T.);
#20472=ORIENTED_EDGE('',*,*,#15154,.T.);
#20473=ORIENTED_EDGE('',*,*,#15036,.F.);
#20474=ORIENTED_EDGE('',*,*,#15155,.F.);
#20475=ORIENTED_EDGE('',*,*,#15143,.F.);
#20476=ORIENTED_EDGE('',*,*,#15156,.F.);
#20477=ORIENTED_EDGE('',*,*,#15103,.F.);
#20478=ORIENTED_EDGE('',*,*,#15013,.T.);
#20479=ORIENTED_EDGE('',*,*,#15009,.F.);
#20480=ORIENTED_EDGE('',*,*,#15038,.T.);
#20481=ORIENTED_EDGE('',*,*,#15033,.F.);
#20482=ORIENTED_EDGE('',*,*,#15156,.T.);
#20483=ORIENTED_EDGE('',*,*,#15151,.F.);
#20484=ORIENTED_EDGE('',*,*,#15148,.F.);
#20485=ORIENTED_EDGE('',*,*,#15157,.F.);
#20486=ORIENTED_EDGE('',*,*,#15158,.T.);
#20487=ORIENTED_EDGE('',*,*,#15086,.F.);
#20488=ORIENTED_EDGE('',*,*,#15088,.T.);
#20489=ORIENTED_EDGE('',*,*,#15041,.F.);
#20490=ORIENTED_EDGE('',*,*,#15045,.T.);
#20491=ORIENTED_EDGE('',*,*,#15159,.F.);
#20492=ORIENTED_EDGE('',*,*,#15098,.F.);
#20493=ORIENTED_EDGE('',*,*,#15147,.F.);
#20494=ORIENTED_EDGE('',*,*,#15160,.F.);
#20495=ORIENTED_EDGE('',*,*,#15161,.T.);
#20496=ORIENTED_EDGE('',*,*,#15162,.T.);
#20497=ORIENTED_EDGE('',*,*,#15157,.T.);
#20498=ORIENTED_EDGE('',*,*,#15150,.F.);
#20499=ORIENTED_EDGE('',*,*,#15163,.T.);
#20500=ORIENTED_EDGE('',*,*,#15164,.F.);
#20501=ORIENTED_EDGE('',*,*,#15165,.T.);
#20502=ORIENTED_EDGE('',*,*,#15166,.T.);
#20503=ORIENTED_EDGE('',*,*,#15160,.T.);
#20504=ORIENTED_EDGE('',*,*,#15149,.F.);
#20505=ORIENTED_EDGE('',*,*,#15153,.F.);
#20506=ORIENTED_EDGE('',*,*,#15167,.F.);
#20507=ORIENTED_EDGE('',*,*,#15163,.F.);
#20508=ORIENTED_EDGE('',*,*,#15168,.F.);
#20509=ORIENTED_EDGE('',*,*,#15169,.F.);
#20510=ORIENTED_EDGE('',*,*,#15170,.F.);
#20511=ORIENTED_EDGE('',*,*,#15171,.F.);
#20512=ORIENTED_EDGE('',*,*,#15152,.F.);
#20513=ORIENTED_EDGE('',*,*,#15172,.T.);
#20514=ORIENTED_EDGE('',*,*,#15173,.T.);
#20515=ORIENTED_EDGE('',*,*,#15174,.T.);
#20516=ORIENTED_EDGE('',*,*,#15164,.T.);
#20517=ORIENTED_EDGE('',*,*,#15167,.T.);
#20518=ORIENTED_EDGE('',*,*,#15174,.F.);
#20519=ORIENTED_EDGE('',*,*,#15175,.T.);
#20520=ORIENTED_EDGE('',*,*,#15176,.F.);
#20521=ORIENTED_EDGE('',*,*,#15177,.F.);
#20522=ORIENTED_EDGE('',*,*,#15178,.T.);
#20523=ORIENTED_EDGE('',*,*,#15165,.F.);
#20524=ORIENTED_EDGE('',*,*,#15179,.T.);
#20525=ORIENTED_EDGE('',*,*,#15180,.T.);
#20526=ORIENTED_EDGE('',*,*,#15181,.T.);
#20527=ORIENTED_EDGE('',*,*,#15176,.T.);
#20528=ORIENTED_EDGE('',*,*,#15182,.T.);
#20529=ORIENTED_EDGE('',*,*,#15183,.T.);
#20530=ORIENTED_EDGE('',*,*,#15181,.F.);
#20531=ORIENTED_EDGE('',*,*,#15184,.T.);
#20532=ORIENTED_EDGE('',*,*,#15185,.F.);
#20533=ORIENTED_EDGE('',*,*,#15186,.T.);
#20534=ORIENTED_EDGE('',*,*,#15177,.T.);
#20535=ORIENTED_EDGE('',*,*,#15180,.F.);
#20536=ORIENTED_EDGE('',*,*,#15187,.F.);
#20537=ORIENTED_EDGE('',*,*,#15188,.F.);
#20538=ORIENTED_EDGE('',*,*,#15184,.F.);
#20539=ORIENTED_EDGE('',*,*,#15189,.F.);
#20540=ORIENTED_EDGE('',*,*,#15190,.F.);
#20541=ORIENTED_EDGE('',*,*,#15191,.F.);
#20542=ORIENTED_EDGE('',*,*,#15192,.F.);
#20543=ORIENTED_EDGE('',*,*,#15179,.F.);
#20544=ORIENTED_EDGE('',*,*,#15193,.T.);
#20545=ORIENTED_EDGE('',*,*,#15116,.T.);
#20546=ORIENTED_EDGE('',*,*,#15137,.F.);
#20547=ORIENTED_EDGE('',*,*,#15187,.T.);
#20548=ORIENTED_EDGE('',*,*,#15154,.F.);
#20549=ORIENTED_EDGE('',*,*,#15117,.T.);
#20550=ORIENTED_EDGE('',*,*,#15193,.F.);
#20551=ORIENTED_EDGE('',*,*,#15183,.F.);
#20552=ORIENTED_EDGE('',*,*,#15194,.T.);
#20553=ORIENTED_EDGE('',*,*,#15172,.F.);
#20554=ORIENTED_EDGE('',*,*,#15195,.T.);
#20555=ORIENTED_EDGE('',*,*,#15196,.T.);
#20556=ORIENTED_EDGE('',*,*,#15044,.T.);
#20557=ORIENTED_EDGE('',*,*,#15111,.F.);
#20558=ORIENTED_EDGE('',*,*,#15099,.F.);
#20559=ORIENTED_EDGE('',*,*,#15159,.T.);
#20560=ORIENTED_EDGE('',*,*,#15196,.F.);
#20561=ORIENTED_EDGE('',*,*,#15197,.T.);
#20562=ORIENTED_EDGE('',*,*,#15031,.T.);
#20563=ORIENTED_EDGE('',*,*,#15032,.F.);
#20564=ORIENTED_EDGE('',*,*,#15197,.F.);
#20565=ORIENTED_EDGE('',*,*,#15195,.F.);
#20566=ORIENTED_EDGE('',*,*,#15110,.F.);
#20567=ORIENTED_EDGE('',*,*,#15071,.F.);
#20568=ORIENTED_EDGE('',*,*,#15060,.F.);
#20569=ORIENTED_EDGE('',*,*,#15198,.F.);
#20570=ORIENTED_EDGE('',*,*,#15199,.F.);
#20571=ORIENTED_EDGE('',*,*,#15200,.F.);
#20572=ORIENTED_EDGE('',*,*,#15201,.F.);
#20573=ORIENTED_EDGE('',*,*,#15202,.F.);
#20574=ORIENTED_EDGE('',*,*,#15203,.F.);
#20575=ORIENTED_EDGE('',*,*,#15204,.F.);
#20576=ORIENTED_EDGE('',*,*,#15161,.F.);
#20577=ORIENTED_EDGE('',*,*,#15166,.F.);
#20578=ORIENTED_EDGE('',*,*,#15178,.F.);
#20579=ORIENTED_EDGE('',*,*,#15186,.F.);
#20580=ORIENTED_EDGE('',*,*,#15205,.F.);
#20581=ORIENTED_EDGE('',*,*,#15134,.F.);
#20582=ORIENTED_EDGE('',*,*,#15026,.F.);
#20583=ORIENTED_EDGE('',*,*,#15205,.T.);
#20584=ORIENTED_EDGE('',*,*,#15185,.T.);
#20585=ORIENTED_EDGE('',*,*,#15206,.T.);
#20586=ORIENTED_EDGE('',*,*,#15135,.F.);
#20587=ORIENTED_EDGE('',*,*,#15136,.F.);
#20588=ORIENTED_EDGE('',*,*,#15133,.F.);
#20589=ORIENTED_EDGE('',*,*,#15206,.F.);
#20590=ORIENTED_EDGE('',*,*,#15188,.T.);
#20591=ORIENTED_EDGE('',*,*,#15207,.F.);
#20592=ORIENTED_EDGE('',*,*,#15208,.F.);
#20593=ORIENTED_EDGE('',*,*,#15209,.F.);
#20594=ORIENTED_EDGE('',*,*,#15203,.T.);
#20595=ORIENTED_EDGE('',*,*,#15208,.T.);
#20596=ORIENTED_EDGE('',*,*,#15210,.T.);
#20597=ORIENTED_EDGE('',*,*,#15211,.T.);
#20598=ORIENTED_EDGE('',*,*,#15212,.T.);
#20599=ORIENTED_EDGE('',*,*,#15213,.T.);
#20600=ORIENTED_EDGE('',*,*,#15209,.T.);
#20601=ORIENTED_EDGE('',*,*,#15202,.T.);
#20602=ORIENTED_EDGE('',*,*,#15214,.T.);
#20603=ORIENTED_EDGE('',*,*,#15139,.F.);
#20604=ORIENTED_EDGE('',*,*,#15215,.T.);
#20605=ORIENTED_EDGE('',*,*,#15207,.T.);
#20606=ORIENTED_EDGE('',*,*,#15216,.T.);
#20607=ORIENTED_EDGE('',*,*,#15217,.T.);
#20608=ORIENTED_EDGE('',*,*,#15204,.T.);
#20609=ORIENTED_EDGE('',*,*,#15211,.F.);
#20610=ORIENTED_EDGE('',*,*,#15218,.T.);
#20611=ORIENTED_EDGE('',*,*,#15162,.F.);
#20612=ORIENTED_EDGE('',*,*,#15140,.F.);
#20613=ORIENTED_EDGE('',*,*,#15217,.F.);
#20614=ORIENTED_EDGE('',*,*,#15219,.T.);
#20615=ORIENTED_EDGE('',*,*,#15220,.T.);
#20616=ORIENTED_EDGE('',*,*,#15221,.T.);
#20617=ORIENTED_EDGE('',*,*,#15122,.T.);
#20618=ORIENTED_EDGE('',*,*,#15087,.F.);
#20619=ORIENTED_EDGE('',*,*,#15158,.F.);
#20620=ORIENTED_EDGE('',*,*,#15218,.F.);
#20621=ORIENTED_EDGE('',*,*,#15222,.F.);
#20622=ORIENTED_EDGE('',*,*,#15093,.F.);
#20623=ORIENTED_EDGE('',*,*,#15112,.F.);
#20624=ORIENTED_EDGE('',*,*,#15043,.T.);
#20625=ORIENTED_EDGE('',*,*,#15039,.F.);
#20626=ORIENTED_EDGE('',*,*,#15089,.T.);
#20627=ORIENTED_EDGE('',*,*,#15084,.F.);
#20628=ORIENTED_EDGE('',*,*,#15222,.T.);
#20629=ORIENTED_EDGE('',*,*,#15210,.F.);
#20630=ORIENTED_EDGE('',*,*,#15215,.F.);
#20631=ORIENTED_EDGE('',*,*,#15138,.F.);
#20632=ORIENTED_EDGE('',*,*,#15155,.T.);
#20633=ORIENTED_EDGE('',*,*,#15035,.F.);
#20634=ORIENTED_EDGE('',*,*,#15037,.T.);
#20635=ORIENTED_EDGE('',*,*,#15011,.F.);
#20636=ORIENTED_EDGE('',*,*,#15015,.T.);
#20637=ORIENTED_EDGE('',*,*,#15109,.F.);
#20638=ORIENTED_EDGE('',*,*,#15221,.F.);
#20639=ORIENTED_EDGE('',*,*,#15223,.F.);
#20640=ORIENTED_EDGE('',*,*,#15224,.T.);
#20641=ORIENTED_EDGE('',*,*,#15225,.F.);
#20642=ORIENTED_EDGE('',*,*,#15226,.F.);
#20643=ORIENTED_EDGE('',*,*,#15123,.T.);
#20644=ORIENTED_EDGE('',*,*,#15083,.T.);
#20645=ORIENTED_EDGE('',*,*,#15227,.T.);
#20646=ORIENTED_EDGE('',*,*,#15199,.T.);
#20647=ORIENTED_EDGE('',*,*,#15228,.T.);
#20648=ORIENTED_EDGE('',*,*,#15048,.F.);
#20649=ORIENTED_EDGE('',*,*,#15081,.T.);
#20650=ORIENTED_EDGE('',*,*,#15228,.F.);
#20651=ORIENTED_EDGE('',*,*,#15198,.T.);
#20652=ORIENTED_EDGE('',*,*,#15059,.T.);
#20653=ORIENTED_EDGE('',*,*,#15229,.T.);
#20654=ORIENTED_EDGE('',*,*,#15230,.T.);
#20655=ORIENTED_EDGE('',*,*,#15078,.F.);
#20656=ORIENTED_EDGE('',*,*,#15124,.T.);
#20657=ORIENTED_EDGE('',*,*,#15226,.T.);
#20658=ORIENTED_EDGE('',*,*,#15230,.F.);
#20659=ORIENTED_EDGE('',*,*,#15231,.F.);
#20660=ORIENTED_EDGE('',*,*,#15232,.F.);
#20661=ORIENTED_EDGE('',*,*,#15082,.T.);
#20662=ORIENTED_EDGE('',*,*,#15233,.F.);
#20663=ORIENTED_EDGE('',*,*,#15234,.F.);
#20664=ORIENTED_EDGE('',*,*,#15235,.F.);
#20665=ORIENTED_EDGE('',*,*,#15236,.F.);
#20666=ORIENTED_EDGE('',*,*,#15229,.F.);
#20667=ORIENTED_EDGE('',*,*,#15225,.T.);
#20668=ORIENTED_EDGE('',*,*,#15237,.T.);
#20669=ORIENTED_EDGE('',*,*,#15238,.T.);
#20670=ORIENTED_EDGE('',*,*,#15239,.F.);
#20671=ORIENTED_EDGE('',*,*,#15231,.T.);
#20672=ORIENTED_EDGE('',*,*,#15240,.T.);
#20673=ORIENTED_EDGE('',*,*,#15200,.T.);
#20674=ORIENTED_EDGE('',*,*,#15227,.F.);
#20675=ORIENTED_EDGE('',*,*,#15232,.T.);
#20676=ORIENTED_EDGE('',*,*,#15239,.T.);
#20677=ORIENTED_EDGE('',*,*,#15214,.F.);
#20678=ORIENTED_EDGE('',*,*,#15201,.T.);
#20679=ORIENTED_EDGE('',*,*,#15240,.F.);
#20680=ORIENTED_EDGE('',*,*,#15238,.F.);
#20681=ORIENTED_EDGE('',*,*,#15241,.T.);
#20682=ORIENTED_EDGE('',*,*,#15242,.F.);
#20683=ORIENTED_EDGE('',*,*,#15212,.F.);
#20684=ORIENTED_EDGE('',*,*,#15242,.T.);
#20685=ORIENTED_EDGE('',*,*,#15243,.T.);
#20686=ORIENTED_EDGE('',*,*,#15223,.T.);
#20687=ORIENTED_EDGE('',*,*,#15220,.F.);
#20688=ORIENTED_EDGE('',*,*,#15244,.T.);
#20689=ORIENTED_EDGE('',*,*,#15213,.F.);
#20690=ORIENTED_EDGE('',*,*,#15244,.F.);
#20691=ORIENTED_EDGE('',*,*,#15219,.F.);
#20692=ORIENTED_EDGE('',*,*,#15216,.F.);
#20693=ORIENTED_EDGE('',*,*,#15245,.F.);
#20694=ORIENTED_EDGE('',*,*,#15246,.F.);
#20695=ORIENTED_EDGE('',*,*,#15247,.F.);
#20696=ORIENTED_EDGE('',*,*,#15248,.F.);
#20697=ORIENTED_EDGE('',*,*,#15249,.T.);
#20698=ORIENTED_EDGE('',*,*,#15189,.T.);
#20699=ORIENTED_EDGE('',*,*,#15250,.T.);
#20700=ORIENTED_EDGE('',*,*,#15251,.T.);
#20701=ORIENTED_EDGE('',*,*,#15252,.T.);
#20702=ORIENTED_EDGE('',*,*,#15190,.T.);
#20703=ORIENTED_EDGE('',*,*,#15249,.F.);
#20704=ORIENTED_EDGE('',*,*,#15253,.T.);
#20705=ORIENTED_EDGE('',*,*,#15254,.T.);
#20706=ORIENTED_EDGE('',*,*,#15191,.T.);
#20707=ORIENTED_EDGE('',*,*,#15252,.F.);
#20708=ORIENTED_EDGE('',*,*,#15255,.T.);
#20709=ORIENTED_EDGE('',*,*,#15250,.F.);
#20710=ORIENTED_EDGE('',*,*,#15192,.T.);
#20711=ORIENTED_EDGE('',*,*,#15254,.F.);
#20712=ORIENTED_EDGE('',*,*,#15256,.T.);
#20713=ORIENTED_EDGE('',*,*,#15253,.F.);
#20714=ORIENTED_EDGE('',*,*,#15257,.F.);
#20715=ORIENTED_EDGE('',*,*,#15258,.F.);
#20716=ORIENTED_EDGE('',*,*,#15259,.T.);
#20717=ORIENTED_EDGE('',*,*,#15251,.F.);
#20718=ORIENTED_EDGE('',*,*,#15260,.F.);
#20719=ORIENTED_EDGE('',*,*,#15261,.F.);
#20720=ORIENTED_EDGE('',*,*,#15257,.T.);
#20721=ORIENTED_EDGE('',*,*,#15262,.T.);
#20722=ORIENTED_EDGE('',*,*,#15168,.T.);
#20723=ORIENTED_EDGE('',*,*,#15263,.T.);
#20724=ORIENTED_EDGE('',*,*,#15261,.T.);
#20725=ORIENTED_EDGE('',*,*,#15264,.T.);
#20726=ORIENTED_EDGE('',*,*,#15169,.T.);
#20727=ORIENTED_EDGE('',*,*,#15262,.F.);
#20728=ORIENTED_EDGE('',*,*,#15265,.T.);
#20729=ORIENTED_EDGE('',*,*,#15266,.T.);
#20730=ORIENTED_EDGE('',*,*,#15170,.T.);
#20731=ORIENTED_EDGE('',*,*,#15264,.F.);
#20732=ORIENTED_EDGE('',*,*,#15267,.T.);
#20733=ORIENTED_EDGE('',*,*,#15263,.F.);
#20734=ORIENTED_EDGE('',*,*,#15171,.T.);
#20735=ORIENTED_EDGE('',*,*,#15266,.F.);
#20736=ORIENTED_EDGE('',*,*,#15258,.T.);
#20737=ORIENTED_EDGE('',*,*,#15256,.F.);
#20738=ORIENTED_EDGE('',*,*,#15268,.F.);
#20739=ORIENTED_EDGE('',*,*,#15265,.F.);
#20740=ORIENTED_EDGE('',*,*,#15260,.T.);
#20741=ORIENTED_EDGE('',*,*,#15269,.T.);
#20742=ORIENTED_EDGE('',*,*,#15233,.T.);
#20743=ORIENTED_EDGE('',*,*,#15270,.T.);
#20744=ORIENTED_EDGE('',*,*,#15271,.T.);
#20745=ORIENTED_EDGE('',*,*,#15272,.T.);
#20746=ORIENTED_EDGE('',*,*,#15234,.T.);
#20747=ORIENTED_EDGE('',*,*,#15269,.F.);
#20748=ORIENTED_EDGE('',*,*,#15273,.T.);
#20749=ORIENTED_EDGE('',*,*,#15274,.T.);
#20750=ORIENTED_EDGE('',*,*,#15235,.T.);
#20751=ORIENTED_EDGE('',*,*,#15272,.F.);
#20752=ORIENTED_EDGE('',*,*,#15275,.T.);
#20753=ORIENTED_EDGE('',*,*,#15270,.F.);
#20754=ORIENTED_EDGE('',*,*,#15236,.T.);
#20755=ORIENTED_EDGE('',*,*,#15274,.F.);
#20756=ORIENTED_EDGE('',*,*,#15276,.T.);
#20757=ORIENTED_EDGE('',*,*,#15273,.F.);
#20758=ORIENTED_EDGE('',*,*,#15277,.F.);
#20759=ORIENTED_EDGE('',*,*,#15278,.F.);
#20760=ORIENTED_EDGE('',*,*,#15279,.T.);
#20761=ORIENTED_EDGE('',*,*,#15271,.F.);
#20762=ORIENTED_EDGE('',*,*,#15280,.F.);
#20763=ORIENTED_EDGE('',*,*,#15281,.F.);
#20764=ORIENTED_EDGE('',*,*,#15277,.T.);
#20765=ORIENTED_EDGE('',*,*,#15282,.T.);
#20766=ORIENTED_EDGE('',*,*,#15245,.T.);
#20767=ORIENTED_EDGE('',*,*,#15283,.T.);
#20768=ORIENTED_EDGE('',*,*,#15281,.T.);
#20769=ORIENTED_EDGE('',*,*,#15284,.T.);
#20770=ORIENTED_EDGE('',*,*,#15246,.T.);
#20771=ORIENTED_EDGE('',*,*,#15282,.F.);
#20772=ORIENTED_EDGE('',*,*,#15285,.T.);
#20773=ORIENTED_EDGE('',*,*,#15286,.T.);
#20774=ORIENTED_EDGE('',*,*,#15247,.T.);
#20775=ORIENTED_EDGE('',*,*,#15284,.F.);
#20776=ORIENTED_EDGE('',*,*,#15287,.T.);
#20777=ORIENTED_EDGE('',*,*,#15283,.F.);
#20778=ORIENTED_EDGE('',*,*,#15248,.T.);
#20779=ORIENTED_EDGE('',*,*,#15286,.F.);
#20780=ORIENTED_EDGE('',*,*,#15278,.T.);
#20781=ORIENTED_EDGE('',*,*,#15276,.F.);
#20782=ORIENTED_EDGE('',*,*,#15288,.F.);
#20783=ORIENTED_EDGE('',*,*,#15285,.F.);
#20784=ORIENTED_EDGE('',*,*,#15280,.T.);
#20785=ORIENTED_EDGE('',*,*,#15275,.F.);
#20786=ORIENTED_EDGE('',*,*,#15279,.F.);
#20787=ORIENTED_EDGE('',*,*,#15287,.F.);
#20788=ORIENTED_EDGE('',*,*,#15288,.T.);
#20789=ORIENTED_EDGE('',*,*,#15255,.F.);
#20790=ORIENTED_EDGE('',*,*,#15259,.F.);
#20791=ORIENTED_EDGE('',*,*,#15267,.F.);
#20792=ORIENTED_EDGE('',*,*,#15268,.T.);
#20793=ORIENTED_EDGE('',*,*,#15243,.F.);
#20794=ORIENTED_EDGE('',*,*,#15241,.F.);
#20795=ORIENTED_EDGE('',*,*,#15237,.F.);
#20796=ORIENTED_EDGE('',*,*,#15224,.F.);
#20797=ORIENTED_EDGE('',*,*,#15021,.F.);
#20798=ORIENTED_EDGE('',*,*,#15024,.T.);
#20799=ORIENTED_EDGE('',*,*,#15125,.F.);
#20800=ORIENTED_EDGE('',*,*,#15131,.F.);
#20801=ORIENTED_EDGE('',*,*,#15113,.T.);
#20802=ORIENTED_EDGE('',*,*,#15100,.F.);
#20803=ORIENTED_EDGE('',*,*,#15173,.F.);
#20804=ORIENTED_EDGE('',*,*,#15194,.F.);
#20805=ORIENTED_EDGE('',*,*,#15182,.F.);
#20806=ORIENTED_EDGE('',*,*,#15175,.F.);
#20807=ORIENTED_EDGE('',*,*,#15017,.F.);
#20808=ORIENTED_EDGE('',*,*,#15102,.F.);
#20809=ORIENTED_EDGE('',*,*,#15097,.F.);
#20810=ORIENTED_EDGE('',*,*,#15029,.F.);
#20811=ORIENTED_EDGE('',*,*,#15289,.T.);
#20812=ORIENTED_EDGE('',*,*,#15290,.T.);
#20813=ORIENTED_EDGE('',*,*,#15291,.T.);
#20814=ORIENTED_EDGE('',*,*,#15292,.T.);
#20815=ORIENTED_EDGE('',*,*,#15293,.T.);
#20816=ORIENTED_EDGE('',*,*,#15294,.T.);
#20817=ORIENTED_EDGE('',*,*,#15291,.F.);
#20818=ORIENTED_EDGE('',*,*,#15295,.T.);
#20819=ORIENTED_EDGE('',*,*,#15296,.F.);
#20820=ORIENTED_EDGE('',*,*,#15297,.T.);
#20821=ORIENTED_EDGE('',*,*,#15298,.T.);
#20822=ORIENTED_EDGE('',*,*,#15299,.T.);
#20823=ORIENTED_EDGE('',*,*,#15290,.F.);
#20824=ORIENTED_EDGE('',*,*,#15300,.F.);
#20825=ORIENTED_EDGE('',*,*,#15301,.F.);
#20826=ORIENTED_EDGE('',*,*,#15295,.F.);
#20827=ORIENTED_EDGE('',*,*,#15289,.F.);
#20828=ORIENTED_EDGE('',*,*,#15302,.F.);
#20829=ORIENTED_EDGE('',*,*,#15303,.T.);
#20830=ORIENTED_EDGE('',*,*,#15304,.T.);
#20831=ORIENTED_EDGE('',*,*,#15305,.F.);
#20832=ORIENTED_EDGE('',*,*,#15300,.T.);
#20833=ORIENTED_EDGE('',*,*,#15306,.T.);
#20834=ORIENTED_EDGE('',*,*,#15307,.T.);
#20835=ORIENTED_EDGE('',*,*,#15308,.T.);
#20836=ORIENTED_EDGE('',*,*,#15296,.T.);
#20837=ORIENTED_EDGE('',*,*,#15301,.T.);
#20838=ORIENTED_EDGE('',*,*,#15305,.T.);
#20839=ORIENTED_EDGE('',*,*,#15309,.T.);
#20840=ORIENTED_EDGE('',*,*,#15310,.T.);
#20841=ORIENTED_EDGE('',*,*,#15311,.T.);
#20842=ORIENTED_EDGE('',*,*,#15312,.T.);
#20843=ORIENTED_EDGE('',*,*,#15313,.T.);
#20844=ORIENTED_EDGE('',*,*,#15314,.T.);
#20845=ORIENTED_EDGE('',*,*,#15312,.F.);
#20846=ORIENTED_EDGE('',*,*,#15315,.F.);
#20847=ORIENTED_EDGE('',*,*,#15316,.T.);
#20848=ORIENTED_EDGE('',*,*,#15317,.T.);
#20849=ORIENTED_EDGE('',*,*,#15318,.F.);
#20850=ORIENTED_EDGE('',*,*,#15319,.T.);
#20851=ORIENTED_EDGE('',*,*,#15311,.F.);
#20852=ORIENTED_EDGE('',*,*,#15320,.T.);
#20853=ORIENTED_EDGE('',*,*,#15321,.F.);
#20854=ORIENTED_EDGE('',*,*,#15322,.T.);
#20855=ORIENTED_EDGE('',*,*,#15315,.T.);
#20856=ORIENTED_EDGE('',*,*,#15310,.F.);
#20857=ORIENTED_EDGE('',*,*,#15323,.F.);
#20858=ORIENTED_EDGE('',*,*,#15324,.F.);
#20859=ORIENTED_EDGE('',*,*,#15320,.F.);
#20860=ORIENTED_EDGE('',*,*,#15325,.F.);
#20861=ORIENTED_EDGE('',*,*,#15326,.F.);
#20862=ORIENTED_EDGE('',*,*,#15327,.T.);
#20863=ORIENTED_EDGE('',*,*,#15328,.T.);
#20864=ORIENTED_EDGE('',*,*,#15329,.T.);
#20865=ORIENTED_EDGE('',*,*,#15330,.T.);
#20866=ORIENTED_EDGE('',*,*,#15331,.T.);
#20867=ORIENTED_EDGE('',*,*,#15332,.T.);
#20868=ORIENTED_EDGE('',*,*,#15329,.F.);
#20869=ORIENTED_EDGE('',*,*,#15333,.T.);
#20870=ORIENTED_EDGE('',*,*,#15334,.F.);
#20871=ORIENTED_EDGE('',*,*,#15317,.F.);
#20872=ORIENTED_EDGE('',*,*,#15335,.T.);
#20873=ORIENTED_EDGE('',*,*,#15336,.T.);
#20874=ORIENTED_EDGE('',*,*,#15328,.F.);
#20875=ORIENTED_EDGE('',*,*,#15337,.F.);
#20876=ORIENTED_EDGE('',*,*,#15338,.F.);
#20877=ORIENTED_EDGE('',*,*,#15333,.F.);
#20878=ORIENTED_EDGE('',*,*,#15339,.F.);
#20879=ORIENTED_EDGE('',*,*,#15340,.F.);
#20880=ORIENTED_EDGE('',*,*,#15327,.F.);
#20881=ORIENTED_EDGE('',*,*,#15341,.F.);
#20882=ORIENTED_EDGE('',*,*,#15342,.T.);
#20883=ORIENTED_EDGE('',*,*,#15343,.T.);
#20884=ORIENTED_EDGE('',*,*,#15344,.F.);
#20885=ORIENTED_EDGE('',*,*,#15337,.T.);
#20886=ORIENTED_EDGE('',*,*,#15345,.T.);
#20887=ORIENTED_EDGE('',*,*,#15346,.T.);
#20888=ORIENTED_EDGE('',*,*,#15318,.T.);
#20889=ORIENTED_EDGE('',*,*,#15334,.T.);
#20890=ORIENTED_EDGE('',*,*,#15338,.T.);
#20891=ORIENTED_EDGE('',*,*,#15344,.T.);
#20892=ORIENTED_EDGE('',*,*,#15314,.F.);
#20893=ORIENTED_EDGE('',*,*,#15347,.T.);
#20894=ORIENTED_EDGE('',*,*,#15345,.F.);
#20895=ORIENTED_EDGE('',*,*,#15343,.F.);
#20896=ORIENTED_EDGE('',*,*,#15348,.T.);
#20897=ORIENTED_EDGE('',*,*,#15349,.T.);
#20898=ORIENTED_EDGE('',*,*,#15325,.T.);
#20899=ORIENTED_EDGE('',*,*,#15350,.T.);
#20900=ORIENTED_EDGE('',*,*,#15351,.T.);
#20901=ORIENTED_EDGE('',*,*,#15350,.F.);
#20902=ORIENTED_EDGE('',*,*,#15352,.F.);
#20903=ORIENTED_EDGE('',*,*,#15353,.T.);
#20904=ORIENTED_EDGE('',*,*,#15351,.F.);
#20905=ORIENTED_EDGE('',*,*,#15353,.F.);
#20906=ORIENTED_EDGE('',*,*,#15340,.T.);
#20907=ORIENTED_EDGE('',*,*,#15354,.T.);
#20908=ORIENTED_EDGE('',*,*,#15352,.T.);
#20909=ORIENTED_EDGE('',*,*,#15354,.F.);
#20910=ORIENTED_EDGE('',*,*,#15326,.T.);
#20911=ORIENTED_EDGE('',*,*,#15355,.T.);
#20912=ORIENTED_EDGE('',*,*,#15356,.T.);
#20913=ORIENTED_EDGE('',*,*,#15355,.F.);
#20914=ORIENTED_EDGE('',*,*,#15357,.F.);
#20915=ORIENTED_EDGE('',*,*,#15358,.T.);
#20916=ORIENTED_EDGE('',*,*,#15356,.F.);
#20917=ORIENTED_EDGE('',*,*,#15358,.F.);
#20918=ORIENTED_EDGE('',*,*,#15339,.T.);
#20919=ORIENTED_EDGE('',*,*,#15359,.T.);
#20920=ORIENTED_EDGE('',*,*,#15357,.T.);
#20921=ORIENTED_EDGE('',*,*,#15359,.F.);
#20922=ORIENTED_EDGE('',*,*,#15309,.F.);
#20923=ORIENTED_EDGE('',*,*,#15349,.F.);
#20924=ORIENTED_EDGE('',*,*,#15360,.T.);
#20925=ORIENTED_EDGE('',*,*,#15361,.T.);
#20926=ORIENTED_EDGE('',*,*,#15323,.T.);
#20927=ORIENTED_EDGE('',*,*,#15294,.F.);
#20928=ORIENTED_EDGE('',*,*,#15362,.T.);
#20929=ORIENTED_EDGE('',*,*,#15361,.F.);
#20930=ORIENTED_EDGE('',*,*,#15363,.T.);
#20931=ORIENTED_EDGE('',*,*,#15302,.T.);
#20932=ORIENTED_EDGE('',*,*,#15306,.F.);
#20933=ORIENTED_EDGE('',*,*,#15304,.F.);
#20934=ORIENTED_EDGE('',*,*,#15364,.T.);
#20935=ORIENTED_EDGE('',*,*,#15341,.T.);
#20936=ORIENTED_EDGE('',*,*,#15332,.F.);
#20937=ORIENTED_EDGE('',*,*,#15365,.T.);
#20938=ORIENTED_EDGE('',*,*,#15313,.F.);
#20939=ORIENTED_EDGE('',*,*,#15319,.F.);
#20940=ORIENTED_EDGE('',*,*,#15346,.F.);
#20941=ORIENTED_EDGE('',*,*,#15347,.F.);
#20942=ORIENTED_EDGE('',*,*,#15360,.F.);
#20943=ORIENTED_EDGE('',*,*,#15348,.F.);
#20944=ORIENTED_EDGE('',*,*,#15342,.F.);
#20945=ORIENTED_EDGE('',*,*,#15364,.F.);
#20946=ORIENTED_EDGE('',*,*,#15303,.F.);
#20947=ORIENTED_EDGE('',*,*,#15363,.F.);
#20948=ORIENTED_EDGE('',*,*,#15308,.F.);
#20949=ORIENTED_EDGE('',*,*,#15366,.T.);
#20950=ORIENTED_EDGE('',*,*,#15330,.F.);
#20951=ORIENTED_EDGE('',*,*,#15336,.F.);
#20952=ORIENTED_EDGE('',*,*,#15367,.T.);
#20953=ORIENTED_EDGE('',*,*,#15297,.F.);
#20954=ORIENTED_EDGE('',*,*,#15292,.F.);
#20955=ORIENTED_EDGE('',*,*,#15299,.F.);
#20956=ORIENTED_EDGE('',*,*,#15368,.T.);
#20957=ORIENTED_EDGE('',*,*,#15321,.T.);
#20958=ORIENTED_EDGE('',*,*,#15369,.T.);
#20959=ORIENTED_EDGE('',*,*,#15307,.F.);
#20960=ORIENTED_EDGE('',*,*,#15365,.F.);
#20961=ORIENTED_EDGE('',*,*,#15331,.F.);
#20962=ORIENTED_EDGE('',*,*,#15366,.F.);
#20963=ORIENTED_EDGE('',*,*,#15298,.F.);
#20964=ORIENTED_EDGE('',*,*,#15367,.F.);
#20965=ORIENTED_EDGE('',*,*,#15335,.F.);
#20966=ORIENTED_EDGE('',*,*,#15316,.F.);
#20967=ORIENTED_EDGE('',*,*,#15322,.F.);
#20968=ORIENTED_EDGE('',*,*,#15368,.F.);
#20969=ORIENTED_EDGE('',*,*,#15293,.F.);
#20970=ORIENTED_EDGE('',*,*,#15369,.F.);
#20971=ORIENTED_EDGE('',*,*,#15324,.T.);
#20972=ORIENTED_EDGE('',*,*,#15362,.F.);
#20973=ORIENTED_EDGE('',*,*,#15370,.T.);
#20974=ORIENTED_EDGE('',*,*,#15371,.T.);
#20975=ORIENTED_EDGE('',*,*,#15372,.T.);
#20976=ORIENTED_EDGE('',*,*,#15373,.T.);
#20977=ORIENTED_EDGE('',*,*,#15374,.T.);
#20978=ORIENTED_EDGE('',*,*,#15375,.T.);
#20979=ORIENTED_EDGE('',*,*,#15370,.F.);
#20980=ORIENTED_EDGE('',*,*,#15376,.T.);
#20981=ORIENTED_EDGE('',*,*,#15377,.T.);
#20982=ORIENTED_EDGE('',*,*,#15378,.T.);
#20983=ORIENTED_EDGE('',*,*,#15374,.F.);
#20984=ORIENTED_EDGE('',*,*,#15379,.T.);
#20985=ORIENTED_EDGE('',*,*,#15380,.T.);
#20986=ORIENTED_EDGE('',*,*,#15381,.T.);
#20987=ORIENTED_EDGE('',*,*,#15377,.F.);
#20988=ORIENTED_EDGE('',*,*,#15382,.T.);
#20989=ORIENTED_EDGE('',*,*,#15383,.T.);
#20990=ORIENTED_EDGE('',*,*,#15384,.T.);
#20991=ORIENTED_EDGE('',*,*,#15380,.F.);
#20992=ORIENTED_EDGE('',*,*,#15385,.T.);
#20993=ORIENTED_EDGE('',*,*,#15386,.T.);
#20994=ORIENTED_EDGE('',*,*,#15387,.T.);
#20995=ORIENTED_EDGE('',*,*,#15383,.F.);
#20996=ORIENTED_EDGE('',*,*,#15388,.T.);
#20997=ORIENTED_EDGE('',*,*,#15389,.T.);
#20998=ORIENTED_EDGE('',*,*,#15390,.T.);
#20999=ORIENTED_EDGE('',*,*,#15386,.F.);
#21000=ORIENTED_EDGE('',*,*,#15391,.T.);
#21001=ORIENTED_EDGE('',*,*,#15372,.F.);
#21002=ORIENTED_EDGE('',*,*,#15392,.T.);
#21003=ORIENTED_EDGE('',*,*,#15389,.F.);
#21004=ORIENTED_EDGE('',*,*,#15393,.T.);
#21005=ORIENTED_EDGE('',*,*,#15387,.F.);
#21006=ORIENTED_EDGE('',*,*,#15394,.T.);
#21007=ORIENTED_EDGE('',*,*,#15395,.F.);
#21008=ORIENTED_EDGE('',*,*,#15396,.F.);
#21009=ORIENTED_EDGE('',*,*,#15390,.F.);
#21010=ORIENTED_EDGE('',*,*,#15397,.T.);
#21011=ORIENTED_EDGE('',*,*,#15398,.F.);
#21012=ORIENTED_EDGE('',*,*,#15394,.F.);
#21013=ORIENTED_EDGE('',*,*,#15392,.F.);
#21014=ORIENTED_EDGE('',*,*,#15399,.F.);
#21015=ORIENTED_EDGE('',*,*,#15400,.F.);
#21016=ORIENTED_EDGE('',*,*,#15397,.F.);
#21017=ORIENTED_EDGE('',*,*,#15371,.F.);
#21018=ORIENTED_EDGE('',*,*,#15401,.T.);
#21019=ORIENTED_EDGE('',*,*,#15402,.F.);
#21020=ORIENTED_EDGE('',*,*,#15399,.T.);
#21021=ORIENTED_EDGE('',*,*,#15373,.F.);
#21022=ORIENTED_EDGE('',*,*,#15393,.F.);
#21023=ORIENTED_EDGE('',*,*,#15391,.F.);
#21024=ORIENTED_EDGE('',*,*,#15388,.F.);
#21025=ORIENTED_EDGE('',*,*,#15385,.F.);
#21026=ORIENTED_EDGE('',*,*,#15382,.F.);
#21027=ORIENTED_EDGE('',*,*,#15379,.F.);
#21028=ORIENTED_EDGE('',*,*,#15376,.F.);
#21029=ORIENTED_EDGE('',*,*,#15403,.F.);
#21030=ORIENTED_EDGE('',*,*,#15404,.T.);
#21031=ORIENTED_EDGE('',*,*,#15405,.T.);
#21032=ORIENTED_EDGE('',*,*,#15406,.T.);
#21033=ORIENTED_EDGE('',*,*,#15407,.T.);
#21034=ORIENTED_EDGE('',*,*,#15408,.T.);
#21035=ORIENTED_EDGE('',*,*,#15409,.T.);
#21036=ORIENTED_EDGE('',*,*,#15407,.F.);
#21037=ORIENTED_EDGE('',*,*,#15410,.T.);
#21038=ORIENTED_EDGE('',*,*,#15411,.F.);
#21039=ORIENTED_EDGE('',*,*,#15412,.F.);
#21040=ORIENTED_EDGE('',*,*,#15413,.T.);
#21041=ORIENTED_EDGE('',*,*,#15411,.T.);
#21042=ORIENTED_EDGE('',*,*,#15414,.T.);
#21043=ORIENTED_EDGE('',*,*,#15415,.T.);
#21044=ORIENTED_EDGE('',*,*,#15416,.T.);
#21045=ORIENTED_EDGE('',*,*,#15400,.T.);
#21046=ORIENTED_EDGE('',*,*,#15417,.T.);
#21047=ORIENTED_EDGE('',*,*,#15418,.T.);
#21048=ORIENTED_EDGE('',*,*,#15419,.T.);
#21049=ORIENTED_EDGE('',*,*,#15398,.T.);
#21050=ORIENTED_EDGE('',*,*,#15416,.F.);
#21051=ORIENTED_EDGE('',*,*,#15420,.T.);
#21052=ORIENTED_EDGE('',*,*,#15421,.T.);
#21053=ORIENTED_EDGE('',*,*,#15395,.T.);
#21054=ORIENTED_EDGE('',*,*,#15419,.F.);
#21055=ORIENTED_EDGE('',*,*,#15422,.T.);
#21056=ORIENTED_EDGE('',*,*,#15423,.T.);
#21057=ORIENTED_EDGE('',*,*,#15424,.T.);
#21058=ORIENTED_EDGE('',*,*,#15421,.F.);
#21059=ORIENTED_EDGE('',*,*,#15425,.T.);
#21060=ORIENTED_EDGE('',*,*,#15426,.T.);
#21061=ORIENTED_EDGE('',*,*,#15427,.T.);
#21062=ORIENTED_EDGE('',*,*,#15423,.F.);
#21063=ORIENTED_EDGE('',*,*,#15428,.T.);
#21064=ORIENTED_EDGE('',*,*,#15429,.T.);
#21065=ORIENTED_EDGE('',*,*,#15430,.T.);
#21066=ORIENTED_EDGE('',*,*,#15426,.F.);
#21067=ORIENTED_EDGE('',*,*,#15431,.T.);
#21068=ORIENTED_EDGE('',*,*,#15432,.T.);
#21069=ORIENTED_EDGE('',*,*,#15433,.T.);
#21070=ORIENTED_EDGE('',*,*,#15429,.F.);
#21071=ORIENTED_EDGE('',*,*,#15434,.T.);
#21072=ORIENTED_EDGE('',*,*,#15417,.F.);
#21073=ORIENTED_EDGE('',*,*,#15402,.T.);
#21074=ORIENTED_EDGE('',*,*,#15432,.F.);
#21075=ORIENTED_EDGE('',*,*,#15435,.T.);
#21076=ORIENTED_EDGE('',*,*,#15425,.F.);
#21077=ORIENTED_EDGE('',*,*,#15436,.T.);
#21078=ORIENTED_EDGE('',*,*,#15437,.F.);
#21079=ORIENTED_EDGE('',*,*,#15438,.T.);
#21080=ORIENTED_EDGE('',*,*,#15422,.F.);
#21081=ORIENTED_EDGE('',*,*,#15439,.F.);
#21082=ORIENTED_EDGE('',*,*,#15440,.F.);
#21083=ORIENTED_EDGE('',*,*,#15436,.F.);
#21084=ORIENTED_EDGE('',*,*,#15420,.F.);
#21085=ORIENTED_EDGE('',*,*,#15441,.T.);
#21086=ORIENTED_EDGE('',*,*,#15442,.F.);
#21087=ORIENTED_EDGE('',*,*,#15439,.T.);
#21088=ORIENTED_EDGE('',*,*,#15418,.F.);
#21089=ORIENTED_EDGE('',*,*,#15443,.F.);
#21090=ORIENTED_EDGE('',*,*,#15444,.F.);
#21091=ORIENTED_EDGE('',*,*,#15441,.F.);
#21092=ORIENTED_EDGE('',*,*,#15445,.F.);
#21093=ORIENTED_EDGE('',*,*,#15378,.F.);
#21094=ORIENTED_EDGE('',*,*,#15446,.T.);
#21095=ORIENTED_EDGE('',*,*,#15430,.F.);
#21096=ORIENTED_EDGE('',*,*,#15447,.F.);
#21097=ORIENTED_EDGE('',*,*,#15375,.F.);
#21098=ORIENTED_EDGE('',*,*,#15447,.T.);
#21099=ORIENTED_EDGE('',*,*,#15433,.F.);
#21100=ORIENTED_EDGE('',*,*,#15401,.F.);
#21101=ORIENTED_EDGE('',*,*,#15448,.T.);
#21102=ORIENTED_EDGE('',*,*,#15449,.T.);
#21103=ORIENTED_EDGE('',*,*,#15450,.T.);
#21104=ORIENTED_EDGE('',*,*,#15451,.T.);
#21105=ORIENTED_EDGE('',*,*,#15452,.T.);
#21106=ORIENTED_EDGE('',*,*,#15453,.T.);
#21107=ORIENTED_EDGE('',*,*,#15450,.F.);
#21108=ORIENTED_EDGE('',*,*,#15454,.T.);
#21109=ORIENTED_EDGE('',*,*,#15455,.T.);
#21110=ORIENTED_EDGE('',*,*,#15456,.T.);
#21111=ORIENTED_EDGE('',*,*,#15452,.F.);
#21112=ORIENTED_EDGE('',*,*,#15457,.T.);
#21113=ORIENTED_EDGE('',*,*,#15458,.T.);
#21114=ORIENTED_EDGE('',*,*,#15459,.T.);
#21115=ORIENTED_EDGE('',*,*,#15455,.F.);
#21116=ORIENTED_EDGE('',*,*,#15460,.T.);
#21117=ORIENTED_EDGE('',*,*,#15461,.T.);
#21118=ORIENTED_EDGE('',*,*,#15462,.T.);
#21119=ORIENTED_EDGE('',*,*,#15458,.F.);
#21120=ORIENTED_EDGE('',*,*,#15463,.T.);
#21121=ORIENTED_EDGE('',*,*,#15461,.F.);
#21122=ORIENTED_EDGE('',*,*,#15464,.F.);
#21123=ORIENTED_EDGE('',*,*,#15465,.F.);
#21124=ORIENTED_EDGE('',*,*,#15466,.F.);
#21125=ORIENTED_EDGE('',*,*,#15463,.F.);
#21126=ORIENTED_EDGE('',*,*,#15460,.F.);
#21127=ORIENTED_EDGE('',*,*,#15457,.F.);
#21128=ORIENTED_EDGE('',*,*,#15454,.F.);
#21129=ORIENTED_EDGE('',*,*,#15449,.F.);
#21130=ORIENTED_EDGE('',*,*,#15467,.T.);
#21131=ORIENTED_EDGE('',*,*,#15468,.F.);
#21132=ORIENTED_EDGE('',*,*,#15464,.T.);
#21133=ORIENTED_EDGE('',*,*,#15469,.T.);
#21134=ORIENTED_EDGE('',*,*,#15470,.T.);
#21135=ORIENTED_EDGE('',*,*,#15471,.T.);
#21136=ORIENTED_EDGE('',*,*,#15472,.T.);
#21137=ORIENTED_EDGE('',*,*,#15473,.T.);
#21138=ORIENTED_EDGE('',*,*,#15474,.T.);
#21139=ORIENTED_EDGE('',*,*,#15471,.F.);
#21140=ORIENTED_EDGE('',*,*,#15475,.T.);
#21141=ORIENTED_EDGE('',*,*,#15476,.T.);
#21142=ORIENTED_EDGE('',*,*,#15477,.T.);
#21143=ORIENTED_EDGE('',*,*,#15473,.F.);
#21144=ORIENTED_EDGE('',*,*,#15478,.T.);
#21145=ORIENTED_EDGE('',*,*,#15479,.T.);
#21146=ORIENTED_EDGE('',*,*,#15480,.T.);
#21147=ORIENTED_EDGE('',*,*,#15476,.F.);
#21148=ORIENTED_EDGE('',*,*,#15481,.T.);
#21149=ORIENTED_EDGE('',*,*,#15482,.T.);
#21150=ORIENTED_EDGE('',*,*,#15483,.T.);
#21151=ORIENTED_EDGE('',*,*,#15479,.F.);
#21152=ORIENTED_EDGE('',*,*,#15484,.T.);
#21153=ORIENTED_EDGE('',*,*,#15484,.F.);
#21154=ORIENTED_EDGE('',*,*,#15481,.F.);
#21155=ORIENTED_EDGE('',*,*,#15478,.F.);
#21156=ORIENTED_EDGE('',*,*,#15475,.F.);
#21157=ORIENTED_EDGE('',*,*,#15470,.F.);
#21158=ORIENTED_EDGE('',*,*,#15485,.F.);
#21159=ORIENTED_EDGE('',*,*,#15486,.T.);
#21160=ORIENTED_EDGE('',*,*,#15487,.T.);
#21161=ORIENTED_EDGE('',*,*,#15488,.T.);
#21162=ORIENTED_EDGE('',*,*,#15489,.T.);
#21163=ORIENTED_EDGE('',*,*,#15490,.T.);
#21164=ORIENTED_EDGE('',*,*,#15491,.T.);
#21165=ORIENTED_EDGE('',*,*,#15492,.T.);
#21166=ORIENTED_EDGE('',*,*,#15489,.F.);
#21167=ORIENTED_EDGE('',*,*,#15493,.T.);
#21168=ORIENTED_EDGE('',*,*,#15494,.T.);
#21169=ORIENTED_EDGE('',*,*,#15495,.T.);
#21170=ORIENTED_EDGE('',*,*,#15491,.F.);
#21171=ORIENTED_EDGE('',*,*,#15496,.T.);
#21172=ORIENTED_EDGE('',*,*,#15497,.T.);
#21173=ORIENTED_EDGE('',*,*,#15498,.T.);
#21174=ORIENTED_EDGE('',*,*,#15494,.F.);
#21175=ORIENTED_EDGE('',*,*,#15499,.T.);
#21176=ORIENTED_EDGE('',*,*,#15500,.T.);
#21177=ORIENTED_EDGE('',*,*,#15501,.T.);
#21178=ORIENTED_EDGE('',*,*,#15497,.F.);
#21179=ORIENTED_EDGE('',*,*,#15502,.T.);
#21180=ORIENTED_EDGE('',*,*,#15502,.F.);
#21181=ORIENTED_EDGE('',*,*,#15499,.F.);
#21182=ORIENTED_EDGE('',*,*,#15496,.F.);
#21183=ORIENTED_EDGE('',*,*,#15493,.F.);
#21184=ORIENTED_EDGE('',*,*,#15488,.F.);
#21185=ORIENTED_EDGE('',*,*,#15503,.F.);
#21186=ORIENTED_EDGE('',*,*,#15504,.T.);
#21187=ORIENTED_EDGE('',*,*,#15505,.T.);
#21188=ORIENTED_EDGE('',*,*,#15506,.T.);
#21189=ORIENTED_EDGE('',*,*,#15507,.T.);
#21190=ORIENTED_EDGE('',*,*,#15508,.T.);
#21191=ORIENTED_EDGE('',*,*,#15509,.T.);
#21192=ORIENTED_EDGE('',*,*,#15510,.T.);
#21193=ORIENTED_EDGE('',*,*,#15507,.F.);
#21194=ORIENTED_EDGE('',*,*,#15511,.T.);
#21195=ORIENTED_EDGE('',*,*,#15512,.T.);
#21196=ORIENTED_EDGE('',*,*,#15513,.T.);
#21197=ORIENTED_EDGE('',*,*,#15509,.F.);
#21198=ORIENTED_EDGE('',*,*,#15514,.T.);
#21199=ORIENTED_EDGE('',*,*,#15515,.T.);
#21200=ORIENTED_EDGE('',*,*,#15516,.T.);
#21201=ORIENTED_EDGE('',*,*,#15512,.F.);
#21202=ORIENTED_EDGE('',*,*,#15517,.T.);
#21203=ORIENTED_EDGE('',*,*,#15518,.T.);
#21204=ORIENTED_EDGE('',*,*,#15519,.T.);
#21205=ORIENTED_EDGE('',*,*,#15515,.F.);
#21206=ORIENTED_EDGE('',*,*,#15520,.T.);
#21207=ORIENTED_EDGE('',*,*,#15501,.F.);
#21208=ORIENTED_EDGE('',*,*,#15521,.F.);
#21209=ORIENTED_EDGE('',*,*,#15522,.T.);
#21210=ORIENTED_EDGE('',*,*,#15508,.F.);
#21211=ORIENTED_EDGE('',*,*,#15523,.F.);
#21212=ORIENTED_EDGE('',*,*,#15498,.F.);
#21213=ORIENTED_EDGE('',*,*,#15523,.T.);
#21214=ORIENTED_EDGE('',*,*,#15510,.F.);
#21215=ORIENTED_EDGE('',*,*,#15524,.T.);
#21216=ORIENTED_EDGE('',*,*,#15495,.F.);
#21217=ORIENTED_EDGE('',*,*,#15524,.F.);
#21218=ORIENTED_EDGE('',*,*,#15513,.F.);
#21219=ORIENTED_EDGE('',*,*,#15525,.F.);
#21220=ORIENTED_EDGE('',*,*,#15492,.F.);
#21221=ORIENTED_EDGE('',*,*,#15525,.T.);
#21222=ORIENTED_EDGE('',*,*,#15516,.F.);
#21223=ORIENTED_EDGE('',*,*,#15526,.T.);
#21224=ORIENTED_EDGE('',*,*,#15490,.F.);
#21225=ORIENTED_EDGE('',*,*,#15526,.F.);
#21226=ORIENTED_EDGE('',*,*,#15519,.F.);
#21227=ORIENTED_EDGE('',*,*,#15527,.T.);
#21228=ORIENTED_EDGE('',*,*,#15528,.F.);
#21229=ORIENTED_EDGE('',*,*,#15518,.F.);
#21230=ORIENTED_EDGE('',*,*,#15529,.F.);
#21231=ORIENTED_EDGE('',*,*,#15530,.F.);
#21232=ORIENTED_EDGE('',*,*,#15527,.F.);
#21233=ORIENTED_EDGE('',*,*,#15531,.T.);
#21234=ORIENTED_EDGE('',*,*,#15532,.T.);
#21235=ORIENTED_EDGE('',*,*,#15533,.T.);
#21236=ORIENTED_EDGE('',*,*,#15532,.F.);
#21237=ORIENTED_EDGE('',*,*,#15531,.F.);
#21238=ORIENTED_EDGE('',*,*,#15534,.F.);
#21239=ORIENTED_EDGE('',*,*,#15533,.F.);
#21240=ORIENTED_EDGE('',*,*,#15535,.T.);
#21241=ORIENTED_EDGE('',*,*,#15405,.F.);
#21242=ORIENTED_EDGE('',*,*,#15535,.F.);
#21243=ORIENTED_EDGE('',*,*,#15534,.T.);
#21244=ORIENTED_EDGE('',*,*,#15536,.T.);
#21245=ORIENTED_EDGE('',*,*,#15537,.T.);
#21246=ORIENTED_EDGE('',*,*,#15536,.F.);
#21247=ORIENTED_EDGE('',*,*,#15538,.F.);
#21248=ORIENTED_EDGE('',*,*,#15539,.T.);
#21249=ORIENTED_EDGE('',*,*,#15537,.F.);
#21250=ORIENTED_EDGE('',*,*,#15539,.F.);
#21251=ORIENTED_EDGE('',*,*,#15445,.T.);
#21252=ORIENTED_EDGE('',*,*,#15540,.T.);
#21253=ORIENTED_EDGE('',*,*,#15541,.T.);
#21254=ORIENTED_EDGE('',*,*,#15540,.F.);
#21255=ORIENTED_EDGE('',*,*,#15541,.F.);
#21256=ORIENTED_EDGE('',*,*,#15542,.T.);
#21257=ORIENTED_EDGE('',*,*,#15543,.T.);
#21258=ORIENTED_EDGE('',*,*,#15542,.F.);
#21259=ORIENTED_EDGE('',*,*,#15543,.F.);
#21260=ORIENTED_EDGE('',*,*,#15544,.T.);
#21261=ORIENTED_EDGE('',*,*,#15544,.F.);
#21262=ORIENTED_EDGE('',*,*,#15545,.T.);
#21263=ORIENTED_EDGE('',*,*,#15538,.T.);
#21264=ORIENTED_EDGE('',*,*,#15545,.F.);
#21265=ORIENTED_EDGE('',*,*,#15486,.F.);
#21266=ORIENTED_EDGE('',*,*,#15546,.T.);
#21267=ORIENTED_EDGE('',*,*,#15504,.F.);
#21268=ORIENTED_EDGE('',*,*,#15546,.F.);
#21269=ORIENTED_EDGE('',*,*,#15459,.F.);
#21270=ORIENTED_EDGE('',*,*,#15547,.T.);
#21271=ORIENTED_EDGE('',*,*,#15474,.F.);
#21272=ORIENTED_EDGE('',*,*,#15548,.T.);
#21273=ORIENTED_EDGE('',*,*,#15456,.F.);
#21274=ORIENTED_EDGE('',*,*,#15548,.F.);
#21275=ORIENTED_EDGE('',*,*,#15477,.F.);
#21276=ORIENTED_EDGE('',*,*,#15549,.F.);
#21277=ORIENTED_EDGE('',*,*,#15453,.F.);
#21278=ORIENTED_EDGE('',*,*,#15549,.T.);
#21279=ORIENTED_EDGE('',*,*,#15480,.F.);
#21280=ORIENTED_EDGE('',*,*,#15550,.T.);
#21281=ORIENTED_EDGE('',*,*,#15448,.F.);
#21282=ORIENTED_EDGE('',*,*,#15551,.F.);
#21283=ORIENTED_EDGE('',*,*,#15552,.F.);
#21284=ORIENTED_EDGE('',*,*,#15467,.F.);
#21285=ORIENTED_EDGE('',*,*,#15451,.F.);
#21286=ORIENTED_EDGE('',*,*,#15550,.F.);
#21287=ORIENTED_EDGE('',*,*,#15483,.F.);
#21288=ORIENTED_EDGE('',*,*,#15553,.F.);
#21289=ORIENTED_EDGE('',*,*,#15551,.T.);
#21290=ORIENTED_EDGE('',*,*,#15462,.F.);
#21291=ORIENTED_EDGE('',*,*,#15466,.T.);
#21292=ORIENTED_EDGE('',*,*,#15554,.F.);
#21293=ORIENTED_EDGE('',*,*,#15472,.F.);
#21294=ORIENTED_EDGE('',*,*,#15547,.F.);
#21295=ORIENTED_EDGE('',*,*,#15468,.T.);
#21296=ORIENTED_EDGE('',*,*,#15555,.F.);
#21297=ORIENTED_EDGE('',*,*,#15505,.F.);
#21298=ORIENTED_EDGE('',*,*,#15522,.F.);
#21299=ORIENTED_EDGE('',*,*,#15556,.F.);
#21300=ORIENTED_EDGE('',*,*,#15557,.F.);
#21301=ORIENTED_EDGE('',*,*,#15506,.F.);
#21302=ORIENTED_EDGE('',*,*,#15557,.T.);
#21303=ORIENTED_EDGE('',*,*,#15558,.F.);
#21304=ORIENTED_EDGE('',*,*,#15529,.T.);
#21305=ORIENTED_EDGE('',*,*,#15520,.F.);
#21306=ORIENTED_EDGE('',*,*,#15517,.F.);
#21307=ORIENTED_EDGE('',*,*,#15514,.F.);
#21308=ORIENTED_EDGE('',*,*,#15511,.F.);
#21309=ORIENTED_EDGE('',*,*,#15558,.T.);
#21310=ORIENTED_EDGE('',*,*,#15559,.F.);
#21311=ORIENTED_EDGE('',*,*,#15554,.T.);
#21312=ORIENTED_EDGE('',*,*,#15560,.F.);
#21313=ORIENTED_EDGE('',*,*,#15561,.F.);
#21314=ORIENTED_EDGE('',*,*,#15521,.T.);
#21315=ORIENTED_EDGE('',*,*,#15500,.F.);
#21316=ORIENTED_EDGE('',*,*,#15503,.T.);
#21317=ORIENTED_EDGE('',*,*,#15487,.F.);
#21318=ORIENTED_EDGE('',*,*,#15528,.T.);
#21319=ORIENTED_EDGE('',*,*,#15562,.F.);
#21320=ORIENTED_EDGE('',*,*,#15553,.T.);
#21321=ORIENTED_EDGE('',*,*,#15482,.F.);
#21322=ORIENTED_EDGE('',*,*,#15485,.T.);
#21323=ORIENTED_EDGE('',*,*,#15469,.F.);
#21324=ORIENTED_EDGE('',*,*,#15561,.T.);
#21325=ORIENTED_EDGE('',*,*,#15563,.T.);
#21326=ORIENTED_EDGE('',*,*,#15564,.T.);
#21327=ORIENTED_EDGE('',*,*,#15563,.F.);
#21328=ORIENTED_EDGE('',*,*,#15560,.T.);
#21329=ORIENTED_EDGE('',*,*,#15465,.T.);
#21330=ORIENTED_EDGE('',*,*,#15555,.T.);
#21331=ORIENTED_EDGE('',*,*,#15552,.T.);
#21332=ORIENTED_EDGE('',*,*,#15562,.T.);
#21333=ORIENTED_EDGE('',*,*,#15530,.T.);
#21334=ORIENTED_EDGE('',*,*,#15559,.T.);
#21335=ORIENTED_EDGE('',*,*,#15556,.T.);
#21336=ORIENTED_EDGE('',*,*,#15564,.F.);
#21337=ORIENTED_EDGE('',*,*,#15565,.T.);
#21338=ORIENTED_EDGE('',*,*,#15404,.F.);
#21339=ORIENTED_EDGE('',*,*,#15565,.F.);
#21340=ORIENTED_EDGE('',*,*,#15566,.T.);
#21341=ORIENTED_EDGE('',*,*,#15567,.T.);
#21342=ORIENTED_EDGE('',*,*,#15568,.T.);
#21343=ORIENTED_EDGE('',*,*,#15567,.F.);
#21344=ORIENTED_EDGE('',*,*,#15569,.F.);
#21345=ORIENTED_EDGE('',*,*,#15570,.T.);
#21346=ORIENTED_EDGE('',*,*,#15568,.F.);
#21347=ORIENTED_EDGE('',*,*,#15570,.F.);
#21348=ORIENTED_EDGE('',*,*,#15571,.T.);
#21349=ORIENTED_EDGE('',*,*,#15566,.F.);
#21350=ORIENTED_EDGE('',*,*,#15572,.F.);
#21351=ORIENTED_EDGE('',*,*,#15414,.F.);
#21352=ORIENTED_EDGE('',*,*,#15410,.F.);
#21353=ORIENTED_EDGE('',*,*,#15406,.F.);
#21354=ORIENTED_EDGE('',*,*,#15573,.F.);
#21355=ORIENTED_EDGE('',*,*,#15408,.F.);
#21356=ORIENTED_EDGE('',*,*,#15412,.T.);
#21357=ORIENTED_EDGE('',*,*,#15413,.F.);
#21358=ORIENTED_EDGE('',*,*,#15569,.T.);
#21359=ORIENTED_EDGE('',*,*,#15574,.T.);
#21360=ORIENTED_EDGE('',*,*,#15575,.T.);
#21361=ORIENTED_EDGE('',*,*,#15403,.T.);
#21362=ORIENTED_EDGE('',*,*,#15575,.F.);
#21363=ORIENTED_EDGE('',*,*,#15576,.T.);
#21364=ORIENTED_EDGE('',*,*,#15577,.F.);
#21365=ORIENTED_EDGE('',*,*,#15578,.T.);
#21366=ORIENTED_EDGE('',*,*,#15576,.F.);
#21367=ORIENTED_EDGE('',*,*,#15574,.F.);
#21368=ORIENTED_EDGE('',*,*,#15578,.F.);
#21369=ORIENTED_EDGE('',*,*,#15573,.T.);
#21370=ORIENTED_EDGE('',*,*,#15415,.F.);
#21371=ORIENTED_EDGE('',*,*,#15572,.T.);
#21372=ORIENTED_EDGE('',*,*,#15409,.F.);
#21373=ORIENTED_EDGE('',*,*,#15579,.F.);
#21374=ORIENTED_EDGE('',*,*,#15577,.T.);
#21375=ORIENTED_EDGE('',*,*,#15580,.F.);
#21376=ORIENTED_EDGE('',*,*,#15581,.T.);
#21377=ORIENTED_EDGE('',*,*,#15579,.T.);
#21378=ORIENTED_EDGE('',*,*,#15581,.F.);
#21379=ORIENTED_EDGE('',*,*,#15582,.F.);
#21380=ORIENTED_EDGE('',*,*,#15583,.T.);
#21381=ORIENTED_EDGE('',*,*,#15580,.T.);
#21382=ORIENTED_EDGE('',*,*,#15583,.F.);
#21383=ORIENTED_EDGE('',*,*,#15571,.F.);
#21384=ORIENTED_EDGE('',*,*,#15584,.T.);
#21385=ORIENTED_EDGE('',*,*,#15582,.T.);
#21386=ORIENTED_EDGE('',*,*,#15584,.F.);
#21387=ORIENTED_EDGE('',*,*,#15585,.T.);
#21388=ORIENTED_EDGE('',*,*,#15440,.T.);
#21389=ORIENTED_EDGE('',*,*,#15586,.T.);
#21390=ORIENTED_EDGE('',*,*,#15587,.T.);
#21391=ORIENTED_EDGE('',*,*,#15588,.T.);
#21392=ORIENTED_EDGE('',*,*,#15437,.T.);
#21393=ORIENTED_EDGE('',*,*,#15585,.F.);
#21394=ORIENTED_EDGE('',*,*,#15589,.T.);
#21395=ORIENTED_EDGE('',*,*,#15590,.T.);
#21396=ORIENTED_EDGE('',*,*,#15591,.T.);
#21397=ORIENTED_EDGE('',*,*,#15588,.F.);
#21398=ORIENTED_EDGE('',*,*,#15592,.T.);
#21399=ORIENTED_EDGE('',*,*,#15593,.T.);
#21400=ORIENTED_EDGE('',*,*,#15594,.T.);
#21401=ORIENTED_EDGE('',*,*,#15590,.F.);
#21402=ORIENTED_EDGE('',*,*,#15595,.T.);
#21403=ORIENTED_EDGE('',*,*,#15596,.T.);
#21404=ORIENTED_EDGE('',*,*,#15597,.T.);
#21405=ORIENTED_EDGE('',*,*,#15593,.F.);
#21406=ORIENTED_EDGE('',*,*,#15598,.T.);
#21407=ORIENTED_EDGE('',*,*,#15599,.T.);
#21408=ORIENTED_EDGE('',*,*,#15600,.T.);
#21409=ORIENTED_EDGE('',*,*,#15596,.F.);
#21410=ORIENTED_EDGE('',*,*,#15601,.T.);
#21411=ORIENTED_EDGE('',*,*,#15602,.T.);
#21412=ORIENTED_EDGE('',*,*,#15444,.T.);
#21413=ORIENTED_EDGE('',*,*,#15599,.F.);
#21414=ORIENTED_EDGE('',*,*,#15603,.T.);
#21415=ORIENTED_EDGE('',*,*,#15586,.F.);
#21416=ORIENTED_EDGE('',*,*,#15442,.T.);
#21417=ORIENTED_EDGE('',*,*,#15602,.F.);
#21418=ORIENTED_EDGE('',*,*,#15604,.T.);
#21419=ORIENTED_EDGE('',*,*,#15435,.F.);
#21420=ORIENTED_EDGE('',*,*,#15605,.T.);
#21421=ORIENTED_EDGE('',*,*,#15600,.F.);
#21422=ORIENTED_EDGE('',*,*,#15443,.T.);
#21423=ORIENTED_EDGE('',*,*,#15587,.F.);
#21424=ORIENTED_EDGE('',*,*,#15604,.F.);
#21425=ORIENTED_EDGE('',*,*,#15603,.F.);
#21426=ORIENTED_EDGE('',*,*,#15601,.F.);
#21427=ORIENTED_EDGE('',*,*,#15598,.F.);
#21428=ORIENTED_EDGE('',*,*,#15595,.F.);
#21429=ORIENTED_EDGE('',*,*,#15592,.F.);
#21430=ORIENTED_EDGE('',*,*,#15589,.F.);
#21431=ORIENTED_EDGE('',*,*,#15381,.F.);
#21432=ORIENTED_EDGE('',*,*,#15606,.T.);
#21433=ORIENTED_EDGE('',*,*,#15427,.F.);
#21434=ORIENTED_EDGE('',*,*,#15446,.F.);
#21435=ORIENTED_EDGE('',*,*,#15384,.F.);
#21436=ORIENTED_EDGE('',*,*,#15396,.T.);
#21437=ORIENTED_EDGE('',*,*,#15424,.F.);
#21438=ORIENTED_EDGE('',*,*,#15606,.F.);
#21439=ORIENTED_EDGE('',*,*,#15434,.F.);
#21440=ORIENTED_EDGE('',*,*,#15607,.F.);
#21441=ORIENTED_EDGE('',*,*,#15597,.F.);
#21442=ORIENTED_EDGE('',*,*,#15605,.F.);
#21443=ORIENTED_EDGE('',*,*,#15431,.F.);
#21444=ORIENTED_EDGE('',*,*,#15608,.T.);
#21445=ORIENTED_EDGE('',*,*,#15594,.F.);
#21446=ORIENTED_EDGE('',*,*,#15607,.T.);
#21447=ORIENTED_EDGE('',*,*,#15428,.F.);
#21448=ORIENTED_EDGE('',*,*,#15438,.F.);
#21449=ORIENTED_EDGE('',*,*,#15591,.F.);
#21450=ORIENTED_EDGE('',*,*,#15608,.F.);
#21451=ORIENTED_EDGE('',*,*,#15609,.F.);
#21452=ORIENTED_EDGE('',*,*,#15610,.T.);
#21453=ORIENTED_EDGE('',*,*,#15611,.T.);
#21454=ORIENTED_EDGE('',*,*,#15612,.T.);
#21455=ORIENTED_EDGE('',*,*,#15613,.F.);
#21456=ORIENTED_EDGE('',*,*,#15614,.T.);
#21457=ORIENTED_EDGE('',*,*,#15609,.T.);
#21458=ORIENTED_EDGE('',*,*,#15615,.T.);
#21459=ORIENTED_EDGE('',*,*,#15616,.F.);
#21460=ORIENTED_EDGE('',*,*,#15617,.T.);
#21461=ORIENTED_EDGE('',*,*,#15613,.T.);
#21462=ORIENTED_EDGE('',*,*,#15618,.T.);
#21463=ORIENTED_EDGE('',*,*,#15619,.F.);
#21464=ORIENTED_EDGE('',*,*,#15620,.T.);
#21465=ORIENTED_EDGE('',*,*,#15616,.T.);
#21466=ORIENTED_EDGE('',*,*,#15621,.T.);
#21467=ORIENTED_EDGE('',*,*,#15622,.F.);
#21468=ORIENTED_EDGE('',*,*,#15623,.F.);
#21469=ORIENTED_EDGE('',*,*,#15624,.T.);
#21470=ORIENTED_EDGE('',*,*,#15619,.T.);
#21471=ORIENTED_EDGE('',*,*,#15625,.T.);
#21472=ORIENTED_EDGE('',*,*,#15626,.F.);
#21473=ORIENTED_EDGE('',*,*,#15627,.T.);
#21474=ORIENTED_EDGE('',*,*,#15628,.F.);
#21475=ORIENTED_EDGE('',*,*,#15629,.F.);
#21476=ORIENTED_EDGE('',*,*,#15630,.F.);
#21477=ORIENTED_EDGE('',*,*,#15631,.T.);
#21478=ORIENTED_EDGE('',*,*,#15626,.T.);
#21479=ORIENTED_EDGE('',*,*,#15632,.F.);
#21480=ORIENTED_EDGE('',*,*,#15633,.F.);
#21481=ORIENTED_EDGE('',*,*,#15634,.T.);
#21482=ORIENTED_EDGE('',*,*,#15630,.T.);
#21483=ORIENTED_EDGE('',*,*,#15635,.F.);
#21484=ORIENTED_EDGE('',*,*,#15636,.F.);
#21485=ORIENTED_EDGE('',*,*,#15637,.T.);
#21486=ORIENTED_EDGE('',*,*,#15633,.T.);
#21487=ORIENTED_EDGE('',*,*,#15638,.F.);
#21488=ORIENTED_EDGE('',*,*,#15639,.F.);
#21489=ORIENTED_EDGE('',*,*,#15640,.T.);
#21490=ORIENTED_EDGE('',*,*,#15641,.F.);
#21491=ORIENTED_EDGE('',*,*,#15642,.F.);
#21492=ORIENTED_EDGE('',*,*,#15643,.F.);
#21493=ORIENTED_EDGE('',*,*,#15641,.T.);
#21494=ORIENTED_EDGE('',*,*,#15644,.T.);
#21495=ORIENTED_EDGE('',*,*,#15645,.F.);
#21496=ORIENTED_EDGE('',*,*,#15646,.T.);
#21497=ORIENTED_EDGE('',*,*,#15644,.F.);
#21498=ORIENTED_EDGE('',*,*,#15640,.F.);
#21499=ORIENTED_EDGE('',*,*,#15647,.F.);
#21500=ORIENTED_EDGE('',*,*,#15648,.T.);
#21501=ORIENTED_EDGE('',*,*,#15649,.F.);
#21502=ORIENTED_EDGE('',*,*,#15650,.F.);
#21503=ORIENTED_EDGE('',*,*,#15651,.F.);
#21504=ORIENTED_EDGE('',*,*,#15649,.T.);
#21505=ORIENTED_EDGE('',*,*,#15652,.T.);
#21506=ORIENTED_EDGE('',*,*,#15653,.F.);
#21507=ORIENTED_EDGE('',*,*,#15654,.T.);
#21508=ORIENTED_EDGE('',*,*,#15652,.F.);
#21509=ORIENTED_EDGE('',*,*,#15648,.F.);
#21510=ORIENTED_EDGE('',*,*,#15655,.F.);
#21511=ORIENTED_EDGE('',*,*,#15656,.T.);
#21512=ORIENTED_EDGE('',*,*,#15657,.F.);
#21513=ORIENTED_EDGE('',*,*,#15658,.F.);
#21514=ORIENTED_EDGE('',*,*,#15659,.F.);
#21515=ORIENTED_EDGE('',*,*,#15657,.T.);
#21516=ORIENTED_EDGE('',*,*,#15660,.T.);
#21517=ORIENTED_EDGE('',*,*,#15661,.F.);
#21518=ORIENTED_EDGE('',*,*,#15662,.T.);
#21519=ORIENTED_EDGE('',*,*,#15660,.F.);
#21520=ORIENTED_EDGE('',*,*,#15656,.F.);
#21521=ORIENTED_EDGE('',*,*,#15663,.F.);
#21522=ORIENTED_EDGE('',*,*,#15664,.T.);
#21523=ORIENTED_EDGE('',*,*,#15665,.F.);
#21524=ORIENTED_EDGE('',*,*,#15666,.F.);
#21525=ORIENTED_EDGE('',*,*,#15667,.F.);
#21526=ORIENTED_EDGE('',*,*,#15665,.T.);
#21527=ORIENTED_EDGE('',*,*,#15668,.T.);
#21528=ORIENTED_EDGE('',*,*,#15669,.F.);
#21529=ORIENTED_EDGE('',*,*,#15670,.T.);
#21530=ORIENTED_EDGE('',*,*,#15668,.F.);
#21531=ORIENTED_EDGE('',*,*,#15664,.F.);
#21532=ORIENTED_EDGE('',*,*,#15671,.F.);
#21533=ORIENTED_EDGE('',*,*,#15672,.T.);
#21534=ORIENTED_EDGE('',*,*,#15673,.F.);
#21535=ORIENTED_EDGE('',*,*,#15674,.F.);
#21536=ORIENTED_EDGE('',*,*,#15675,.F.);
#21537=ORIENTED_EDGE('',*,*,#15673,.T.);
#21538=ORIENTED_EDGE('',*,*,#15676,.T.);
#21539=ORIENTED_EDGE('',*,*,#15677,.F.);
#21540=ORIENTED_EDGE('',*,*,#15678,.T.);
#21541=ORIENTED_EDGE('',*,*,#15676,.F.);
#21542=ORIENTED_EDGE('',*,*,#15672,.F.);
#21543=ORIENTED_EDGE('',*,*,#15679,.F.);
#21544=ORIENTED_EDGE('',*,*,#15680,.T.);
#21545=ORIENTED_EDGE('',*,*,#15681,.F.);
#21546=ORIENTED_EDGE('',*,*,#15682,.F.);
#21547=ORIENTED_EDGE('',*,*,#15683,.F.);
#21548=ORIENTED_EDGE('',*,*,#15681,.T.);
#21549=ORIENTED_EDGE('',*,*,#15684,.T.);
#21550=ORIENTED_EDGE('',*,*,#15685,.F.);
#21551=ORIENTED_EDGE('',*,*,#15686,.T.);
#21552=ORIENTED_EDGE('',*,*,#15687,.T.);
#21553=ORIENTED_EDGE('',*,*,#15684,.F.);
#21554=ORIENTED_EDGE('',*,*,#15680,.F.);
#21555=ORIENTED_EDGE('',*,*,#15688,.F.);
#21556=ORIENTED_EDGE('',*,*,#15689,.T.);
#21557=ORIENTED_EDGE('',*,*,#15690,.F.);
#21558=ORIENTED_EDGE('',*,*,#15691,.F.);
#21559=ORIENTED_EDGE('',*,*,#15692,.F.);
#21560=ORIENTED_EDGE('',*,*,#15690,.T.);
#21561=ORIENTED_EDGE('',*,*,#15693,.T.);
#21562=ORIENTED_EDGE('',*,*,#15694,.F.);
#21563=ORIENTED_EDGE('',*,*,#15695,.T.);
#21564=ORIENTED_EDGE('',*,*,#15693,.F.);
#21565=ORIENTED_EDGE('',*,*,#15689,.F.);
#21566=ORIENTED_EDGE('',*,*,#15696,.F.);
#21567=ORIENTED_EDGE('',*,*,#15697,.T.);
#21568=ORIENTED_EDGE('',*,*,#15698,.F.);
#21569=ORIENTED_EDGE('',*,*,#15699,.F.);
#21570=ORIENTED_EDGE('',*,*,#15700,.F.);
#21571=ORIENTED_EDGE('',*,*,#15698,.T.);
#21572=ORIENTED_EDGE('',*,*,#15701,.T.);
#21573=ORIENTED_EDGE('',*,*,#15702,.F.);
#21574=ORIENTED_EDGE('',*,*,#15703,.T.);
#21575=ORIENTED_EDGE('',*,*,#15701,.F.);
#21576=ORIENTED_EDGE('',*,*,#15697,.F.);
#21577=ORIENTED_EDGE('',*,*,#15704,.F.);
#21578=ORIENTED_EDGE('',*,*,#15705,.T.);
#21579=ORIENTED_EDGE('',*,*,#15706,.F.);
#21580=ORIENTED_EDGE('',*,*,#15707,.F.);
#21581=ORIENTED_EDGE('',*,*,#15708,.F.);
#21582=ORIENTED_EDGE('',*,*,#15706,.T.);
#21583=ORIENTED_EDGE('',*,*,#15709,.T.);
#21584=ORIENTED_EDGE('',*,*,#15710,.F.);
#21585=ORIENTED_EDGE('',*,*,#15711,.T.);
#21586=ORIENTED_EDGE('',*,*,#15709,.F.);
#21587=ORIENTED_EDGE('',*,*,#15705,.F.);
#21588=ORIENTED_EDGE('',*,*,#15712,.F.);
#21589=ORIENTED_EDGE('',*,*,#15713,.T.);
#21590=ORIENTED_EDGE('',*,*,#15714,.F.);
#21591=ORIENTED_EDGE('',*,*,#15715,.F.);
#21592=ORIENTED_EDGE('',*,*,#15716,.F.);
#21593=ORIENTED_EDGE('',*,*,#15714,.T.);
#21594=ORIENTED_EDGE('',*,*,#15717,.T.);
#21595=ORIENTED_EDGE('',*,*,#15718,.F.);
#21596=ORIENTED_EDGE('',*,*,#15719,.T.);
#21597=ORIENTED_EDGE('',*,*,#15717,.F.);
#21598=ORIENTED_EDGE('',*,*,#15713,.F.);
#21599=ORIENTED_EDGE('',*,*,#15720,.F.);
#21600=ORIENTED_EDGE('',*,*,#15721,.T.);
#21601=ORIENTED_EDGE('',*,*,#15722,.F.);
#21602=ORIENTED_EDGE('',*,*,#15723,.F.);
#21603=ORIENTED_EDGE('',*,*,#15724,.F.);
#21604=ORIENTED_EDGE('',*,*,#15722,.T.);
#21605=ORIENTED_EDGE('',*,*,#15725,.T.);
#21606=ORIENTED_EDGE('',*,*,#15726,.F.);
#21607=ORIENTED_EDGE('',*,*,#15727,.T.);
#21608=ORIENTED_EDGE('',*,*,#15725,.F.);
#21609=ORIENTED_EDGE('',*,*,#15721,.F.);
#21610=ORIENTED_EDGE('',*,*,#15728,.F.);
#21611=ORIENTED_EDGE('',*,*,#15729,.T.);
#21612=ORIENTED_EDGE('',*,*,#15730,.F.);
#21613=ORIENTED_EDGE('',*,*,#15731,.F.);
#21614=ORIENTED_EDGE('',*,*,#15732,.F.);
#21615=ORIENTED_EDGE('',*,*,#15730,.T.);
#21616=ORIENTED_EDGE('',*,*,#15733,.T.);
#21617=ORIENTED_EDGE('',*,*,#15734,.F.);
#21618=ORIENTED_EDGE('',*,*,#15735,.T.);
#21619=ORIENTED_EDGE('',*,*,#15733,.F.);
#21620=ORIENTED_EDGE('',*,*,#15729,.F.);
#21621=ORIENTED_EDGE('',*,*,#15736,.F.);
#21622=ORIENTED_EDGE('',*,*,#15737,.T.);
#21623=ORIENTED_EDGE('',*,*,#15738,.F.);
#21624=ORIENTED_EDGE('',*,*,#15739,.F.);
#21625=ORIENTED_EDGE('',*,*,#15740,.F.);
#21626=ORIENTED_EDGE('',*,*,#15738,.T.);
#21627=ORIENTED_EDGE('',*,*,#15741,.T.);
#21628=ORIENTED_EDGE('',*,*,#15742,.F.);
#21629=ORIENTED_EDGE('',*,*,#15743,.T.);
#21630=ORIENTED_EDGE('',*,*,#15741,.F.);
#21631=ORIENTED_EDGE('',*,*,#15737,.F.);
#21632=ORIENTED_EDGE('',*,*,#15744,.F.);
#21633=ORIENTED_EDGE('',*,*,#15745,.T.);
#21634=ORIENTED_EDGE('',*,*,#15746,.F.);
#21635=ORIENTED_EDGE('',*,*,#15747,.F.);
#21636=ORIENTED_EDGE('',*,*,#15748,.F.);
#21637=ORIENTED_EDGE('',*,*,#15746,.T.);
#21638=ORIENTED_EDGE('',*,*,#15749,.T.);
#21639=ORIENTED_EDGE('',*,*,#15750,.F.);
#21640=ORIENTED_EDGE('',*,*,#15751,.T.);
#21641=ORIENTED_EDGE('',*,*,#15749,.F.);
#21642=ORIENTED_EDGE('',*,*,#15745,.F.);
#21643=ORIENTED_EDGE('',*,*,#15752,.F.);
#21644=ORIENTED_EDGE('',*,*,#15753,.T.);
#21645=ORIENTED_EDGE('',*,*,#15754,.F.);
#21646=ORIENTED_EDGE('',*,*,#15755,.F.);
#21647=ORIENTED_EDGE('',*,*,#15756,.F.);
#21648=ORIENTED_EDGE('',*,*,#15754,.T.);
#21649=ORIENTED_EDGE('',*,*,#15757,.T.);
#21650=ORIENTED_EDGE('',*,*,#15758,.F.);
#21651=ORIENTED_EDGE('',*,*,#15759,.T.);
#21652=ORIENTED_EDGE('',*,*,#15757,.F.);
#21653=ORIENTED_EDGE('',*,*,#15753,.F.);
#21654=ORIENTED_EDGE('',*,*,#15760,.F.);
#21655=ORIENTED_EDGE('',*,*,#15761,.T.);
#21656=ORIENTED_EDGE('',*,*,#15762,.F.);
#21657=ORIENTED_EDGE('',*,*,#15763,.F.);
#21658=ORIENTED_EDGE('',*,*,#15764,.F.);
#21659=ORIENTED_EDGE('',*,*,#15762,.T.);
#21660=ORIENTED_EDGE('',*,*,#15765,.T.);
#21661=ORIENTED_EDGE('',*,*,#15766,.F.);
#21662=ORIENTED_EDGE('',*,*,#15767,.T.);
#21663=ORIENTED_EDGE('',*,*,#15765,.F.);
#21664=ORIENTED_EDGE('',*,*,#15761,.F.);
#21665=ORIENTED_EDGE('',*,*,#15768,.F.);
#21666=ORIENTED_EDGE('',*,*,#15769,.T.);
#21667=ORIENTED_EDGE('',*,*,#15770,.F.);
#21668=ORIENTED_EDGE('',*,*,#15771,.F.);
#21669=ORIENTED_EDGE('',*,*,#15772,.F.);
#21670=ORIENTED_EDGE('',*,*,#15770,.T.);
#21671=ORIENTED_EDGE('',*,*,#15773,.T.);
#21672=ORIENTED_EDGE('',*,*,#15774,.F.);
#21673=ORIENTED_EDGE('',*,*,#15775,.T.);
#21674=ORIENTED_EDGE('',*,*,#15773,.F.);
#21675=ORIENTED_EDGE('',*,*,#15769,.F.);
#21676=ORIENTED_EDGE('',*,*,#15776,.F.);
#21677=ORIENTED_EDGE('',*,*,#15777,.T.);
#21678=ORIENTED_EDGE('',*,*,#15778,.F.);
#21679=ORIENTED_EDGE('',*,*,#15779,.F.);
#21680=ORIENTED_EDGE('',*,*,#15780,.F.);
#21681=ORIENTED_EDGE('',*,*,#15778,.T.);
#21682=ORIENTED_EDGE('',*,*,#15781,.T.);
#21683=ORIENTED_EDGE('',*,*,#15782,.F.);
#21684=ORIENTED_EDGE('',*,*,#15783,.T.);
#21685=ORIENTED_EDGE('',*,*,#15781,.F.);
#21686=ORIENTED_EDGE('',*,*,#15777,.F.);
#21687=ORIENTED_EDGE('',*,*,#15784,.F.);
#21688=ORIENTED_EDGE('',*,*,#15785,.T.);
#21689=ORIENTED_EDGE('',*,*,#15786,.F.);
#21690=ORIENTED_EDGE('',*,*,#15787,.F.);
#21691=ORIENTED_EDGE('',*,*,#15788,.F.);
#21692=ORIENTED_EDGE('',*,*,#15786,.T.);
#21693=ORIENTED_EDGE('',*,*,#15789,.T.);
#21694=ORIENTED_EDGE('',*,*,#15790,.F.);
#21695=ORIENTED_EDGE('',*,*,#15791,.T.);
#21696=ORIENTED_EDGE('',*,*,#15789,.F.);
#21697=ORIENTED_EDGE('',*,*,#15785,.F.);
#21698=ORIENTED_EDGE('',*,*,#15792,.F.);
#21699=ORIENTED_EDGE('',*,*,#15793,.T.);
#21700=ORIENTED_EDGE('',*,*,#15794,.F.);
#21701=ORIENTED_EDGE('',*,*,#15795,.F.);
#21702=ORIENTED_EDGE('',*,*,#15796,.F.);
#21703=ORIENTED_EDGE('',*,*,#15794,.T.);
#21704=ORIENTED_EDGE('',*,*,#15797,.T.);
#21705=ORIENTED_EDGE('',*,*,#15798,.F.);
#21706=ORIENTED_EDGE('',*,*,#15799,.T.);
#21707=ORIENTED_EDGE('',*,*,#15797,.F.);
#21708=ORIENTED_EDGE('',*,*,#15793,.F.);
#21709=ORIENTED_EDGE('',*,*,#15800,.F.);
#21710=ORIENTED_EDGE('',*,*,#15801,.T.);
#21711=ORIENTED_EDGE('',*,*,#15802,.F.);
#21712=ORIENTED_EDGE('',*,*,#15803,.F.);
#21713=ORIENTED_EDGE('',*,*,#15804,.F.);
#21714=ORIENTED_EDGE('',*,*,#15802,.T.);
#21715=ORIENTED_EDGE('',*,*,#15805,.T.);
#21716=ORIENTED_EDGE('',*,*,#15806,.F.);
#21717=ORIENTED_EDGE('',*,*,#15807,.T.);
#21718=ORIENTED_EDGE('',*,*,#15805,.F.);
#21719=ORIENTED_EDGE('',*,*,#15801,.F.);
#21720=ORIENTED_EDGE('',*,*,#15808,.F.);
#21721=ORIENTED_EDGE('',*,*,#15809,.T.);
#21722=ORIENTED_EDGE('',*,*,#15810,.F.);
#21723=ORIENTED_EDGE('',*,*,#15811,.F.);
#21724=ORIENTED_EDGE('',*,*,#15812,.F.);
#21725=ORIENTED_EDGE('',*,*,#15810,.T.);
#21726=ORIENTED_EDGE('',*,*,#15813,.T.);
#21727=ORIENTED_EDGE('',*,*,#15814,.F.);
#21728=ORIENTED_EDGE('',*,*,#15815,.T.);
#21729=ORIENTED_EDGE('',*,*,#15813,.F.);
#21730=ORIENTED_EDGE('',*,*,#15809,.F.);
#21731=ORIENTED_EDGE('',*,*,#15816,.F.);
#21732=ORIENTED_EDGE('',*,*,#15817,.T.);
#21733=ORIENTED_EDGE('',*,*,#15818,.F.);
#21734=ORIENTED_EDGE('',*,*,#15819,.F.);
#21735=ORIENTED_EDGE('',*,*,#15820,.F.);
#21736=ORIENTED_EDGE('',*,*,#15818,.T.);
#21737=ORIENTED_EDGE('',*,*,#15821,.T.);
#21738=ORIENTED_EDGE('',*,*,#15822,.F.);
#21739=ORIENTED_EDGE('',*,*,#15823,.T.);
#21740=ORIENTED_EDGE('',*,*,#15821,.F.);
#21741=ORIENTED_EDGE('',*,*,#15817,.F.);
#21742=ORIENTED_EDGE('',*,*,#15824,.F.);
#21743=ORIENTED_EDGE('',*,*,#15825,.T.);
#21744=ORIENTED_EDGE('',*,*,#15826,.F.);
#21745=ORIENTED_EDGE('',*,*,#15827,.F.);
#21746=ORIENTED_EDGE('',*,*,#15828,.F.);
#21747=ORIENTED_EDGE('',*,*,#15826,.T.);
#21748=ORIENTED_EDGE('',*,*,#15829,.T.);
#21749=ORIENTED_EDGE('',*,*,#15830,.F.);
#21750=ORIENTED_EDGE('',*,*,#15831,.T.);
#21751=ORIENTED_EDGE('',*,*,#15829,.F.);
#21752=ORIENTED_EDGE('',*,*,#15825,.F.);
#21753=ORIENTED_EDGE('',*,*,#15832,.F.);
#21754=ORIENTED_EDGE('',*,*,#15833,.T.);
#21755=ORIENTED_EDGE('',*,*,#15683,.T.);
#21756=ORIENTED_EDGE('',*,*,#15834,.T.);
#21757=ORIENTED_EDGE('',*,*,#15787,.T.);
#21758=ORIENTED_EDGE('',*,*,#15788,.T.);
#21759=ORIENTED_EDGE('',*,*,#15835,.T.);
#21760=ORIENTED_EDGE('',*,*,#15674,.T.);
#21761=ORIENTED_EDGE('',*,*,#15675,.T.);
#21762=ORIENTED_EDGE('',*,*,#15836,.T.);
#21763=ORIENTED_EDGE('',*,*,#15795,.T.);
#21764=ORIENTED_EDGE('',*,*,#15796,.T.);
#21765=ORIENTED_EDGE('',*,*,#15837,.T.);
#21766=ORIENTED_EDGE('',*,*,#15666,.T.);
#21767=ORIENTED_EDGE('',*,*,#15667,.T.);
#21768=ORIENTED_EDGE('',*,*,#15838,.T.);
#21769=ORIENTED_EDGE('',*,*,#15803,.T.);
#21770=ORIENTED_EDGE('',*,*,#15804,.T.);
#21771=ORIENTED_EDGE('',*,*,#15839,.T.);
#21772=ORIENTED_EDGE('',*,*,#15658,.T.);
#21773=ORIENTED_EDGE('',*,*,#15659,.T.);
#21774=ORIENTED_EDGE('',*,*,#15840,.T.);
#21775=ORIENTED_EDGE('',*,*,#15811,.T.);
#21776=ORIENTED_EDGE('',*,*,#15812,.T.);
#21777=ORIENTED_EDGE('',*,*,#15841,.T.);
#21778=ORIENTED_EDGE('',*,*,#15650,.T.);
#21779=ORIENTED_EDGE('',*,*,#15651,.T.);
#21780=ORIENTED_EDGE('',*,*,#15842,.T.);
#21781=ORIENTED_EDGE('',*,*,#15819,.T.);
#21782=ORIENTED_EDGE('',*,*,#15820,.T.);
#21783=ORIENTED_EDGE('',*,*,#15843,.T.);
#21784=ORIENTED_EDGE('',*,*,#15642,.T.);
#21785=ORIENTED_EDGE('',*,*,#15643,.T.);
#21786=ORIENTED_EDGE('',*,*,#15844,.T.);
#21787=ORIENTED_EDGE('',*,*,#15827,.T.);
#21788=ORIENTED_EDGE('',*,*,#15828,.T.);
#21789=ORIENTED_EDGE('',*,*,#15845,.T.);
#21790=ORIENTED_EDGE('',*,*,#15779,.T.);
#21791=ORIENTED_EDGE('',*,*,#15780,.T.);
#21792=ORIENTED_EDGE('',*,*,#15846,.T.);
#21793=ORIENTED_EDGE('',*,*,#15731,.T.);
#21794=ORIENTED_EDGE('',*,*,#15732,.T.);
#21795=ORIENTED_EDGE('',*,*,#15847,.T.);
#21796=ORIENTED_EDGE('',*,*,#15739,.T.);
#21797=ORIENTED_EDGE('',*,*,#15740,.T.);
#21798=ORIENTED_EDGE('',*,*,#15848,.T.);
#21799=ORIENTED_EDGE('',*,*,#15723,.T.);
#21800=ORIENTED_EDGE('',*,*,#15724,.T.);
#21801=ORIENTED_EDGE('',*,*,#15849,.T.);
#21802=ORIENTED_EDGE('',*,*,#15747,.T.);
#21803=ORIENTED_EDGE('',*,*,#15748,.T.);
#21804=ORIENTED_EDGE('',*,*,#15850,.T.);
#21805=ORIENTED_EDGE('',*,*,#15715,.T.);
#21806=ORIENTED_EDGE('',*,*,#15716,.T.);
#21807=ORIENTED_EDGE('',*,*,#15851,.T.);
#21808=ORIENTED_EDGE('',*,*,#15755,.T.);
#21809=ORIENTED_EDGE('',*,*,#15756,.T.);
#21810=ORIENTED_EDGE('',*,*,#15852,.T.);
#21811=ORIENTED_EDGE('',*,*,#15707,.T.);
#21812=ORIENTED_EDGE('',*,*,#15708,.T.);
#21813=ORIENTED_EDGE('',*,*,#15853,.T.);
#21814=ORIENTED_EDGE('',*,*,#15763,.T.);
#21815=ORIENTED_EDGE('',*,*,#15764,.T.);
#21816=ORIENTED_EDGE('',*,*,#15854,.T.);
#21817=ORIENTED_EDGE('',*,*,#15699,.T.);
#21818=ORIENTED_EDGE('',*,*,#15700,.T.);
#21819=ORIENTED_EDGE('',*,*,#15855,.T.);
#21820=ORIENTED_EDGE('',*,*,#15771,.T.);
#21821=ORIENTED_EDGE('',*,*,#15772,.T.);
#21822=ORIENTED_EDGE('',*,*,#15856,.T.);
#21823=ORIENTED_EDGE('',*,*,#15691,.T.);
#21824=ORIENTED_EDGE('',*,*,#15692,.T.);
#21825=ORIENTED_EDGE('',*,*,#15857,.T.);
#21826=ORIENTED_EDGE('',*,*,#15682,.T.);
#21827=ORIENTED_EDGE('',*,*,#15833,.F.);
#21828=ORIENTED_EDGE('',*,*,#15776,.T.);
#21829=ORIENTED_EDGE('',*,*,#15845,.F.);
#21830=ORIENTED_EDGE('',*,*,#15830,.T.);
#21831=ORIENTED_EDGE('',*,*,#15858,.T.);
#21832=ORIENTED_EDGE('',*,*,#15734,.T.);
#21833=ORIENTED_EDGE('',*,*,#15859,.T.);
#21834=ORIENTED_EDGE('',*,*,#15736,.T.);
#21835=ORIENTED_EDGE('',*,*,#15847,.F.);
#21836=ORIENTED_EDGE('',*,*,#15728,.T.);
#21837=ORIENTED_EDGE('',*,*,#15846,.F.);
#21838=ORIENTED_EDGE('',*,*,#15782,.T.);
#21839=ORIENTED_EDGE('',*,*,#15860,.T.);
#21840=ORIENTED_EDGE('',*,*,#15726,.T.);
#21841=ORIENTED_EDGE('',*,*,#15861,.T.);
#21842=ORIENTED_EDGE('',*,*,#15744,.T.);
#21843=ORIENTED_EDGE('',*,*,#15849,.F.);
#21844=ORIENTED_EDGE('',*,*,#15720,.T.);
#21845=ORIENTED_EDGE('',*,*,#15848,.F.);
#21846=ORIENTED_EDGE('',*,*,#15742,.T.);
#21847=ORIENTED_EDGE('',*,*,#15862,.T.);
#21848=ORIENTED_EDGE('',*,*,#15718,.T.);
#21849=ORIENTED_EDGE('',*,*,#15863,.T.);
#21850=ORIENTED_EDGE('',*,*,#15752,.T.);
#21851=ORIENTED_EDGE('',*,*,#15851,.F.);
#21852=ORIENTED_EDGE('',*,*,#15712,.T.);
#21853=ORIENTED_EDGE('',*,*,#15850,.F.);
#21854=ORIENTED_EDGE('',*,*,#15750,.T.);
#21855=ORIENTED_EDGE('',*,*,#15864,.T.);
#21856=ORIENTED_EDGE('',*,*,#15710,.T.);
#21857=ORIENTED_EDGE('',*,*,#15865,.T.);
#21858=ORIENTED_EDGE('',*,*,#15760,.T.);
#21859=ORIENTED_EDGE('',*,*,#15853,.F.);
#21860=ORIENTED_EDGE('',*,*,#15704,.T.);
#21861=ORIENTED_EDGE('',*,*,#15852,.F.);
#21862=ORIENTED_EDGE('',*,*,#15758,.T.);
#21863=ORIENTED_EDGE('',*,*,#15866,.T.);
#21864=ORIENTED_EDGE('',*,*,#15702,.T.);
#21865=ORIENTED_EDGE('',*,*,#15867,.T.);
#21866=ORIENTED_EDGE('',*,*,#15768,.T.);
#21867=ORIENTED_EDGE('',*,*,#15855,.F.);
#21868=ORIENTED_EDGE('',*,*,#15696,.T.);
#21869=ORIENTED_EDGE('',*,*,#15854,.F.);
#21870=ORIENTED_EDGE('',*,*,#15766,.T.);
#21871=ORIENTED_EDGE('',*,*,#15868,.T.);
#21872=ORIENTED_EDGE('',*,*,#15688,.T.);
#21873=ORIENTED_EDGE('',*,*,#15856,.F.);
#21874=ORIENTED_EDGE('',*,*,#15774,.T.);
#21875=ORIENTED_EDGE('',*,*,#15869,.T.);
#21876=ORIENTED_EDGE('',*,*,#15685,.T.);
#21877=ORIENTED_EDGE('',*,*,#15870,.T.);
#21878=ORIENTED_EDGE('',*,*,#15784,.T.);
#21879=ORIENTED_EDGE('',*,*,#15834,.F.);
#21880=ORIENTED_EDGE('',*,*,#15679,.T.);
#21881=ORIENTED_EDGE('',*,*,#15857,.F.);
#21882=ORIENTED_EDGE('',*,*,#15694,.T.);
#21883=ORIENTED_EDGE('',*,*,#15871,.T.);
#21884=ORIENTED_EDGE('',*,*,#15677,.T.);
#21885=ORIENTED_EDGE('',*,*,#15872,.T.);
#21886=ORIENTED_EDGE('',*,*,#15792,.T.);
#21887=ORIENTED_EDGE('',*,*,#15836,.F.);
#21888=ORIENTED_EDGE('',*,*,#15671,.T.);
#21889=ORIENTED_EDGE('',*,*,#15835,.F.);
#21890=ORIENTED_EDGE('',*,*,#15790,.T.);
#21891=ORIENTED_EDGE('',*,*,#15873,.T.);
#21892=ORIENTED_EDGE('',*,*,#15669,.T.);
#21893=ORIENTED_EDGE('',*,*,#15874,.T.);
#21894=ORIENTED_EDGE('',*,*,#15800,.T.);
#21895=ORIENTED_EDGE('',*,*,#15838,.F.);
#21896=ORIENTED_EDGE('',*,*,#15663,.T.);
#21897=ORIENTED_EDGE('',*,*,#15837,.F.);
#21898=ORIENTED_EDGE('',*,*,#15798,.T.);
#21899=ORIENTED_EDGE('',*,*,#15875,.T.);
#21900=ORIENTED_EDGE('',*,*,#15661,.T.);
#21901=ORIENTED_EDGE('',*,*,#15876,.T.);
#21902=ORIENTED_EDGE('',*,*,#15808,.T.);
#21903=ORIENTED_EDGE('',*,*,#15840,.F.);
#21904=ORIENTED_EDGE('',*,*,#15655,.T.);
#21905=ORIENTED_EDGE('',*,*,#15839,.F.);
#21906=ORIENTED_EDGE('',*,*,#15806,.T.);
#21907=ORIENTED_EDGE('',*,*,#15877,.T.);
#21908=ORIENTED_EDGE('',*,*,#15653,.T.);
#21909=ORIENTED_EDGE('',*,*,#15878,.T.);
#21910=ORIENTED_EDGE('',*,*,#15816,.T.);
#21911=ORIENTED_EDGE('',*,*,#15842,.F.);
#21912=ORIENTED_EDGE('',*,*,#15647,.T.);
#21913=ORIENTED_EDGE('',*,*,#15841,.F.);
#21914=ORIENTED_EDGE('',*,*,#15814,.T.);
#21915=ORIENTED_EDGE('',*,*,#15879,.T.);
#21916=ORIENTED_EDGE('',*,*,#15645,.T.);
#21917=ORIENTED_EDGE('',*,*,#15880,.T.);
#21918=ORIENTED_EDGE('',*,*,#15824,.T.);
#21919=ORIENTED_EDGE('',*,*,#15844,.F.);
#21920=ORIENTED_EDGE('',*,*,#15881,.F.);
#21921=ORIENTED_EDGE('',*,*,#15882,.F.);
#21922=ORIENTED_EDGE('',*,*,#15625,.F.);
#21923=ORIENTED_EDGE('',*,*,#15621,.F.);
#21924=ORIENTED_EDGE('',*,*,#15618,.F.);
#21925=ORIENTED_EDGE('',*,*,#15615,.F.);
#21926=ORIENTED_EDGE('',*,*,#15612,.F.);
#21927=ORIENTED_EDGE('',*,*,#15883,.F.);
#21928=ORIENTED_EDGE('',*,*,#15884,.T.);
#21929=ORIENTED_EDGE('',*,*,#15638,.T.);
#21930=ORIENTED_EDGE('',*,*,#15635,.T.);
#21931=ORIENTED_EDGE('',*,*,#15632,.T.);
#21932=ORIENTED_EDGE('',*,*,#15629,.T.);
#21933=ORIENTED_EDGE('',*,*,#15636,.T.);
#21934=ORIENTED_EDGE('',*,*,#15884,.F.);
#21935=ORIENTED_EDGE('',*,*,#15885,.F.);
#21936=ORIENTED_EDGE('',*,*,#15886,.T.);
#21937=ORIENTED_EDGE('',*,*,#15887,.F.);
#21938=ORIENTED_EDGE('',*,*,#15627,.F.);
#21939=ORIENTED_EDGE('',*,*,#15631,.F.);
#21940=ORIENTED_EDGE('',*,*,#15634,.F.);
#21941=ORIENTED_EDGE('',*,*,#15637,.F.);
#21942=ORIENTED_EDGE('',*,*,#15886,.F.);
#21943=ORIENTED_EDGE('',*,*,#15888,.F.);
#21944=ORIENTED_EDGE('',*,*,#15610,.F.);
#21945=ORIENTED_EDGE('',*,*,#15614,.F.);
#21946=ORIENTED_EDGE('',*,*,#15617,.F.);
#21947=ORIENTED_EDGE('',*,*,#15620,.F.);
#21948=ORIENTED_EDGE('',*,*,#15624,.F.);
#21949=ORIENTED_EDGE('',*,*,#15622,.T.);
#21950=ORIENTED_EDGE('',*,*,#15882,.T.);
#21951=ORIENTED_EDGE('',*,*,#15889,.F.);
#21952=ORIENTED_EDGE('',*,*,#15890,.F.);
#21953=ORIENTED_EDGE('',*,*,#15891,.F.);
#21954=ORIENTED_EDGE('',*,*,#15892,.T.);
#21955=ORIENTED_EDGE('',*,*,#15890,.T.);
#21956=ORIENTED_EDGE('',*,*,#15892,.F.);
#21957=ORIENTED_EDGE('',*,*,#15893,.F.);
#21958=ORIENTED_EDGE('',*,*,#15894,.T.);
#21959=ORIENTED_EDGE('',*,*,#15891,.T.);
#21960=ORIENTED_EDGE('',*,*,#15894,.F.);
#21961=ORIENTED_EDGE('',*,*,#15895,.F.);
#21962=ORIENTED_EDGE('',*,*,#15896,.T.);
#21963=ORIENTED_EDGE('',*,*,#15893,.T.);
#21964=ORIENTED_EDGE('',*,*,#15896,.F.);
#21965=ORIENTED_EDGE('',*,*,#15895,.T.);
#21966=ORIENTED_EDGE('',*,*,#15888,.T.);
#21967=ORIENTED_EDGE('',*,*,#15885,.T.);
#21968=ORIENTED_EDGE('',*,*,#15883,.T.);
#21969=ORIENTED_EDGE('',*,*,#15611,.F.);
#21970=ORIENTED_EDGE('',*,*,#15897,.F.);
#21971=ORIENTED_EDGE('',*,*,#15623,.T.);
#21972=ORIENTED_EDGE('',*,*,#15889,.T.);
#21973=ORIENTED_EDGE('',*,*,#15881,.T.);
#21974=ORIENTED_EDGE('',*,*,#15628,.T.);
#21975=ORIENTED_EDGE('',*,*,#15887,.T.);
#21976=ORIENTED_EDGE('',*,*,#15783,.F.);
#21977=ORIENTED_EDGE('',*,*,#15858,.F.);
#21978=ORIENTED_EDGE('',*,*,#15831,.F.);
#21979=ORIENTED_EDGE('',*,*,#15880,.F.);
#21980=ORIENTED_EDGE('',*,*,#15646,.F.);
#21981=ORIENTED_EDGE('',*,*,#15898,.F.);
#21982=ORIENTED_EDGE('',*,*,#15823,.F.);
#21983=ORIENTED_EDGE('',*,*,#15878,.F.);
#21984=ORIENTED_EDGE('',*,*,#15654,.F.);
#21985=ORIENTED_EDGE('',*,*,#15879,.F.);
#21986=ORIENTED_EDGE('',*,*,#15815,.F.);
#21987=ORIENTED_EDGE('',*,*,#15876,.F.);
#21988=ORIENTED_EDGE('',*,*,#15662,.F.);
#21989=ORIENTED_EDGE('',*,*,#15877,.F.);
#21990=ORIENTED_EDGE('',*,*,#15807,.F.);
#21991=ORIENTED_EDGE('',*,*,#15874,.F.);
#21992=ORIENTED_EDGE('',*,*,#15670,.F.);
#21993=ORIENTED_EDGE('',*,*,#15875,.F.);
#21994=ORIENTED_EDGE('',*,*,#15799,.F.);
#21995=ORIENTED_EDGE('',*,*,#15872,.F.);
#21996=ORIENTED_EDGE('',*,*,#15678,.F.);
#21997=ORIENTED_EDGE('',*,*,#15873,.F.);
#21998=ORIENTED_EDGE('',*,*,#15791,.F.);
#21999=ORIENTED_EDGE('',*,*,#15870,.F.);
#22000=ORIENTED_EDGE('',*,*,#15687,.F.);
#22001=ORIENTED_EDGE('',*,*,#15899,.T.);
#22002=ORIENTED_EDGE('',*,*,#15897,.T.);
#22003=ORIENTED_EDGE('',*,*,#15899,.F.);
#22004=ORIENTED_EDGE('',*,*,#15686,.F.);
#22005=ORIENTED_EDGE('',*,*,#15871,.F.);
#22006=ORIENTED_EDGE('',*,*,#15695,.F.);
#22007=ORIENTED_EDGE('',*,*,#15869,.F.);
#22008=ORIENTED_EDGE('',*,*,#15775,.F.);
#22009=ORIENTED_EDGE('',*,*,#15867,.F.);
#22010=ORIENTED_EDGE('',*,*,#15703,.F.);
#22011=ORIENTED_EDGE('',*,*,#15868,.F.);
#22012=ORIENTED_EDGE('',*,*,#15767,.F.);
#22013=ORIENTED_EDGE('',*,*,#15865,.F.);
#22014=ORIENTED_EDGE('',*,*,#15711,.F.);
#22015=ORIENTED_EDGE('',*,*,#15866,.F.);
#22016=ORIENTED_EDGE('',*,*,#15759,.F.);
#22017=ORIENTED_EDGE('',*,*,#15863,.F.);
#22018=ORIENTED_EDGE('',*,*,#15719,.F.);
#22019=ORIENTED_EDGE('',*,*,#15864,.F.);
#22020=ORIENTED_EDGE('',*,*,#15751,.F.);
#22021=ORIENTED_EDGE('',*,*,#15861,.F.);
#22022=ORIENTED_EDGE('',*,*,#15727,.F.);
#22023=ORIENTED_EDGE('',*,*,#15862,.F.);
#22024=ORIENTED_EDGE('',*,*,#15743,.F.);
#22025=ORIENTED_EDGE('',*,*,#15859,.F.);
#22026=ORIENTED_EDGE('',*,*,#15735,.F.);
#22027=ORIENTED_EDGE('',*,*,#15860,.F.);
#22028=ORIENTED_EDGE('',*,*,#15639,.T.);
#22029=ORIENTED_EDGE('',*,*,#15843,.F.);
#22030=ORIENTED_EDGE('',*,*,#15822,.T.);
#22031=ORIENTED_EDGE('',*,*,#15898,.T.);
#22032=ORIENTED_EDGE('',*,*,#15832,.T.);
#22033=ORIENTED_EDGE('',*,*,#15900,.F.);
#22034=ORIENTED_EDGE('',*,*,#15901,.T.);
#22035=ORIENTED_EDGE('',*,*,#15902,.T.);
#22036=ORIENTED_EDGE('',*,*,#15903,.T.);
#22037=ORIENTED_EDGE('',*,*,#15904,.F.);
#22038=ORIENTED_EDGE('',*,*,#15905,.T.);
#22039=ORIENTED_EDGE('',*,*,#15900,.T.);
#22040=ORIENTED_EDGE('',*,*,#15906,.T.);
#22041=ORIENTED_EDGE('',*,*,#15907,.F.);
#22042=ORIENTED_EDGE('',*,*,#15908,.T.);
#22043=ORIENTED_EDGE('',*,*,#15904,.T.);
#22044=ORIENTED_EDGE('',*,*,#15909,.T.);
#22045=ORIENTED_EDGE('',*,*,#15910,.F.);
#22046=ORIENTED_EDGE('',*,*,#15911,.T.);
#22047=ORIENTED_EDGE('',*,*,#15907,.T.);
#22048=ORIENTED_EDGE('',*,*,#15912,.T.);
#22049=ORIENTED_EDGE('',*,*,#15913,.F.);
#22050=ORIENTED_EDGE('',*,*,#15914,.T.);
#22051=ORIENTED_EDGE('',*,*,#15910,.T.);
#22052=ORIENTED_EDGE('',*,*,#15915,.T.);
#22053=ORIENTED_EDGE('',*,*,#15916,.F.);
#22054=ORIENTED_EDGE('',*,*,#15917,.T.);
#22055=ORIENTED_EDGE('',*,*,#15913,.T.);
#22056=ORIENTED_EDGE('',*,*,#15918,.T.);
#22057=ORIENTED_EDGE('',*,*,#15919,.F.);
#22058=ORIENTED_EDGE('',*,*,#15920,.T.);
#22059=ORIENTED_EDGE('',*,*,#15916,.T.);
#22060=ORIENTED_EDGE('',*,*,#15921,.T.);
#22061=ORIENTED_EDGE('',*,*,#15922,.F.);
#22062=ORIENTED_EDGE('',*,*,#15923,.T.);
#22063=ORIENTED_EDGE('',*,*,#15919,.T.);
#22064=ORIENTED_EDGE('',*,*,#15924,.T.);
#22065=ORIENTED_EDGE('',*,*,#15925,.F.);
#22066=ORIENTED_EDGE('',*,*,#15926,.T.);
#22067=ORIENTED_EDGE('',*,*,#15922,.T.);
#22068=ORIENTED_EDGE('',*,*,#15927,.T.);
#22069=ORIENTED_EDGE('',*,*,#15928,.F.);
#22070=ORIENTED_EDGE('',*,*,#15929,.T.);
#22071=ORIENTED_EDGE('',*,*,#15925,.T.);
#22072=ORIENTED_EDGE('',*,*,#15930,.T.);
#22073=ORIENTED_EDGE('',*,*,#15931,.F.);
#22074=ORIENTED_EDGE('',*,*,#15932,.T.);
#22075=ORIENTED_EDGE('',*,*,#15928,.T.);
#22076=ORIENTED_EDGE('',*,*,#15933,.T.);
#22077=ORIENTED_EDGE('',*,*,#15934,.F.);
#22078=ORIENTED_EDGE('',*,*,#15935,.T.);
#22079=ORIENTED_EDGE('',*,*,#15931,.T.);
#22080=ORIENTED_EDGE('',*,*,#15936,.T.);
#22081=ORIENTED_EDGE('',*,*,#15937,.F.);
#22082=ORIENTED_EDGE('',*,*,#15938,.T.);
#22083=ORIENTED_EDGE('',*,*,#15934,.T.);
#22084=ORIENTED_EDGE('',*,*,#15939,.T.);
#22085=ORIENTED_EDGE('',*,*,#15940,.F.);
#22086=ORIENTED_EDGE('',*,*,#15941,.T.);
#22087=ORIENTED_EDGE('',*,*,#15937,.T.);
#22088=ORIENTED_EDGE('',*,*,#15942,.T.);
#22089=ORIENTED_EDGE('',*,*,#15943,.F.);
#22090=ORIENTED_EDGE('',*,*,#15944,.T.);
#22091=ORIENTED_EDGE('',*,*,#15940,.T.);
#22092=ORIENTED_EDGE('',*,*,#15945,.T.);
#22093=ORIENTED_EDGE('',*,*,#15946,.F.);
#22094=ORIENTED_EDGE('',*,*,#15947,.T.);
#22095=ORIENTED_EDGE('',*,*,#15948,.F.);
#22096=ORIENTED_EDGE('',*,*,#15949,.F.);
#22097=ORIENTED_EDGE('',*,*,#15950,.F.);
#22098=ORIENTED_EDGE('',*,*,#15951,.T.);
#22099=ORIENTED_EDGE('',*,*,#15946,.T.);
#22100=ORIENTED_EDGE('',*,*,#15952,.F.);
#22101=ORIENTED_EDGE('',*,*,#15953,.F.);
#22102=ORIENTED_EDGE('',*,*,#15954,.T.);
#22103=ORIENTED_EDGE('',*,*,#15950,.T.);
#22104=ORIENTED_EDGE('',*,*,#15955,.F.);
#22105=ORIENTED_EDGE('',*,*,#15956,.F.);
#22106=ORIENTED_EDGE('',*,*,#15957,.T.);
#22107=ORIENTED_EDGE('',*,*,#15953,.T.);
#22108=ORIENTED_EDGE('',*,*,#15958,.F.);
#22109=ORIENTED_EDGE('',*,*,#15959,.F.);
#22110=ORIENTED_EDGE('',*,*,#15960,.T.);
#22111=ORIENTED_EDGE('',*,*,#15956,.T.);
#22112=ORIENTED_EDGE('',*,*,#15961,.F.);
#22113=ORIENTED_EDGE('',*,*,#15962,.F.);
#22114=ORIENTED_EDGE('',*,*,#15963,.T.);
#22115=ORIENTED_EDGE('',*,*,#15959,.T.);
#22116=ORIENTED_EDGE('',*,*,#15964,.F.);
#22117=ORIENTED_EDGE('',*,*,#15965,.F.);
#22118=ORIENTED_EDGE('',*,*,#15966,.T.);
#22119=ORIENTED_EDGE('',*,*,#15962,.T.);
#22120=ORIENTED_EDGE('',*,*,#15967,.F.);
#22121=ORIENTED_EDGE('',*,*,#15968,.F.);
#22122=ORIENTED_EDGE('',*,*,#15969,.T.);
#22123=ORIENTED_EDGE('',*,*,#15965,.T.);
#22124=ORIENTED_EDGE('',*,*,#15970,.F.);
#22125=ORIENTED_EDGE('',*,*,#15971,.F.);
#22126=ORIENTED_EDGE('',*,*,#15972,.T.);
#22127=ORIENTED_EDGE('',*,*,#15968,.T.);
#22128=ORIENTED_EDGE('',*,*,#15973,.F.);
#22129=ORIENTED_EDGE('',*,*,#15974,.F.);
#22130=ORIENTED_EDGE('',*,*,#15975,.T.);
#22131=ORIENTED_EDGE('',*,*,#15971,.T.);
#22132=ORIENTED_EDGE('',*,*,#15976,.F.);
#22133=ORIENTED_EDGE('',*,*,#15977,.F.);
#22134=ORIENTED_EDGE('',*,*,#15978,.T.);
#22135=ORIENTED_EDGE('',*,*,#15974,.T.);
#22136=ORIENTED_EDGE('',*,*,#15979,.F.);
#22137=ORIENTED_EDGE('',*,*,#15980,.F.);
#22138=ORIENTED_EDGE('',*,*,#15981,.T.);
#22139=ORIENTED_EDGE('',*,*,#15977,.T.);
#22140=ORIENTED_EDGE('',*,*,#15982,.F.);
#22141=ORIENTED_EDGE('',*,*,#15983,.F.);
#22142=ORIENTED_EDGE('',*,*,#15984,.T.);
#22143=ORIENTED_EDGE('',*,*,#15980,.T.);
#22144=ORIENTED_EDGE('',*,*,#15985,.F.);
#22145=ORIENTED_EDGE('',*,*,#15986,.F.);
#22146=ORIENTED_EDGE('',*,*,#15987,.T.);
#22147=ORIENTED_EDGE('',*,*,#15983,.T.);
#22148=ORIENTED_EDGE('',*,*,#15988,.F.);
#22149=ORIENTED_EDGE('',*,*,#15989,.F.);
#22150=ORIENTED_EDGE('',*,*,#15990,.T.);
#22151=ORIENTED_EDGE('',*,*,#15986,.T.);
#22152=ORIENTED_EDGE('',*,*,#15991,.F.);
#22153=ORIENTED_EDGE('',*,*,#15992,.F.);
#22154=ORIENTED_EDGE('',*,*,#15993,.T.);
#22155=ORIENTED_EDGE('',*,*,#15994,.T.);
#22156=ORIENTED_EDGE('',*,*,#15995,.F.);
#22157=ORIENTED_EDGE('',*,*,#15996,.F.);
#22158=ORIENTED_EDGE('',*,*,#15994,.F.);
#22159=ORIENTED_EDGE('',*,*,#15997,.F.);
#22160=ORIENTED_EDGE('',*,*,#15998,.F.);
#22161=ORIENTED_EDGE('',*,*,#15999,.F.);
#22162=ORIENTED_EDGE('',*,*,#15997,.T.);
#22163=ORIENTED_EDGE('',*,*,#15993,.F.);
#22164=ORIENTED_EDGE('',*,*,#16000,.F.);
#22165=ORIENTED_EDGE('',*,*,#16001,.T.);
#22166=ORIENTED_EDGE('',*,*,#16002,.T.);
#22167=ORIENTED_EDGE('',*,*,#16003,.F.);
#22168=ORIENTED_EDGE('',*,*,#16004,.F.);
#22169=ORIENTED_EDGE('',*,*,#16002,.F.);
#22170=ORIENTED_EDGE('',*,*,#16005,.F.);
#22171=ORIENTED_EDGE('',*,*,#16006,.F.);
#22172=ORIENTED_EDGE('',*,*,#16007,.F.);
#22173=ORIENTED_EDGE('',*,*,#16005,.T.);
#22174=ORIENTED_EDGE('',*,*,#16001,.F.);
#22175=ORIENTED_EDGE('',*,*,#16008,.F.);
#22176=ORIENTED_EDGE('',*,*,#16009,.T.);
#22177=ORIENTED_EDGE('',*,*,#16010,.T.);
#22178=ORIENTED_EDGE('',*,*,#16011,.F.);
#22179=ORIENTED_EDGE('',*,*,#16012,.F.);
#22180=ORIENTED_EDGE('',*,*,#16010,.F.);
#22181=ORIENTED_EDGE('',*,*,#16013,.F.);
#22182=ORIENTED_EDGE('',*,*,#16014,.F.);
#22183=ORIENTED_EDGE('',*,*,#16015,.F.);
#22184=ORIENTED_EDGE('',*,*,#16013,.T.);
#22185=ORIENTED_EDGE('',*,*,#16009,.F.);
#22186=ORIENTED_EDGE('',*,*,#16016,.F.);
#22187=ORIENTED_EDGE('',*,*,#16017,.T.);
#22188=ORIENTED_EDGE('',*,*,#16018,.T.);
#22189=ORIENTED_EDGE('',*,*,#16019,.F.);
#22190=ORIENTED_EDGE('',*,*,#16020,.F.);
#22191=ORIENTED_EDGE('',*,*,#16018,.F.);
#22192=ORIENTED_EDGE('',*,*,#16021,.F.);
#22193=ORIENTED_EDGE('',*,*,#16022,.F.);
#22194=ORIENTED_EDGE('',*,*,#16023,.F.);
#22195=ORIENTED_EDGE('',*,*,#16021,.T.);
#22196=ORIENTED_EDGE('',*,*,#16017,.F.);
#22197=ORIENTED_EDGE('',*,*,#16024,.F.);
#22198=ORIENTED_EDGE('',*,*,#16025,.T.);
#22199=ORIENTED_EDGE('',*,*,#16026,.T.);
#22200=ORIENTED_EDGE('',*,*,#16027,.F.);
#22201=ORIENTED_EDGE('',*,*,#16028,.F.);
#22202=ORIENTED_EDGE('',*,*,#16026,.F.);
#22203=ORIENTED_EDGE('',*,*,#16029,.F.);
#22204=ORIENTED_EDGE('',*,*,#16030,.F.);
#22205=ORIENTED_EDGE('',*,*,#16031,.F.);
#22206=ORIENTED_EDGE('',*,*,#16029,.T.);
#22207=ORIENTED_EDGE('',*,*,#16025,.F.);
#22208=ORIENTED_EDGE('',*,*,#16032,.F.);
#22209=ORIENTED_EDGE('',*,*,#16033,.T.);
#22210=ORIENTED_EDGE('',*,*,#16034,.T.);
#22211=ORIENTED_EDGE('',*,*,#16035,.F.);
#22212=ORIENTED_EDGE('',*,*,#16036,.F.);
#22213=ORIENTED_EDGE('',*,*,#16034,.F.);
#22214=ORIENTED_EDGE('',*,*,#16037,.F.);
#22215=ORIENTED_EDGE('',*,*,#16038,.F.);
#22216=ORIENTED_EDGE('',*,*,#16039,.F.);
#22217=ORIENTED_EDGE('',*,*,#16037,.T.);
#22218=ORIENTED_EDGE('',*,*,#16033,.F.);
#22219=ORIENTED_EDGE('',*,*,#16040,.F.);
#22220=ORIENTED_EDGE('',*,*,#16041,.T.);
#22221=ORIENTED_EDGE('',*,*,#16042,.T.);
#22222=ORIENTED_EDGE('',*,*,#16043,.F.);
#22223=ORIENTED_EDGE('',*,*,#16044,.F.);
#22224=ORIENTED_EDGE('',*,*,#16042,.F.);
#22225=ORIENTED_EDGE('',*,*,#16045,.F.);
#22226=ORIENTED_EDGE('',*,*,#16046,.F.);
#22227=ORIENTED_EDGE('',*,*,#16047,.F.);
#22228=ORIENTED_EDGE('',*,*,#16045,.T.);
#22229=ORIENTED_EDGE('',*,*,#16041,.F.);
#22230=ORIENTED_EDGE('',*,*,#16048,.F.);
#22231=ORIENTED_EDGE('',*,*,#16049,.T.);
#22232=ORIENTED_EDGE('',*,*,#16050,.T.);
#22233=ORIENTED_EDGE('',*,*,#16051,.F.);
#22234=ORIENTED_EDGE('',*,*,#16052,.F.);
#22235=ORIENTED_EDGE('',*,*,#16050,.F.);
#22236=ORIENTED_EDGE('',*,*,#16053,.F.);
#22237=ORIENTED_EDGE('',*,*,#16054,.F.);
#22238=ORIENTED_EDGE('',*,*,#16055,.F.);
#22239=ORIENTED_EDGE('',*,*,#16053,.T.);
#22240=ORIENTED_EDGE('',*,*,#16049,.F.);
#22241=ORIENTED_EDGE('',*,*,#16056,.F.);
#22242=ORIENTED_EDGE('',*,*,#16057,.T.);
#22243=ORIENTED_EDGE('',*,*,#16058,.T.);
#22244=ORIENTED_EDGE('',*,*,#16059,.F.);
#22245=ORIENTED_EDGE('',*,*,#16060,.F.);
#22246=ORIENTED_EDGE('',*,*,#16058,.F.);
#22247=ORIENTED_EDGE('',*,*,#16061,.F.);
#22248=ORIENTED_EDGE('',*,*,#16062,.F.);
#22249=ORIENTED_EDGE('',*,*,#16063,.F.);
#22250=ORIENTED_EDGE('',*,*,#16061,.T.);
#22251=ORIENTED_EDGE('',*,*,#16057,.F.);
#22252=ORIENTED_EDGE('',*,*,#16064,.F.);
#22253=ORIENTED_EDGE('',*,*,#16065,.T.);
#22254=ORIENTED_EDGE('',*,*,#16066,.T.);
#22255=ORIENTED_EDGE('',*,*,#16067,.F.);
#22256=ORIENTED_EDGE('',*,*,#16068,.F.);
#22257=ORIENTED_EDGE('',*,*,#16066,.F.);
#22258=ORIENTED_EDGE('',*,*,#16069,.F.);
#22259=ORIENTED_EDGE('',*,*,#16070,.F.);
#22260=ORIENTED_EDGE('',*,*,#16071,.F.);
#22261=ORIENTED_EDGE('',*,*,#16069,.T.);
#22262=ORIENTED_EDGE('',*,*,#16065,.F.);
#22263=ORIENTED_EDGE('',*,*,#16072,.F.);
#22264=ORIENTED_EDGE('',*,*,#16073,.T.);
#22265=ORIENTED_EDGE('',*,*,#16074,.T.);
#22266=ORIENTED_EDGE('',*,*,#16075,.F.);
#22267=ORIENTED_EDGE('',*,*,#16076,.F.);
#22268=ORIENTED_EDGE('',*,*,#16074,.F.);
#22269=ORIENTED_EDGE('',*,*,#16077,.F.);
#22270=ORIENTED_EDGE('',*,*,#16078,.F.);
#22271=ORIENTED_EDGE('',*,*,#16079,.F.);
#22272=ORIENTED_EDGE('',*,*,#16077,.T.);
#22273=ORIENTED_EDGE('',*,*,#16073,.F.);
#22274=ORIENTED_EDGE('',*,*,#16080,.F.);
#22275=ORIENTED_EDGE('',*,*,#16081,.T.);
#22276=ORIENTED_EDGE('',*,*,#16082,.T.);
#22277=ORIENTED_EDGE('',*,*,#16083,.F.);
#22278=ORIENTED_EDGE('',*,*,#16084,.F.);
#22279=ORIENTED_EDGE('',*,*,#16082,.F.);
#22280=ORIENTED_EDGE('',*,*,#16085,.F.);
#22281=ORIENTED_EDGE('',*,*,#16086,.F.);
#22282=ORIENTED_EDGE('',*,*,#16087,.F.);
#22283=ORIENTED_EDGE('',*,*,#16085,.T.);
#22284=ORIENTED_EDGE('',*,*,#16081,.F.);
#22285=ORIENTED_EDGE('',*,*,#16088,.F.);
#22286=ORIENTED_EDGE('',*,*,#16089,.T.);
#22287=ORIENTED_EDGE('',*,*,#16090,.T.);
#22288=ORIENTED_EDGE('',*,*,#16091,.F.);
#22289=ORIENTED_EDGE('',*,*,#16092,.F.);
#22290=ORIENTED_EDGE('',*,*,#16090,.F.);
#22291=ORIENTED_EDGE('',*,*,#16093,.F.);
#22292=ORIENTED_EDGE('',*,*,#16094,.F.);
#22293=ORIENTED_EDGE('',*,*,#16095,.F.);
#22294=ORIENTED_EDGE('',*,*,#16093,.T.);
#22295=ORIENTED_EDGE('',*,*,#16089,.F.);
#22296=ORIENTED_EDGE('',*,*,#16096,.F.);
#22297=ORIENTED_EDGE('',*,*,#16097,.T.);
#22298=ORIENTED_EDGE('',*,*,#16098,.T.);
#22299=ORIENTED_EDGE('',*,*,#16099,.F.);
#22300=ORIENTED_EDGE('',*,*,#16100,.F.);
#22301=ORIENTED_EDGE('',*,*,#16098,.F.);
#22302=ORIENTED_EDGE('',*,*,#16101,.F.);
#22303=ORIENTED_EDGE('',*,*,#16102,.F.);
#22304=ORIENTED_EDGE('',*,*,#16103,.F.);
#22305=ORIENTED_EDGE('',*,*,#16104,.F.);
#22306=ORIENTED_EDGE('',*,*,#16101,.T.);
#22307=ORIENTED_EDGE('',*,*,#16097,.F.);
#22308=ORIENTED_EDGE('',*,*,#16105,.F.);
#22309=ORIENTED_EDGE('',*,*,#16106,.T.);
#22310=ORIENTED_EDGE('',*,*,#16107,.T.);
#22311=ORIENTED_EDGE('',*,*,#16108,.F.);
#22312=ORIENTED_EDGE('',*,*,#16109,.F.);
#22313=ORIENTED_EDGE('',*,*,#16107,.F.);
#22314=ORIENTED_EDGE('',*,*,#16110,.F.);
#22315=ORIENTED_EDGE('',*,*,#16111,.F.);
#22316=ORIENTED_EDGE('',*,*,#16112,.F.);
#22317=ORIENTED_EDGE('',*,*,#16110,.T.);
#22318=ORIENTED_EDGE('',*,*,#16106,.F.);
#22319=ORIENTED_EDGE('',*,*,#16113,.F.);
#22320=ORIENTED_EDGE('',*,*,#16114,.T.);
#22321=ORIENTED_EDGE('',*,*,#16115,.T.);
#22322=ORIENTED_EDGE('',*,*,#16116,.F.);
#22323=ORIENTED_EDGE('',*,*,#16117,.F.);
#22324=ORIENTED_EDGE('',*,*,#16115,.F.);
#22325=ORIENTED_EDGE('',*,*,#16118,.F.);
#22326=ORIENTED_EDGE('',*,*,#16119,.F.);
#22327=ORIENTED_EDGE('',*,*,#16120,.F.);
#22328=ORIENTED_EDGE('',*,*,#16118,.T.);
#22329=ORIENTED_EDGE('',*,*,#16114,.F.);
#22330=ORIENTED_EDGE('',*,*,#16121,.F.);
#22331=ORIENTED_EDGE('',*,*,#16122,.T.);
#22332=ORIENTED_EDGE('',*,*,#16123,.T.);
#22333=ORIENTED_EDGE('',*,*,#16124,.F.);
#22334=ORIENTED_EDGE('',*,*,#16125,.F.);
#22335=ORIENTED_EDGE('',*,*,#16123,.F.);
#22336=ORIENTED_EDGE('',*,*,#16126,.F.);
#22337=ORIENTED_EDGE('',*,*,#16127,.F.);
#22338=ORIENTED_EDGE('',*,*,#16128,.F.);
#22339=ORIENTED_EDGE('',*,*,#16126,.T.);
#22340=ORIENTED_EDGE('',*,*,#16122,.F.);
#22341=ORIENTED_EDGE('',*,*,#16129,.F.);
#22342=ORIENTED_EDGE('',*,*,#16130,.T.);
#22343=ORIENTED_EDGE('',*,*,#16131,.T.);
#22344=ORIENTED_EDGE('',*,*,#16132,.F.);
#22345=ORIENTED_EDGE('',*,*,#16133,.F.);
#22346=ORIENTED_EDGE('',*,*,#16131,.F.);
#22347=ORIENTED_EDGE('',*,*,#16134,.F.);
#22348=ORIENTED_EDGE('',*,*,#16135,.F.);
#22349=ORIENTED_EDGE('',*,*,#16136,.F.);
#22350=ORIENTED_EDGE('',*,*,#16134,.T.);
#22351=ORIENTED_EDGE('',*,*,#16130,.F.);
#22352=ORIENTED_EDGE('',*,*,#15995,.T.);
#22353=ORIENTED_EDGE('',*,*,#15996,.T.);
#22354=ORIENTED_EDGE('',*,*,#15999,.T.);
#22355=ORIENTED_EDGE('',*,*,#16137,.F.);
#22356=ORIENTED_EDGE('',*,*,#16124,.T.);
#22357=ORIENTED_EDGE('',*,*,#16125,.T.);
#22358=ORIENTED_EDGE('',*,*,#16128,.T.);
#22359=ORIENTED_EDGE('',*,*,#16138,.F.);
#22360=ORIENTED_EDGE('',*,*,#16003,.T.);
#22361=ORIENTED_EDGE('',*,*,#16004,.T.);
#22362=ORIENTED_EDGE('',*,*,#16007,.T.);
#22363=ORIENTED_EDGE('',*,*,#16139,.F.);
#22364=ORIENTED_EDGE('',*,*,#16116,.T.);
#22365=ORIENTED_EDGE('',*,*,#16117,.T.);
#22366=ORIENTED_EDGE('',*,*,#16120,.T.);
#22367=ORIENTED_EDGE('',*,*,#16140,.F.);
#22368=ORIENTED_EDGE('',*,*,#16011,.T.);
#22369=ORIENTED_EDGE('',*,*,#16012,.T.);
#22370=ORIENTED_EDGE('',*,*,#16015,.T.);
#22371=ORIENTED_EDGE('',*,*,#16141,.F.);
#22372=ORIENTED_EDGE('',*,*,#16108,.T.);
#22373=ORIENTED_EDGE('',*,*,#16109,.T.);
#22374=ORIENTED_EDGE('',*,*,#16112,.T.);
#22375=ORIENTED_EDGE('',*,*,#16142,.F.);
#22376=ORIENTED_EDGE('',*,*,#16019,.T.);
#22377=ORIENTED_EDGE('',*,*,#16020,.T.);
#22378=ORIENTED_EDGE('',*,*,#16023,.T.);
#22379=ORIENTED_EDGE('',*,*,#16143,.F.);
#22380=ORIENTED_EDGE('',*,*,#16099,.T.);
#22381=ORIENTED_EDGE('',*,*,#16100,.T.);
#22382=ORIENTED_EDGE('',*,*,#16144,.T.);
#22383=ORIENTED_EDGE('',*,*,#16145,.T.);
#22384=ORIENTED_EDGE('',*,*,#16144,.F.);
#22385=ORIENTED_EDGE('',*,*,#16102,.T.);
#22386=ORIENTED_EDGE('',*,*,#16104,.T.);
#22387=ORIENTED_EDGE('',*,*,#16146,.F.);
#22388=ORIENTED_EDGE('',*,*,#16091,.T.);
#22389=ORIENTED_EDGE('',*,*,#16092,.T.);
#22390=ORIENTED_EDGE('',*,*,#16095,.T.);
#22391=ORIENTED_EDGE('',*,*,#16147,.F.);
#22392=ORIENTED_EDGE('',*,*,#16035,.T.);
#22393=ORIENTED_EDGE('',*,*,#16036,.T.);
#22394=ORIENTED_EDGE('',*,*,#16039,.T.);
#22395=ORIENTED_EDGE('',*,*,#16148,.F.);
#22396=ORIENTED_EDGE('',*,*,#16083,.T.);
#22397=ORIENTED_EDGE('',*,*,#16084,.T.);
#22398=ORIENTED_EDGE('',*,*,#16087,.T.);
#22399=ORIENTED_EDGE('',*,*,#16149,.F.);
#22400=ORIENTED_EDGE('',*,*,#16043,.T.);
#22401=ORIENTED_EDGE('',*,*,#16044,.T.);
#22402=ORIENTED_EDGE('',*,*,#16047,.T.);
#22403=ORIENTED_EDGE('',*,*,#16150,.F.);
#22404=ORIENTED_EDGE('',*,*,#16075,.T.);
#22405=ORIENTED_EDGE('',*,*,#16076,.T.);
#22406=ORIENTED_EDGE('',*,*,#16079,.T.);
#22407=ORIENTED_EDGE('',*,*,#16151,.F.);
#22408=ORIENTED_EDGE('',*,*,#16051,.T.);
#22409=ORIENTED_EDGE('',*,*,#16052,.T.);
#22410=ORIENTED_EDGE('',*,*,#16055,.T.);
#22411=ORIENTED_EDGE('',*,*,#16152,.F.);
#22412=ORIENTED_EDGE('',*,*,#16067,.T.);
#22413=ORIENTED_EDGE('',*,*,#16068,.T.);
#22414=ORIENTED_EDGE('',*,*,#16071,.T.);
#22415=ORIENTED_EDGE('',*,*,#16153,.F.);
#22416=ORIENTED_EDGE('',*,*,#16059,.T.);
#22417=ORIENTED_EDGE('',*,*,#16060,.T.);
#22418=ORIENTED_EDGE('',*,*,#16063,.T.);
#22419=ORIENTED_EDGE('',*,*,#16154,.F.);
#22420=ORIENTED_EDGE('',*,*,#16027,.T.);
#22421=ORIENTED_EDGE('',*,*,#16028,.T.);
#22422=ORIENTED_EDGE('',*,*,#16031,.T.);
#22423=ORIENTED_EDGE('',*,*,#16155,.F.);
#22424=ORIENTED_EDGE('',*,*,#16132,.T.);
#22425=ORIENTED_EDGE('',*,*,#16133,.T.);
#22426=ORIENTED_EDGE('',*,*,#16136,.T.);
#22427=ORIENTED_EDGE('',*,*,#16156,.F.);
#22428=ORIENTED_EDGE('',*,*,#16157,.F.);
#22429=ORIENTED_EDGE('',*,*,#16158,.F.);
#22430=ORIENTED_EDGE('',*,*,#15945,.F.);
#22431=ORIENTED_EDGE('',*,*,#15942,.F.);
#22432=ORIENTED_EDGE('',*,*,#15939,.F.);
#22433=ORIENTED_EDGE('',*,*,#15936,.F.);
#22434=ORIENTED_EDGE('',*,*,#15933,.F.);
#22435=ORIENTED_EDGE('',*,*,#15930,.F.);
#22436=ORIENTED_EDGE('',*,*,#15927,.F.);
#22437=ORIENTED_EDGE('',*,*,#15924,.F.);
#22438=ORIENTED_EDGE('',*,*,#15921,.F.);
#22439=ORIENTED_EDGE('',*,*,#15918,.F.);
#22440=ORIENTED_EDGE('',*,*,#15915,.F.);
#22441=ORIENTED_EDGE('',*,*,#15912,.F.);
#22442=ORIENTED_EDGE('',*,*,#15909,.F.);
#22443=ORIENTED_EDGE('',*,*,#15906,.F.);
#22444=ORIENTED_EDGE('',*,*,#15903,.F.);
#22445=ORIENTED_EDGE('',*,*,#16159,.F.);
#22446=ORIENTED_EDGE('',*,*,#16160,.T.);
#22447=ORIENTED_EDGE('',*,*,#15991,.T.);
#22448=ORIENTED_EDGE('',*,*,#15988,.T.);
#22449=ORIENTED_EDGE('',*,*,#15985,.T.);
#22450=ORIENTED_EDGE('',*,*,#15982,.T.);
#22451=ORIENTED_EDGE('',*,*,#15979,.T.);
#22452=ORIENTED_EDGE('',*,*,#15976,.T.);
#22453=ORIENTED_EDGE('',*,*,#15973,.T.);
#22454=ORIENTED_EDGE('',*,*,#15970,.T.);
#22455=ORIENTED_EDGE('',*,*,#15967,.T.);
#22456=ORIENTED_EDGE('',*,*,#15964,.T.);
#22457=ORIENTED_EDGE('',*,*,#15961,.T.);
#22458=ORIENTED_EDGE('',*,*,#15958,.T.);
#22459=ORIENTED_EDGE('',*,*,#15955,.T.);
#22460=ORIENTED_EDGE('',*,*,#15952,.T.);
#22461=ORIENTED_EDGE('',*,*,#15949,.T.);
#22462=ORIENTED_EDGE('',*,*,#16161,.T.);
#22463=ORIENTED_EDGE('',*,*,#16162,.T.);
#22464=ORIENTED_EDGE('',*,*,#16163,.T.);
#22465=ORIENTED_EDGE('',*,*,#16164,.T.);
#22466=ORIENTED_EDGE('',*,*,#16159,.T.);
#22467=ORIENTED_EDGE('',*,*,#15989,.T.);
#22468=ORIENTED_EDGE('',*,*,#16160,.F.);
#22469=ORIENTED_EDGE('',*,*,#16164,.F.);
#22470=ORIENTED_EDGE('',*,*,#16165,.T.);
#22471=ORIENTED_EDGE('',*,*,#16166,.F.);
#22472=ORIENTED_EDGE('',*,*,#15947,.F.);
#22473=ORIENTED_EDGE('',*,*,#15951,.F.);
#22474=ORIENTED_EDGE('',*,*,#15954,.F.);
#22475=ORIENTED_EDGE('',*,*,#15957,.F.);
#22476=ORIENTED_EDGE('',*,*,#15960,.F.);
#22477=ORIENTED_EDGE('',*,*,#15963,.F.);
#22478=ORIENTED_EDGE('',*,*,#15966,.F.);
#22479=ORIENTED_EDGE('',*,*,#15969,.F.);
#22480=ORIENTED_EDGE('',*,*,#15972,.F.);
#22481=ORIENTED_EDGE('',*,*,#15975,.F.);
#22482=ORIENTED_EDGE('',*,*,#15978,.F.);
#22483=ORIENTED_EDGE('',*,*,#15981,.F.);
#22484=ORIENTED_EDGE('',*,*,#15984,.F.);
#22485=ORIENTED_EDGE('',*,*,#15987,.F.);
#22486=ORIENTED_EDGE('',*,*,#15990,.F.);
#22487=ORIENTED_EDGE('',*,*,#16165,.F.);
#22488=ORIENTED_EDGE('',*,*,#16163,.F.);
#22489=ORIENTED_EDGE('',*,*,#15901,.F.);
#22490=ORIENTED_EDGE('',*,*,#15905,.F.);
#22491=ORIENTED_EDGE('',*,*,#15908,.F.);
#22492=ORIENTED_EDGE('',*,*,#15911,.F.);
#22493=ORIENTED_EDGE('',*,*,#15914,.F.);
#22494=ORIENTED_EDGE('',*,*,#15917,.F.);
#22495=ORIENTED_EDGE('',*,*,#15920,.F.);
#22496=ORIENTED_EDGE('',*,*,#15923,.F.);
#22497=ORIENTED_EDGE('',*,*,#15926,.F.);
#22498=ORIENTED_EDGE('',*,*,#15929,.F.);
#22499=ORIENTED_EDGE('',*,*,#15932,.F.);
#22500=ORIENTED_EDGE('',*,*,#15935,.F.);
#22501=ORIENTED_EDGE('',*,*,#15938,.F.);
#22502=ORIENTED_EDGE('',*,*,#15941,.F.);
#22503=ORIENTED_EDGE('',*,*,#15944,.F.);
#22504=ORIENTED_EDGE('',*,*,#16167,.F.);
#22505=ORIENTED_EDGE('',*,*,#16168,.F.);
#22506=ORIENTED_EDGE('',*,*,#16161,.F.);
#22507=ORIENTED_EDGE('',*,*,#15902,.F.);
#22508=ORIENTED_EDGE('',*,*,#16162,.F.);
#22509=ORIENTED_EDGE('',*,*,#16169,.T.);
#22510=ORIENTED_EDGE('',*,*,#16168,.T.);
#22511=ORIENTED_EDGE('',*,*,#16169,.F.);
#22512=ORIENTED_EDGE('',*,*,#15943,.T.);
#22513=ORIENTED_EDGE('',*,*,#16158,.T.);
#22514=ORIENTED_EDGE('',*,*,#16170,.F.);
#22515=ORIENTED_EDGE('',*,*,#16167,.T.);
#22516=ORIENTED_EDGE('',*,*,#16171,.F.);
#22517=ORIENTED_EDGE('',*,*,#16170,.T.);
#22518=ORIENTED_EDGE('',*,*,#16157,.T.);
#22519=ORIENTED_EDGE('',*,*,#15948,.T.);
#22520=ORIENTED_EDGE('',*,*,#16166,.T.);
#22521=ORIENTED_EDGE('',*,*,#16145,.F.);
#22522=ORIENTED_EDGE('',*,*,#16172,.T.);
#22523=ORIENTED_EDGE('',*,*,#16171,.T.);
#22524=ORIENTED_EDGE('',*,*,#16172,.F.);
#22525=ORIENTED_EDGE('',*,*,#16173,.F.);
#22526=ORIENTED_EDGE('',*,*,#16174,.T.);
#22527=ORIENTED_EDGE('',*,*,#16096,.T.);
#22528=ORIENTED_EDGE('',*,*,#16143,.T.);
#22529=ORIENTED_EDGE('',*,*,#16022,.T.);
#22530=ORIENTED_EDGE('',*,*,#16016,.T.);
#22531=ORIENTED_EDGE('',*,*,#16142,.T.);
#22532=ORIENTED_EDGE('',*,*,#16111,.T.);
#22533=ORIENTED_EDGE('',*,*,#16105,.T.);
#22534=ORIENTED_EDGE('',*,*,#16141,.T.);
#22535=ORIENTED_EDGE('',*,*,#16014,.T.);
#22536=ORIENTED_EDGE('',*,*,#16008,.T.);
#22537=ORIENTED_EDGE('',*,*,#16140,.T.);
#22538=ORIENTED_EDGE('',*,*,#16119,.T.);
#22539=ORIENTED_EDGE('',*,*,#16113,.T.);
#22540=ORIENTED_EDGE('',*,*,#16139,.T.);
#22541=ORIENTED_EDGE('',*,*,#16006,.T.);
#22542=ORIENTED_EDGE('',*,*,#16000,.T.);
#22543=ORIENTED_EDGE('',*,*,#16138,.T.);
#22544=ORIENTED_EDGE('',*,*,#16127,.T.);
#22545=ORIENTED_EDGE('',*,*,#16121,.T.);
#22546=ORIENTED_EDGE('',*,*,#16137,.T.);
#22547=ORIENTED_EDGE('',*,*,#15998,.T.);
#22548=ORIENTED_EDGE('',*,*,#15992,.T.);
#22549=ORIENTED_EDGE('',*,*,#16156,.T.);
#22550=ORIENTED_EDGE('',*,*,#16135,.T.);
#22551=ORIENTED_EDGE('',*,*,#16129,.T.);
#22552=ORIENTED_EDGE('',*,*,#16155,.T.);
#22553=ORIENTED_EDGE('',*,*,#16030,.T.);
#22554=ORIENTED_EDGE('',*,*,#16024,.T.);
#22555=ORIENTED_EDGE('',*,*,#16154,.T.);
#22556=ORIENTED_EDGE('',*,*,#16062,.T.);
#22557=ORIENTED_EDGE('',*,*,#16056,.T.);
#22558=ORIENTED_EDGE('',*,*,#16153,.T.);
#22559=ORIENTED_EDGE('',*,*,#16070,.T.);
#22560=ORIENTED_EDGE('',*,*,#16064,.T.);
#22561=ORIENTED_EDGE('',*,*,#16152,.T.);
#22562=ORIENTED_EDGE('',*,*,#16054,.T.);
#22563=ORIENTED_EDGE('',*,*,#16048,.T.);
#22564=ORIENTED_EDGE('',*,*,#16151,.T.);
#22565=ORIENTED_EDGE('',*,*,#16078,.T.);
#22566=ORIENTED_EDGE('',*,*,#16072,.T.);
#22567=ORIENTED_EDGE('',*,*,#16150,.T.);
#22568=ORIENTED_EDGE('',*,*,#16046,.T.);
#22569=ORIENTED_EDGE('',*,*,#16040,.T.);
#22570=ORIENTED_EDGE('',*,*,#16149,.T.);
#22571=ORIENTED_EDGE('',*,*,#16086,.T.);
#22572=ORIENTED_EDGE('',*,*,#16080,.T.);
#22573=ORIENTED_EDGE('',*,*,#16148,.T.);
#22574=ORIENTED_EDGE('',*,*,#16038,.T.);
#22575=ORIENTED_EDGE('',*,*,#16032,.T.);
#22576=ORIENTED_EDGE('',*,*,#16147,.T.);
#22577=ORIENTED_EDGE('',*,*,#16094,.T.);
#22578=ORIENTED_EDGE('',*,*,#16088,.T.);
#22579=ORIENTED_EDGE('',*,*,#16146,.T.);
#22580=ORIENTED_EDGE('',*,*,#16103,.T.);
#22581=ORIENTED_EDGE('',*,*,#16174,.F.);
#22582=ORIENTED_EDGE('',*,*,#16173,.T.);
#22583=ORIENTED_EDGE('',*,*,#16175,.F.);
#22584=ORIENTED_EDGE('',*,*,#16176,.T.);
#22585=ORIENTED_EDGE('',*,*,#16177,.T.);
#22586=ORIENTED_EDGE('',*,*,#16176,.F.);
#22587=ORIENTED_EDGE('',*,*,#16177,.F.);
#22588=ORIENTED_EDGE('',*,*,#16178,.T.);
#22589=ORIENTED_EDGE('',*,*,#16179,.T.);
#22590=ORIENTED_EDGE('',*,*,#16180,.T.);
#22591=ORIENTED_EDGE('',*,*,#16181,.T.);
#22592=ORIENTED_EDGE('',*,*,#16182,.T.);
#22593=ORIENTED_EDGE('',*,*,#16183,.T.);
#22594=ORIENTED_EDGE('',*,*,#16184,.F.);
#22595=ORIENTED_EDGE('',*,*,#16185,.T.);
#22596=ORIENTED_EDGE('',*,*,#16186,.T.);
#22597=ORIENTED_EDGE('',*,*,#16183,.F.);
#22598=ORIENTED_EDGE('',*,*,#16187,.F.);
#22599=ORIENTED_EDGE('',*,*,#16188,.T.);
#22600=ORIENTED_EDGE('',*,*,#16187,.T.);
#22601=ORIENTED_EDGE('',*,*,#16182,.F.);
#22602=ORIENTED_EDGE('',*,*,#16189,.F.);
#22603=ORIENTED_EDGE('',*,*,#16190,.T.);
#22604=ORIENTED_EDGE('',*,*,#16189,.T.);
#22605=ORIENTED_EDGE('',*,*,#16181,.F.);
#22606=ORIENTED_EDGE('',*,*,#16191,.F.);
#22607=ORIENTED_EDGE('',*,*,#16192,.T.);
#22608=ORIENTED_EDGE('',*,*,#16191,.T.);
#22609=ORIENTED_EDGE('',*,*,#16180,.F.);
#22610=ORIENTED_EDGE('',*,*,#16193,.F.);
#22611=ORIENTED_EDGE('',*,*,#16194,.T.);
#22612=ORIENTED_EDGE('',*,*,#16193,.T.);
#22613=ORIENTED_EDGE('',*,*,#16179,.F.);
#22614=ORIENTED_EDGE('',*,*,#16195,.F.);
#22615=ORIENTED_EDGE('',*,*,#16196,.T.);
#22616=ORIENTED_EDGE('',*,*,#16195,.T.);
#22617=ORIENTED_EDGE('',*,*,#16178,.F.);
#22618=ORIENTED_EDGE('',*,*,#16186,.F.);
#22619=ORIENTED_EDGE('',*,*,#16196,.F.);
#22620=ORIENTED_EDGE('',*,*,#16185,.F.);
#22621=ORIENTED_EDGE('',*,*,#16188,.F.);
#22622=ORIENTED_EDGE('',*,*,#16190,.F.);
#22623=ORIENTED_EDGE('',*,*,#16192,.F.);
#22624=ORIENTED_EDGE('',*,*,#16194,.F.);
#22625=ORIENTED_EDGE('',*,*,#16175,.T.);
#22626=ORIENTED_EDGE('',*,*,#16197,.F.);
#22627=ORIENTED_EDGE('',*,*,#16198,.T.);
#22628=ORIENTED_EDGE('',*,*,#16199,.F.);
#22629=ORIENTED_EDGE('',*,*,#16200,.T.);
#22630=ORIENTED_EDGE('',*,*,#16201,.T.);
#22631=ORIENTED_EDGE('',*,*,#16202,.F.);
#22632=ORIENTED_EDGE('',*,*,#16201,.F.);
#22633=ORIENTED_EDGE('',*,*,#16203,.T.);
#22634=ORIENTED_EDGE('',*,*,#16184,.T.);
#22635=ORIENTED_EDGE('',*,*,#16203,.F.);
#22636=ORIENTED_EDGE('',*,*,#16200,.F.);
#22637=ORIENTED_EDGE('',*,*,#16204,.F.);
#22638=ORIENTED_EDGE('',*,*,#16198,.F.);
#22639=ORIENTED_EDGE('',*,*,#16205,.F.);
#22640=ORIENTED_EDGE('',*,*,#16206,.T.);
#22641=ORIENTED_EDGE('',*,*,#16207,.F.);
#22642=ORIENTED_EDGE('',*,*,#16208,.F.);
#22643=ORIENTED_EDGE('',*,*,#16209,.F.);
#22644=ORIENTED_EDGE('',*,*,#16208,.T.);
#22645=ORIENTED_EDGE('',*,*,#16210,.F.);
#22646=ORIENTED_EDGE('',*,*,#16211,.F.);
#22647=ORIENTED_EDGE('',*,*,#16212,.F.);
#22648=ORIENTED_EDGE('',*,*,#16211,.T.);
#22649=ORIENTED_EDGE('',*,*,#16213,.F.);
#22650=ORIENTED_EDGE('',*,*,#16214,.F.);
#22651=ORIENTED_EDGE('',*,*,#16215,.F.);
#22652=ORIENTED_EDGE('',*,*,#16214,.T.);
#22653=ORIENTED_EDGE('',*,*,#16216,.F.);
#22654=ORIENTED_EDGE('',*,*,#16217,.F.);
#22655=ORIENTED_EDGE('',*,*,#16218,.F.);
#22656=ORIENTED_EDGE('',*,*,#16217,.T.);
#22657=ORIENTED_EDGE('',*,*,#16219,.F.);
#22658=ORIENTED_EDGE('',*,*,#16220,.F.);
#22659=ORIENTED_EDGE('',*,*,#16221,.F.);
#22660=ORIENTED_EDGE('',*,*,#16220,.T.);
#22661=ORIENTED_EDGE('',*,*,#16222,.F.);
#22662=ORIENTED_EDGE('',*,*,#16223,.F.);
#22663=ORIENTED_EDGE('',*,*,#16224,.F.);
#22664=ORIENTED_EDGE('',*,*,#16223,.T.);
#22665=ORIENTED_EDGE('',*,*,#16225,.F.);
#22666=ORIENTED_EDGE('',*,*,#16206,.F.);
#22667=ORIENTED_EDGE('',*,*,#16225,.T.);
#22668=ORIENTED_EDGE('',*,*,#16222,.T.);
#22669=ORIENTED_EDGE('',*,*,#16219,.T.);
#22670=ORIENTED_EDGE('',*,*,#16216,.T.);
#22671=ORIENTED_EDGE('',*,*,#16213,.T.);
#22672=ORIENTED_EDGE('',*,*,#16210,.T.);
#22673=ORIENTED_EDGE('',*,*,#16207,.T.);
#22674=ORIENTED_EDGE('',*,*,#16226,.F.);
#22675=ORIENTED_EDGE('',*,*,#16227,.T.);
#22676=ORIENTED_EDGE('',*,*,#16228,.T.);
#22677=ORIENTED_EDGE('',*,*,#16229,.F.);
#22678=ORIENTED_EDGE('',*,*,#16230,.F.);
#22679=ORIENTED_EDGE('',*,*,#16231,.T.);
#22680=ORIENTED_EDGE('',*,*,#16232,.T.);
#22681=ORIENTED_EDGE('',*,*,#16227,.F.);
#22682=ORIENTED_EDGE('',*,*,#16233,.F.);
#22683=ORIENTED_EDGE('',*,*,#16234,.T.);
#22684=ORIENTED_EDGE('',*,*,#16235,.T.);
#22685=ORIENTED_EDGE('',*,*,#16231,.F.);
#22686=ORIENTED_EDGE('',*,*,#16236,.F.);
#22687=ORIENTED_EDGE('',*,*,#16229,.T.);
#22688=ORIENTED_EDGE('',*,*,#16237,.T.);
#22689=ORIENTED_EDGE('',*,*,#16234,.F.);
#22690=ORIENTED_EDGE('',*,*,#16237,.F.);
#22691=ORIENTED_EDGE('',*,*,#16228,.F.);
#22692=ORIENTED_EDGE('',*,*,#16232,.F.);
#22693=ORIENTED_EDGE('',*,*,#16235,.F.);
#22694=ORIENTED_EDGE('',*,*,#16238,.F.);
#22695=ORIENTED_EDGE('',*,*,#16239,.T.);
#22696=ORIENTED_EDGE('',*,*,#16240,.T.);
#22697=ORIENTED_EDGE('',*,*,#16241,.F.);
#22698=ORIENTED_EDGE('',*,*,#16242,.F.);
#22699=ORIENTED_EDGE('',*,*,#16243,.T.);
#22700=ORIENTED_EDGE('',*,*,#16244,.T.);
#22701=ORIENTED_EDGE('',*,*,#16239,.F.);
#22702=ORIENTED_EDGE('',*,*,#16245,.F.);
#22703=ORIENTED_EDGE('',*,*,#16246,.T.);
#22704=ORIENTED_EDGE('',*,*,#16247,.T.);
#22705=ORIENTED_EDGE('',*,*,#16243,.F.);
#22706=ORIENTED_EDGE('',*,*,#16248,.F.);
#22707=ORIENTED_EDGE('',*,*,#16241,.T.);
#22708=ORIENTED_EDGE('',*,*,#16249,.T.);
#22709=ORIENTED_EDGE('',*,*,#16246,.F.);
#22710=ORIENTED_EDGE('',*,*,#16249,.F.);
#22711=ORIENTED_EDGE('',*,*,#16240,.F.);
#22712=ORIENTED_EDGE('',*,*,#16244,.F.);
#22713=ORIENTED_EDGE('',*,*,#16247,.F.);
#22714=ORIENTED_EDGE('',*,*,#16250,.F.);
#22715=ORIENTED_EDGE('',*,*,#16251,.T.);
#22716=ORIENTED_EDGE('',*,*,#16252,.T.);
#22717=ORIENTED_EDGE('',*,*,#16253,.F.);
#22718=ORIENTED_EDGE('',*,*,#16254,.F.);
#22719=ORIENTED_EDGE('',*,*,#16255,.T.);
#22720=ORIENTED_EDGE('',*,*,#16256,.T.);
#22721=ORIENTED_EDGE('',*,*,#16251,.F.);
#22722=ORIENTED_EDGE('',*,*,#16257,.F.);
#22723=ORIENTED_EDGE('',*,*,#16258,.T.);
#22724=ORIENTED_EDGE('',*,*,#16259,.T.);
#22725=ORIENTED_EDGE('',*,*,#16255,.F.);
#22726=ORIENTED_EDGE('',*,*,#16260,.F.);
#22727=ORIENTED_EDGE('',*,*,#16253,.T.);
#22728=ORIENTED_EDGE('',*,*,#16261,.T.);
#22729=ORIENTED_EDGE('',*,*,#16258,.F.);
#22730=ORIENTED_EDGE('',*,*,#16261,.F.);
#22731=ORIENTED_EDGE('',*,*,#16252,.F.);
#22732=ORIENTED_EDGE('',*,*,#16256,.F.);
#22733=ORIENTED_EDGE('',*,*,#16259,.F.);
#22734=ORIENTED_EDGE('',*,*,#16262,.F.);
#22735=ORIENTED_EDGE('',*,*,#16263,.T.);
#22736=ORIENTED_EDGE('',*,*,#16264,.T.);
#22737=ORIENTED_EDGE('',*,*,#16265,.F.);
#22738=ORIENTED_EDGE('',*,*,#16266,.F.);
#22739=ORIENTED_EDGE('',*,*,#16267,.T.);
#22740=ORIENTED_EDGE('',*,*,#16268,.T.);
#22741=ORIENTED_EDGE('',*,*,#16263,.F.);
#22742=ORIENTED_EDGE('',*,*,#16269,.F.);
#22743=ORIENTED_EDGE('',*,*,#16270,.T.);
#22744=ORIENTED_EDGE('',*,*,#16271,.T.);
#22745=ORIENTED_EDGE('',*,*,#16267,.F.);
#22746=ORIENTED_EDGE('',*,*,#16272,.F.);
#22747=ORIENTED_EDGE('',*,*,#16265,.T.);
#22748=ORIENTED_EDGE('',*,*,#16273,.T.);
#22749=ORIENTED_EDGE('',*,*,#16270,.F.);
#22750=ORIENTED_EDGE('',*,*,#16273,.F.);
#22751=ORIENTED_EDGE('',*,*,#16264,.F.);
#22752=ORIENTED_EDGE('',*,*,#16268,.F.);
#22753=ORIENTED_EDGE('',*,*,#16271,.F.);
#22754=ORIENTED_EDGE('',*,*,#16274,.F.);
#22755=ORIENTED_EDGE('',*,*,#16275,.T.);
#22756=ORIENTED_EDGE('',*,*,#16276,.T.);
#22757=ORIENTED_EDGE('',*,*,#16277,.F.);
#22758=ORIENTED_EDGE('',*,*,#16278,.F.);
#22759=ORIENTED_EDGE('',*,*,#16279,.T.);
#22760=ORIENTED_EDGE('',*,*,#16280,.T.);
#22761=ORIENTED_EDGE('',*,*,#16275,.F.);
#22762=ORIENTED_EDGE('',*,*,#16281,.F.);
#22763=ORIENTED_EDGE('',*,*,#16282,.T.);
#22764=ORIENTED_EDGE('',*,*,#16283,.T.);
#22765=ORIENTED_EDGE('',*,*,#16279,.F.);
#22766=ORIENTED_EDGE('',*,*,#16284,.F.);
#22767=ORIENTED_EDGE('',*,*,#16277,.T.);
#22768=ORIENTED_EDGE('',*,*,#16285,.T.);
#22769=ORIENTED_EDGE('',*,*,#16282,.F.);
#22770=ORIENTED_EDGE('',*,*,#16285,.F.);
#22771=ORIENTED_EDGE('',*,*,#16276,.F.);
#22772=ORIENTED_EDGE('',*,*,#16280,.F.);
#22773=ORIENTED_EDGE('',*,*,#16283,.F.);
#22774=ORIENTED_EDGE('',*,*,#16286,.F.);
#22775=ORIENTED_EDGE('',*,*,#16287,.T.);
#22776=ORIENTED_EDGE('',*,*,#16288,.T.);
#22777=ORIENTED_EDGE('',*,*,#16289,.F.);
#22778=ORIENTED_EDGE('',*,*,#16290,.F.);
#22779=ORIENTED_EDGE('',*,*,#16291,.T.);
#22780=ORIENTED_EDGE('',*,*,#16292,.T.);
#22781=ORIENTED_EDGE('',*,*,#16287,.F.);
#22782=ORIENTED_EDGE('',*,*,#16293,.F.);
#22783=ORIENTED_EDGE('',*,*,#16294,.T.);
#22784=ORIENTED_EDGE('',*,*,#16295,.T.);
#22785=ORIENTED_EDGE('',*,*,#16291,.F.);
#22786=ORIENTED_EDGE('',*,*,#16296,.F.);
#22787=ORIENTED_EDGE('',*,*,#16289,.T.);
#22788=ORIENTED_EDGE('',*,*,#16297,.T.);
#22789=ORIENTED_EDGE('',*,*,#16294,.F.);
#22790=ORIENTED_EDGE('',*,*,#16297,.F.);
#22791=ORIENTED_EDGE('',*,*,#16288,.F.);
#22792=ORIENTED_EDGE('',*,*,#16292,.F.);
#22793=ORIENTED_EDGE('',*,*,#16295,.F.);
#22794=ORIENTED_EDGE('',*,*,#16298,.F.);
#22795=ORIENTED_EDGE('',*,*,#16299,.T.);
#22796=ORIENTED_EDGE('',*,*,#16300,.T.);
#22797=ORIENTED_EDGE('',*,*,#16301,.F.);
#22798=ORIENTED_EDGE('',*,*,#16302,.F.);
#22799=ORIENTED_EDGE('',*,*,#16303,.T.);
#22800=ORIENTED_EDGE('',*,*,#16304,.T.);
#22801=ORIENTED_EDGE('',*,*,#16299,.F.);
#22802=ORIENTED_EDGE('',*,*,#16305,.F.);
#22803=ORIENTED_EDGE('',*,*,#16306,.T.);
#22804=ORIENTED_EDGE('',*,*,#16307,.T.);
#22805=ORIENTED_EDGE('',*,*,#16303,.F.);
#22806=ORIENTED_EDGE('',*,*,#16308,.F.);
#22807=ORIENTED_EDGE('',*,*,#16301,.T.);
#22808=ORIENTED_EDGE('',*,*,#16309,.T.);
#22809=ORIENTED_EDGE('',*,*,#16306,.F.);
#22810=ORIENTED_EDGE('',*,*,#16309,.F.);
#22811=ORIENTED_EDGE('',*,*,#16300,.F.);
#22812=ORIENTED_EDGE('',*,*,#16304,.F.);
#22813=ORIENTED_EDGE('',*,*,#16307,.F.);
#22814=ORIENTED_EDGE('',*,*,#16310,.F.);
#22815=ORIENTED_EDGE('',*,*,#16311,.T.);
#22816=ORIENTED_EDGE('',*,*,#16312,.T.);
#22817=ORIENTED_EDGE('',*,*,#16313,.F.);
#22818=ORIENTED_EDGE('',*,*,#16314,.F.);
#22819=ORIENTED_EDGE('',*,*,#16315,.T.);
#22820=ORIENTED_EDGE('',*,*,#16316,.T.);
#22821=ORIENTED_EDGE('',*,*,#16311,.F.);
#22822=ORIENTED_EDGE('',*,*,#16317,.F.);
#22823=ORIENTED_EDGE('',*,*,#16318,.T.);
#22824=ORIENTED_EDGE('',*,*,#16319,.T.);
#22825=ORIENTED_EDGE('',*,*,#16315,.F.);
#22826=ORIENTED_EDGE('',*,*,#16320,.F.);
#22827=ORIENTED_EDGE('',*,*,#16313,.T.);
#22828=ORIENTED_EDGE('',*,*,#16321,.T.);
#22829=ORIENTED_EDGE('',*,*,#16318,.F.);
#22830=ORIENTED_EDGE('',*,*,#16321,.F.);
#22831=ORIENTED_EDGE('',*,*,#16312,.F.);
#22832=ORIENTED_EDGE('',*,*,#16316,.F.);
#22833=ORIENTED_EDGE('',*,*,#16319,.F.);
#22834=ORIENTED_EDGE('',*,*,#16322,.F.);
#22835=ORIENTED_EDGE('',*,*,#16323,.T.);
#22836=ORIENTED_EDGE('',*,*,#16324,.T.);
#22837=ORIENTED_EDGE('',*,*,#16325,.F.);
#22838=ORIENTED_EDGE('',*,*,#16326,.F.);
#22839=ORIENTED_EDGE('',*,*,#16327,.T.);
#22840=ORIENTED_EDGE('',*,*,#16328,.T.);
#22841=ORIENTED_EDGE('',*,*,#16323,.F.);
#22842=ORIENTED_EDGE('',*,*,#16329,.F.);
#22843=ORIENTED_EDGE('',*,*,#16330,.T.);
#22844=ORIENTED_EDGE('',*,*,#16331,.T.);
#22845=ORIENTED_EDGE('',*,*,#16327,.F.);
#22846=ORIENTED_EDGE('',*,*,#16332,.F.);
#22847=ORIENTED_EDGE('',*,*,#16325,.T.);
#22848=ORIENTED_EDGE('',*,*,#16333,.T.);
#22849=ORIENTED_EDGE('',*,*,#16330,.F.);
#22850=ORIENTED_EDGE('',*,*,#16333,.F.);
#22851=ORIENTED_EDGE('',*,*,#16324,.F.);
#22852=ORIENTED_EDGE('',*,*,#16328,.F.);
#22853=ORIENTED_EDGE('',*,*,#16331,.F.);
#22854=ORIENTED_EDGE('',*,*,#16334,.F.);
#22855=ORIENTED_EDGE('',*,*,#16335,.T.);
#22856=ORIENTED_EDGE('',*,*,#16336,.T.);
#22857=ORIENTED_EDGE('',*,*,#16337,.F.);
#22858=ORIENTED_EDGE('',*,*,#16338,.F.);
#22859=ORIENTED_EDGE('',*,*,#16339,.T.);
#22860=ORIENTED_EDGE('',*,*,#16340,.T.);
#22861=ORIENTED_EDGE('',*,*,#16335,.F.);
#22862=ORIENTED_EDGE('',*,*,#16341,.F.);
#22863=ORIENTED_EDGE('',*,*,#16342,.T.);
#22864=ORIENTED_EDGE('',*,*,#16343,.T.);
#22865=ORIENTED_EDGE('',*,*,#16339,.F.);
#22866=ORIENTED_EDGE('',*,*,#16344,.F.);
#22867=ORIENTED_EDGE('',*,*,#16337,.T.);
#22868=ORIENTED_EDGE('',*,*,#16345,.T.);
#22869=ORIENTED_EDGE('',*,*,#16342,.F.);
#22870=ORIENTED_EDGE('',*,*,#16345,.F.);
#22871=ORIENTED_EDGE('',*,*,#16336,.F.);
#22872=ORIENTED_EDGE('',*,*,#16340,.F.);
#22873=ORIENTED_EDGE('',*,*,#16343,.F.);
#22874=ORIENTED_EDGE('',*,*,#16346,.F.);
#22875=ORIENTED_EDGE('',*,*,#16347,.T.);
#22876=ORIENTED_EDGE('',*,*,#16348,.T.);
#22877=ORIENTED_EDGE('',*,*,#16349,.F.);
#22878=ORIENTED_EDGE('',*,*,#16350,.F.);
#22879=ORIENTED_EDGE('',*,*,#16351,.T.);
#22880=ORIENTED_EDGE('',*,*,#16352,.T.);
#22881=ORIENTED_EDGE('',*,*,#16347,.F.);
#22882=ORIENTED_EDGE('',*,*,#16353,.F.);
#22883=ORIENTED_EDGE('',*,*,#16354,.T.);
#22884=ORIENTED_EDGE('',*,*,#16355,.T.);
#22885=ORIENTED_EDGE('',*,*,#16351,.F.);
#22886=ORIENTED_EDGE('',*,*,#16356,.F.);
#22887=ORIENTED_EDGE('',*,*,#16349,.T.);
#22888=ORIENTED_EDGE('',*,*,#16357,.T.);
#22889=ORIENTED_EDGE('',*,*,#16354,.F.);
#22890=ORIENTED_EDGE('',*,*,#16357,.F.);
#22891=ORIENTED_EDGE('',*,*,#16348,.F.);
#22892=ORIENTED_EDGE('',*,*,#16352,.F.);
#22893=ORIENTED_EDGE('',*,*,#16355,.F.);
#22894=ORIENTED_EDGE('',*,*,#16358,.T.);
#22895=ORIENTED_EDGE('',*,*,#16226,.T.);
#22896=ORIENTED_EDGE('',*,*,#16236,.T.);
#22897=ORIENTED_EDGE('',*,*,#16233,.T.);
#22898=ORIENTED_EDGE('',*,*,#16230,.T.);
#22899=ORIENTED_EDGE('',*,*,#16238,.T.);
#22900=ORIENTED_EDGE('',*,*,#16248,.T.);
#22901=ORIENTED_EDGE('',*,*,#16245,.T.);
#22902=ORIENTED_EDGE('',*,*,#16242,.T.);
#22903=ORIENTED_EDGE('',*,*,#16250,.T.);
#22904=ORIENTED_EDGE('',*,*,#16260,.T.);
#22905=ORIENTED_EDGE('',*,*,#16257,.T.);
#22906=ORIENTED_EDGE('',*,*,#16254,.T.);
#22907=ORIENTED_EDGE('',*,*,#16262,.T.);
#22908=ORIENTED_EDGE('',*,*,#16272,.T.);
#22909=ORIENTED_EDGE('',*,*,#16269,.T.);
#22910=ORIENTED_EDGE('',*,*,#16266,.T.);
#22911=ORIENTED_EDGE('',*,*,#16274,.T.);
#22912=ORIENTED_EDGE('',*,*,#16284,.T.);
#22913=ORIENTED_EDGE('',*,*,#16281,.T.);
#22914=ORIENTED_EDGE('',*,*,#16278,.T.);
#22915=ORIENTED_EDGE('',*,*,#16286,.T.);
#22916=ORIENTED_EDGE('',*,*,#16296,.T.);
#22917=ORIENTED_EDGE('',*,*,#16293,.T.);
#22918=ORIENTED_EDGE('',*,*,#16290,.T.);
#22919=ORIENTED_EDGE('',*,*,#16298,.T.);
#22920=ORIENTED_EDGE('',*,*,#16308,.T.);
#22921=ORIENTED_EDGE('',*,*,#16305,.T.);
#22922=ORIENTED_EDGE('',*,*,#16302,.T.);
#22923=ORIENTED_EDGE('',*,*,#16310,.T.);
#22924=ORIENTED_EDGE('',*,*,#16320,.T.);
#22925=ORIENTED_EDGE('',*,*,#16317,.T.);
#22926=ORIENTED_EDGE('',*,*,#16314,.T.);
#22927=ORIENTED_EDGE('',*,*,#16322,.T.);
#22928=ORIENTED_EDGE('',*,*,#16332,.T.);
#22929=ORIENTED_EDGE('',*,*,#16329,.T.);
#22930=ORIENTED_EDGE('',*,*,#16326,.T.);
#22931=ORIENTED_EDGE('',*,*,#16334,.T.);
#22932=ORIENTED_EDGE('',*,*,#16344,.T.);
#22933=ORIENTED_EDGE('',*,*,#16341,.T.);
#22934=ORIENTED_EDGE('',*,*,#16338,.T.);
#22935=ORIENTED_EDGE('',*,*,#16346,.T.);
#22936=ORIENTED_EDGE('',*,*,#16356,.T.);
#22937=ORIENTED_EDGE('',*,*,#16353,.T.);
#22938=ORIENTED_EDGE('',*,*,#16350,.T.);
#22939=ORIENTED_EDGE('',*,*,#16205,.T.);
#22940=ORIENTED_EDGE('',*,*,#16209,.T.);
#22941=ORIENTED_EDGE('',*,*,#16212,.T.);
#22942=ORIENTED_EDGE('',*,*,#16215,.T.);
#22943=ORIENTED_EDGE('',*,*,#16218,.T.);
#22944=ORIENTED_EDGE('',*,*,#16221,.T.);
#22945=ORIENTED_EDGE('',*,*,#16224,.T.);
#22946=ORIENTED_EDGE('',*,*,#16358,.F.);
#22947=ORIENTED_EDGE('',*,*,#16359,.T.);
#22948=ORIENTED_EDGE('',*,*,#16360,.F.);
#22949=ORIENTED_EDGE('',*,*,#16359,.F.);
#22950=ORIENTED_EDGE('',*,*,#16361,.F.);
#22951=ORIENTED_EDGE('',*,*,#16362,.F.);
#22952=ORIENTED_EDGE('',*,*,#16363,.T.);
#22953=ORIENTED_EDGE('',*,*,#16361,.T.);
#22954=ORIENTED_EDGE('',*,*,#16363,.F.);
#22955=ORIENTED_EDGE('',*,*,#16364,.F.);
#22956=ORIENTED_EDGE('',*,*,#16365,.T.);
#22957=ORIENTED_EDGE('',*,*,#16362,.T.);
#22958=ORIENTED_EDGE('',*,*,#16365,.F.);
#22959=ORIENTED_EDGE('',*,*,#16204,.T.);
#22960=ORIENTED_EDGE('',*,*,#16199,.T.);
#22961=ORIENTED_EDGE('',*,*,#16202,.T.);
#22962=ORIENTED_EDGE('',*,*,#16197,.T.);
#22963=ORIENTED_EDGE('',*,*,#16366,.F.);
#22964=ORIENTED_EDGE('',*,*,#16364,.T.);
#22965=ORIENTED_EDGE('',*,*,#16367,.F.);
#22966=ORIENTED_EDGE('',*,*,#16368,.T.);
#22967=ORIENTED_EDGE('',*,*,#16366,.T.);
#22968=ORIENTED_EDGE('',*,*,#16368,.F.);
#22969=ORIENTED_EDGE('',*,*,#16369,.F.);
#22970=ORIENTED_EDGE('',*,*,#16370,.T.);
#22971=ORIENTED_EDGE('',*,*,#16367,.T.);
#22972=ORIENTED_EDGE('',*,*,#16370,.F.);
#22973=ORIENTED_EDGE('',*,*,#16369,.T.);
#22974=ORIENTED_EDGE('',*,*,#16360,.T.);
#22975=ORIENTED_EDGE('',*,*,#16371,.T.);
#22976=ORIENTED_EDGE('',*,*,#16372,.T.);
#22977=ORIENTED_EDGE('',*,*,#16373,.T.);
#22978=ORIENTED_EDGE('',*,*,#16371,.F.);
#22979=ORIENTED_EDGE('',*,*,#16374,.T.);
#22980=ORIENTED_EDGE('',*,*,#16372,.F.);
#22981=ORIENTED_EDGE('',*,*,#16373,.F.);
#22982=ORIENTED_EDGE('',*,*,#16375,.T.);
#22983=ORIENTED_EDGE('',*,*,#16376,.F.);
#22984=ORIENTED_EDGE('',*,*,#16377,.F.);
#22985=ORIENTED_EDGE('',*,*,#16375,.F.);
#22986=ORIENTED_EDGE('',*,*,#16378,.F.);
#22987=ORIENTED_EDGE('',*,*,#16379,.T.);
#22988=ORIENTED_EDGE('',*,*,#16380,.T.);
#22989=ORIENTED_EDGE('',*,*,#16379,.F.);
#22990=ORIENTED_EDGE('',*,*,#16381,.F.);
#22991=ORIENTED_EDGE('',*,*,#16374,.F.);
#22992=ORIENTED_EDGE('',*,*,#16382,.T.);
#22993=ORIENTED_EDGE('',*,*,#16376,.T.);
#22994=ORIENTED_EDGE('',*,*,#16377,.T.);
#22995=ORIENTED_EDGE('',*,*,#16382,.F.);
#22996=ORIENTED_EDGE('',*,*,#16381,.T.);
#22997=ORIENTED_EDGE('',*,*,#16383,.F.);
#22998=ORIENTED_EDGE('',*,*,#16384,.T.);
#22999=ORIENTED_EDGE('',*,*,#16383,.T.);
#23000=ORIENTED_EDGE('',*,*,#16384,.F.);
#23001=ORIENTED_EDGE('',*,*,#16385,.F.);
#23002=ORIENTED_EDGE('',*,*,#16386,.F.);
#23003=ORIENTED_EDGE('',*,*,#16387,.F.);
#23004=ORIENTED_EDGE('',*,*,#16388,.F.);
#23005=ORIENTED_EDGE('',*,*,#16389,.T.);
#23006=ORIENTED_EDGE('',*,*,#16386,.T.);
#23007=ORIENTED_EDGE('',*,*,#16385,.T.);
#23008=ORIENTED_EDGE('',*,*,#16390,.T.);
#23009=ORIENTED_EDGE('',*,*,#16391,.T.);
#23010=ORIENTED_EDGE('',*,*,#16390,.F.);
#23011=ORIENTED_EDGE('',*,*,#16387,.T.);
#23012=ORIENTED_EDGE('',*,*,#16389,.F.);
#23013=ORIENTED_EDGE('',*,*,#16392,.F.);
#23014=ORIENTED_EDGE('',*,*,#16391,.F.);
#23015=ORIENTED_EDGE('',*,*,#16393,.T.);
#23016=ORIENTED_EDGE('',*,*,#16392,.T.);
#23017=ORIENTED_EDGE('',*,*,#16393,.F.);
#23018=ORIENTED_EDGE('',*,*,#16394,.F.);
#23019=ORIENTED_EDGE('',*,*,#16388,.T.);
#23020=ORIENTED_EDGE('',*,*,#16395,.F.);
#23021=ORIENTED_EDGE('',*,*,#16396,.T.);
#23022=ORIENTED_EDGE('',*,*,#16394,.T.);
#23023=ORIENTED_EDGE('',*,*,#16396,.F.);
#23024=ORIENTED_EDGE('',*,*,#16397,.F.);
#23025=ORIENTED_EDGE('',*,*,#16398,.T.);
#23026=ORIENTED_EDGE('',*,*,#16395,.T.);
#23027=ORIENTED_EDGE('',*,*,#16398,.F.);
#23028=ORIENTED_EDGE('',*,*,#16399,.F.);
#23029=ORIENTED_EDGE('',*,*,#16400,.T.);
#23030=ORIENTED_EDGE('',*,*,#16397,.T.);
#23031=ORIENTED_EDGE('',*,*,#16400,.F.);
#23032=ORIENTED_EDGE('',*,*,#16399,.T.);
#23033=ORIENTED_EDGE('',*,*,#16380,.F.);
#23034=ORIENTED_EDGE('',*,*,#16401,.F.);
#23035=ORIENTED_EDGE('',*,*,#16402,.T.);
#23036=ORIENTED_EDGE('',*,*,#16378,.T.);
#23037=ORIENTED_EDGE('',*,*,#16402,.F.);
#23038=ORIENTED_EDGE('',*,*,#16401,.T.);
#23039=ORIENTED_EDGE('',*,*,#16403,.T.);
#23040=ORIENTED_EDGE('',*,*,#16404,.T.);
#23041=ORIENTED_EDGE('',*,*,#16405,.F.);
#23042=ORIENTED_EDGE('',*,*,#16404,.F.);
#23043=ORIENTED_EDGE('',*,*,#16405,.T.);
#23044=ORIENTED_EDGE('',*,*,#16403,.F.);
#23045=ORIENTED_EDGE('',*,*,#16406,.T.);
#23046=ORIENTED_EDGE('',*,*,#16407,.T.);
#23047=ORIENTED_EDGE('',*,*,#16408,.T.);
#23048=ORIENTED_EDGE('',*,*,#16409,.T.);
#23049=ORIENTED_EDGE('',*,*,#16407,.F.);
#23050=ORIENTED_EDGE('',*,*,#16410,.F.);
#23051=ORIENTED_EDGE('',*,*,#16411,.F.);
#23052=ORIENTED_EDGE('',*,*,#16412,.F.);
#23053=ORIENTED_EDGE('',*,*,#16413,.T.);
#23054=ORIENTED_EDGE('',*,*,#16411,.T.);
#23055=ORIENTED_EDGE('',*,*,#16414,.T.);
#23056=ORIENTED_EDGE('',*,*,#16415,.T.);
#23057=ORIENTED_EDGE('',*,*,#16416,.T.);
#23058=ORIENTED_EDGE('',*,*,#16417,.T.);
#23059=ORIENTED_EDGE('',*,*,#16418,.T.);
#23060=ORIENTED_EDGE('',*,*,#16419,.T.);
#23061=ORIENTED_EDGE('',*,*,#16417,.F.);
#23062=ORIENTED_EDGE('',*,*,#16420,.F.);
#23063=ORIENTED_EDGE('',*,*,#16421,.F.);
#23064=ORIENTED_EDGE('',*,*,#16422,.F.);
#23065=ORIENTED_EDGE('',*,*,#16423,.T.);
#23066=ORIENTED_EDGE('',*,*,#16421,.T.);
#23067=ORIENTED_EDGE('',*,*,#16424,.T.);
#23068=ORIENTED_EDGE('',*,*,#16425,.T.);
#23069=ORIENTED_EDGE('',*,*,#16426,.T.);
#23070=ORIENTED_EDGE('',*,*,#16427,.T.);
#23071=ORIENTED_EDGE('',*,*,#16428,.T.);
#23072=ORIENTED_EDGE('',*,*,#16429,.T.);
#23073=ORIENTED_EDGE('',*,*,#16430,.T.);
#23074=ORIENTED_EDGE('',*,*,#16429,.F.);
#23075=ORIENTED_EDGE('',*,*,#16431,.F.);
#23076=ORIENTED_EDGE('',*,*,#16432,.T.);
#23077=ORIENTED_EDGE('',*,*,#16433,.T.);
#23078=ORIENTED_EDGE('',*,*,#16434,.T.);
#23079=ORIENTED_EDGE('',*,*,#16435,.F.);
#23080=ORIENTED_EDGE('',*,*,#16436,.F.);
#23081=ORIENTED_EDGE('',*,*,#16437,.T.);
#23082=ORIENTED_EDGE('',*,*,#16438,.F.);
#23083=ORIENTED_EDGE('',*,*,#16439,.F.);
#23084=ORIENTED_EDGE('',*,*,#16432,.F.);
#23085=ORIENTED_EDGE('',*,*,#16436,.T.);
#23086=ORIENTED_EDGE('',*,*,#16440,.F.);
#23087=ORIENTED_EDGE('',*,*,#16441,.T.);
#23088=ORIENTED_EDGE('',*,*,#16442,.T.);
#23089=ORIENTED_EDGE('',*,*,#16443,.T.);
#23090=ORIENTED_EDGE('',*,*,#16444,.F.);
#23091=ORIENTED_EDGE('',*,*,#16434,.F.);
#23092=ORIENTED_EDGE('',*,*,#16445,.T.);
#23093=ORIENTED_EDGE('',*,*,#16425,.F.);
#23094=ORIENTED_EDGE('',*,*,#16446,.F.);
#23095=ORIENTED_EDGE('',*,*,#16447,.F.);
#23096=ORIENTED_EDGE('',*,*,#16448,.T.);
#23097=ORIENTED_EDGE('',*,*,#16449,.T.);
#23098=ORIENTED_EDGE('',*,*,#16441,.F.);
#23099=ORIENTED_EDGE('',*,*,#16450,.F.);
#23100=ORIENTED_EDGE('',*,*,#16433,.F.);
#23101=ORIENTED_EDGE('',*,*,#16451,.F.);
#23102=ORIENTED_EDGE('',*,*,#16452,.F.);
#23103=ORIENTED_EDGE('',*,*,#16453,.F.);
#23104=ORIENTED_EDGE('',*,*,#16454,.F.);
#23105=ORIENTED_EDGE('',*,*,#16455,.F.);
#23106=ORIENTED_EDGE('',*,*,#16456,.T.);
#23107=ORIENTED_EDGE('',*,*,#16452,.T.);
#23108=ORIENTED_EDGE('',*,*,#16457,.T.);
#23109=ORIENTED_EDGE('',*,*,#16458,.T.);
#23110=ORIENTED_EDGE('',*,*,#16459,.T.);
#23111=ORIENTED_EDGE('',*,*,#16460,.T.);
#23112=ORIENTED_EDGE('',*,*,#16456,.F.);
#23113=ORIENTED_EDGE('',*,*,#16461,.F.);
#23114=ORIENTED_EDGE('',*,*,#16462,.T.);
#23115=ORIENTED_EDGE('',*,*,#16463,.F.);
#23116=ORIENTED_EDGE('',*,*,#16464,.F.);
#23117=ORIENTED_EDGE('',*,*,#16453,.T.);
#23118=ORIENTED_EDGE('',*,*,#16460,.F.);
#23119=ORIENTED_EDGE('',*,*,#16465,.T.);
#23120=ORIENTED_EDGE('',*,*,#16466,.T.);
#23121=ORIENTED_EDGE('',*,*,#16467,.T.);
#23122=ORIENTED_EDGE('',*,*,#16461,.T.);
#23123=ORIENTED_EDGE('',*,*,#16468,.T.);
#23124=ORIENTED_EDGE('',*,*,#16454,.T.);
#23125=ORIENTED_EDGE('',*,*,#16464,.T.);
#23126=ORIENTED_EDGE('',*,*,#16469,.T.);
#23127=ORIENTED_EDGE('',*,*,#16470,.T.);
#23128=ORIENTED_EDGE('',*,*,#16471,.T.);
#23129=ORIENTED_EDGE('',*,*,#16468,.F.);
#23130=ORIENTED_EDGE('',*,*,#16472,.F.);
#23131=ORIENTED_EDGE('',*,*,#16473,.T.);
#23132=ORIENTED_EDGE('',*,*,#16445,.F.);
#23133=ORIENTED_EDGE('',*,*,#16455,.T.);
#23134=ORIENTED_EDGE('',*,*,#16471,.F.);
#23135=ORIENTED_EDGE('',*,*,#16474,.T.);
#23136=ORIENTED_EDGE('',*,*,#16475,.T.);
#23137=ORIENTED_EDGE('',*,*,#16476,.T.);
#23138=ORIENTED_EDGE('',*,*,#16472,.T.);
#23139=ORIENTED_EDGE('',*,*,#16477,.T.);
#23140=ORIENTED_EDGE('',*,*,#16478,.F.);
#23141=ORIENTED_EDGE('',*,*,#16479,.T.);
#23142=ORIENTED_EDGE('',*,*,#16480,.T.);
#23143=ORIENTED_EDGE('',*,*,#16481,.T.);
#23144=ORIENTED_EDGE('',*,*,#16482,.F.);
#23145=ORIENTED_EDGE('',*,*,#16477,.F.);
#23146=ORIENTED_EDGE('',*,*,#16483,.T.);
#23147=ORIENTED_EDGE('',*,*,#16484,.F.);
#23148=ORIENTED_EDGE('',*,*,#16485,.F.);
#23149=ORIENTED_EDGE('',*,*,#16486,.T.);
#23150=ORIENTED_EDGE('',*,*,#16487,.T.);
#23151=ORIENTED_EDGE('',*,*,#16488,.T.);
#23152=ORIENTED_EDGE('',*,*,#16481,.F.);
#23153=ORIENTED_EDGE('',*,*,#16489,.T.);
#23154=ORIENTED_EDGE('',*,*,#16490,.F.);
#23155=ORIENTED_EDGE('',*,*,#16483,.F.);
#23156=ORIENTED_EDGE('',*,*,#16409,.F.);
#23157=ORIENTED_EDGE('',*,*,#16491,.F.);
#23158=ORIENTED_EDGE('',*,*,#16492,.F.);
#23159=ORIENTED_EDGE('',*,*,#16493,.T.);
#23160=ORIENTED_EDGE('',*,*,#16494,.T.);
#23161=ORIENTED_EDGE('',*,*,#16479,.F.);
#23162=ORIENTED_EDGE('',*,*,#16495,.F.);
#23163=ORIENTED_EDGE('',*,*,#16480,.F.);
#23164=ORIENTED_EDGE('',*,*,#16494,.F.);
#23165=ORIENTED_EDGE('',*,*,#16496,.F.);
#23166=ORIENTED_EDGE('',*,*,#16497,.F.);
#23167=ORIENTED_EDGE('',*,*,#16498,.F.);
#23168=ORIENTED_EDGE('',*,*,#16489,.F.);
#23169=ORIENTED_EDGE('',*,*,#16498,.T.);
#23170=ORIENTED_EDGE('',*,*,#16499,.T.);
#23171=ORIENTED_EDGE('',*,*,#16500,.T.);
#23172=ORIENTED_EDGE('',*,*,#16484,.T.);
#23173=ORIENTED_EDGE('',*,*,#16490,.T.);
#23174=ORIENTED_EDGE('',*,*,#16415,.F.);
#23175=ORIENTED_EDGE('',*,*,#16501,.F.);
#23176=ORIENTED_EDGE('',*,*,#16499,.F.);
#23177=ORIENTED_EDGE('',*,*,#16497,.T.);
#23178=ORIENTED_EDGE('',*,*,#16502,.T.);
#23179=ORIENTED_EDGE('',*,*,#16503,.T.);
#23180=ORIENTED_EDGE('',*,*,#16504,.F.);
#23181=ORIENTED_EDGE('',*,*,#16505,.F.);
#23182=ORIENTED_EDGE('',*,*,#16506,.F.);
#23183=ORIENTED_EDGE('',*,*,#16486,.F.);
#23184=ORIENTED_EDGE('',*,*,#16507,.F.);
#23185=ORIENTED_EDGE('',*,*,#16488,.F.);
#23186=ORIENTED_EDGE('',*,*,#16508,.T.);
#23187=ORIENTED_EDGE('',*,*,#16487,.F.);
#23188=ORIENTED_EDGE('',*,*,#16509,.F.);
#23189=ORIENTED_EDGE('',*,*,#16510,.F.);
#23190=ORIENTED_EDGE('',*,*,#16511,.F.);
#23191=ORIENTED_EDGE('',*,*,#16512,.F.);
#23192=ORIENTED_EDGE('',*,*,#16513,.F.);
#23193=ORIENTED_EDGE('',*,*,#16514,.T.);
#23194=ORIENTED_EDGE('',*,*,#16512,.T.);
#23195=ORIENTED_EDGE('',*,*,#16515,.T.);
#23196=ORIENTED_EDGE('',*,*,#16516,.T.);
#23197=ORIENTED_EDGE('',*,*,#16517,.T.);
#23198=ORIENTED_EDGE('',*,*,#16518,.T.);
#23199=ORIENTED_EDGE('',*,*,#16516,.F.);
#23200=ORIENTED_EDGE('',*,*,#16519,.T.);
#23201=ORIENTED_EDGE('',*,*,#16520,.T.);
#23202=ORIENTED_EDGE('',*,*,#16521,.T.);
#23203=ORIENTED_EDGE('',*,*,#16522,.T.);
#23204=ORIENTED_EDGE('',*,*,#16515,.F.);
#23205=ORIENTED_EDGE('',*,*,#16511,.T.);
#23206=ORIENTED_EDGE('',*,*,#16523,.F.);
#23207=ORIENTED_EDGE('',*,*,#16524,.F.);
#23208=ORIENTED_EDGE('',*,*,#16525,.T.);
#23209=ORIENTED_EDGE('',*,*,#16519,.F.);
#23210=ORIENTED_EDGE('',*,*,#16523,.T.);
#23211=ORIENTED_EDGE('',*,*,#16510,.T.);
#23212=ORIENTED_EDGE('',*,*,#16526,.T.);
#23213=ORIENTED_EDGE('',*,*,#16527,.T.);
#23214=ORIENTED_EDGE('',*,*,#16528,.T.);
#23215=ORIENTED_EDGE('',*,*,#16529,.T.);
#23216=ORIENTED_EDGE('',*,*,#16529,.F.);
#23217=ORIENTED_EDGE('',*,*,#16530,.T.);
#23218=ORIENTED_EDGE('',*,*,#16531,.T.);
#23219=ORIENTED_EDGE('',*,*,#16532,.T.);
#23220=ORIENTED_EDGE('',*,*,#16524,.T.);
#23221=ORIENTED_EDGE('',*,*,#16533,.T.);
#23222=ORIENTED_EDGE('',*,*,#16534,.T.);
#23223=ORIENTED_EDGE('',*,*,#16535,.T.);
#23224=ORIENTED_EDGE('',*,*,#16536,.T.);
#23225=ORIENTED_EDGE('',*,*,#16537,.T.);
#23226=ORIENTED_EDGE('',*,*,#16538,.T.);
#23227=ORIENTED_EDGE('',*,*,#16533,.F.);
#23228=ORIENTED_EDGE('',*,*,#16539,.T.);
#23229=ORIENTED_EDGE('',*,*,#16540,.T.);
#23230=ORIENTED_EDGE('',*,*,#16541,.T.);
#23231=ORIENTED_EDGE('',*,*,#16537,.F.);
#23232=ORIENTED_EDGE('',*,*,#16542,.T.);
#23233=ORIENTED_EDGE('',*,*,#16543,.T.);
#23234=ORIENTED_EDGE('',*,*,#16544,.T.);
#23235=ORIENTED_EDGE('',*,*,#16540,.F.);
#23236=ORIENTED_EDGE('',*,*,#16545,.T.);
#23237=ORIENTED_EDGE('',*,*,#16546,.T.);
#23238=ORIENTED_EDGE('',*,*,#16547,.T.);
#23239=ORIENTED_EDGE('',*,*,#16543,.F.);
#23240=ORIENTED_EDGE('',*,*,#16548,.T.);
#23241=ORIENTED_EDGE('',*,*,#16549,.T.);
#23242=ORIENTED_EDGE('',*,*,#16550,.T.);
#23243=ORIENTED_EDGE('',*,*,#16546,.F.);
#23244=ORIENTED_EDGE('',*,*,#16551,.T.);
#23245=ORIENTED_EDGE('',*,*,#16552,.T.);
#23246=ORIENTED_EDGE('',*,*,#16553,.T.);
#23247=ORIENTED_EDGE('',*,*,#16549,.F.);
#23248=ORIENTED_EDGE('',*,*,#16554,.T.);
#23249=ORIENTED_EDGE('',*,*,#16535,.F.);
#23250=ORIENTED_EDGE('',*,*,#16555,.T.);
#23251=ORIENTED_EDGE('',*,*,#16552,.F.);
#23252=ORIENTED_EDGE('',*,*,#16556,.T.);
#23253=ORIENTED_EDGE('',*,*,#16550,.F.);
#23254=ORIENTED_EDGE('',*,*,#16557,.F.);
#23255=ORIENTED_EDGE('',*,*,#16558,.F.);
#23256=ORIENTED_EDGE('',*,*,#16559,.F.);
#23257=ORIENTED_EDGE('',*,*,#16553,.F.);
#23258=ORIENTED_EDGE('',*,*,#16560,.T.);
#23259=ORIENTED_EDGE('',*,*,#16561,.F.);
#23260=ORIENTED_EDGE('',*,*,#16557,.T.);
#23261=ORIENTED_EDGE('',*,*,#16555,.F.);
#23262=ORIENTED_EDGE('',*,*,#16562,.F.);
#23263=ORIENTED_EDGE('',*,*,#16563,.F.);
#23264=ORIENTED_EDGE('',*,*,#16560,.F.);
#23265=ORIENTED_EDGE('',*,*,#16534,.F.);
#23266=ORIENTED_EDGE('',*,*,#16564,.T.);
#23267=ORIENTED_EDGE('',*,*,#16565,.F.);
#23268=ORIENTED_EDGE('',*,*,#16562,.T.);
#23269=ORIENTED_EDGE('',*,*,#16536,.F.);
#23270=ORIENTED_EDGE('',*,*,#16556,.F.);
#23271=ORIENTED_EDGE('',*,*,#16554,.F.);
#23272=ORIENTED_EDGE('',*,*,#16551,.F.);
#23273=ORIENTED_EDGE('',*,*,#16548,.F.);
#23274=ORIENTED_EDGE('',*,*,#16545,.F.);
#23275=ORIENTED_EDGE('',*,*,#16542,.F.);
#23276=ORIENTED_EDGE('',*,*,#16539,.F.);
#23277=ORIENTED_EDGE('',*,*,#16566,.F.);
#23278=ORIENTED_EDGE('',*,*,#16567,.F.);
#23279=ORIENTED_EDGE('',*,*,#16528,.F.);
#23280=ORIENTED_EDGE('',*,*,#16568,.F.);
#23281=ORIENTED_EDGE('',*,*,#16569,.F.);
#23282=ORIENTED_EDGE('',*,*,#16530,.F.);
#23283=ORIENTED_EDGE('',*,*,#16517,.F.);
#23284=ORIENTED_EDGE('',*,*,#16522,.F.);
#23285=ORIENTED_EDGE('',*,*,#16570,.F.);
#23286=ORIENTED_EDGE('',*,*,#16571,.F.);
#23287=ORIENTED_EDGE('',*,*,#16527,.F.);
#23288=ORIENTED_EDGE('',*,*,#16572,.T.);
#23289=ORIENTED_EDGE('',*,*,#16573,.T.);
#23290=ORIENTED_EDGE('',*,*,#16574,.T.);
#23291=ORIENTED_EDGE('',*,*,#16568,.T.);
#23292=ORIENTED_EDGE('',*,*,#16526,.F.);
#23293=ORIENTED_EDGE('',*,*,#16509,.T.);
#23294=ORIENTED_EDGE('',*,*,#16506,.T.);
#23295=ORIENTED_EDGE('',*,*,#16575,.T.);
#23296=ORIENTED_EDGE('',*,*,#16572,.F.);
#23297=ORIENTED_EDGE('',*,*,#16573,.F.);
#23298=ORIENTED_EDGE('',*,*,#16575,.F.);
#23299=ORIENTED_EDGE('',*,*,#16505,.T.);
#23300=ORIENTED_EDGE('',*,*,#16485,.T.);
#23301=ORIENTED_EDGE('',*,*,#16500,.F.);
#23302=ORIENTED_EDGE('',*,*,#16501,.T.);
#23303=ORIENTED_EDGE('',*,*,#16414,.F.);
#23304=ORIENTED_EDGE('',*,*,#16410,.T.);
#23305=ORIENTED_EDGE('',*,*,#16406,.F.);
#23306=ORIENTED_EDGE('',*,*,#16495,.T.);
#23307=ORIENTED_EDGE('',*,*,#16478,.T.);
#23308=ORIENTED_EDGE('',*,*,#16482,.T.);
#23309=ORIENTED_EDGE('',*,*,#16507,.T.);
#23310=ORIENTED_EDGE('',*,*,#16576,.F.);
#23311=ORIENTED_EDGE('',*,*,#16577,.F.);
#23312=ORIENTED_EDGE('',*,*,#16578,.F.);
#23313=ORIENTED_EDGE('',*,*,#16579,.F.);
#23314=ORIENTED_EDGE('',*,*,#16580,.F.);
#23315=ORIENTED_EDGE('',*,*,#16518,.F.);
#23316=ORIENTED_EDGE('',*,*,#16571,.T.);
#23317=ORIENTED_EDGE('',*,*,#16581,.T.);
#23318=ORIENTED_EDGE('',*,*,#16577,.T.);
#23319=ORIENTED_EDGE('',*,*,#16582,.T.);
#23320=ORIENTED_EDGE('',*,*,#16514,.F.);
#23321=ORIENTED_EDGE('',*,*,#16582,.F.);
#23322=ORIENTED_EDGE('',*,*,#16576,.T.);
#23323=ORIENTED_EDGE('',*,*,#16508,.F.);
#23324=ORIENTED_EDGE('',*,*,#16513,.T.);
#23325=ORIENTED_EDGE('',*,*,#16458,.F.);
#23326=ORIENTED_EDGE('',*,*,#16583,.T.);
#23327=ORIENTED_EDGE('',*,*,#16584,.T.);
#23328=ORIENTED_EDGE('',*,*,#16585,.T.);
#23329=ORIENTED_EDGE('',*,*,#16586,.T.);
#23330=ORIENTED_EDGE('',*,*,#16457,.F.);
#23331=ORIENTED_EDGE('',*,*,#16451,.T.);
#23332=ORIENTED_EDGE('',*,*,#16439,.T.);
#23333=ORIENTED_EDGE('',*,*,#16587,.T.);
#23334=ORIENTED_EDGE('',*,*,#16583,.F.);
#23335=ORIENTED_EDGE('',*,*,#16584,.F.);
#23336=ORIENTED_EDGE('',*,*,#16587,.F.);
#23337=ORIENTED_EDGE('',*,*,#16438,.T.);
#23338=ORIENTED_EDGE('',*,*,#16431,.T.);
#23339=ORIENTED_EDGE('',*,*,#16428,.F.);
#23340=ORIENTED_EDGE('',*,*,#16588,.T.);
#23341=ORIENTED_EDGE('',*,*,#16418,.F.);
#23342=ORIENTED_EDGE('',*,*,#16422,.T.);
#23343=ORIENTED_EDGE('',*,*,#16423,.F.);
#23344=ORIENTED_EDGE('',*,*,#16450,.T.);
#23345=ORIENTED_EDGE('',*,*,#16440,.T.);
#23346=ORIENTED_EDGE('',*,*,#16435,.T.);
#23347=ORIENTED_EDGE('',*,*,#16444,.T.);
#23348=ORIENTED_EDGE('',*,*,#16473,.F.);
#23349=ORIENTED_EDGE('',*,*,#16476,.F.);
#23350=ORIENTED_EDGE('',*,*,#16589,.F.);
#23351=ORIENTED_EDGE('',*,*,#16590,.F.);
#23352=ORIENTED_EDGE('',*,*,#16591,.F.);
#23353=ORIENTED_EDGE('',*,*,#16470,.F.);
#23354=ORIENTED_EDGE('',*,*,#16592,.F.);
#23355=ORIENTED_EDGE('',*,*,#16593,.F.);
#23356=ORIENTED_EDGE('',*,*,#16474,.F.);
#23357=ORIENTED_EDGE('',*,*,#16469,.F.);
#23358=ORIENTED_EDGE('',*,*,#16463,.T.);
#23359=ORIENTED_EDGE('',*,*,#16594,.T.);
#23360=ORIENTED_EDGE('',*,*,#16595,.T.);
#23361=ORIENTED_EDGE('',*,*,#16592,.T.);
#23362=ORIENTED_EDGE('',*,*,#16459,.F.);
#23363=ORIENTED_EDGE('',*,*,#16586,.F.);
#23364=ORIENTED_EDGE('',*,*,#16596,.F.);
#23365=ORIENTED_EDGE('',*,*,#16465,.F.);
#23366=ORIENTED_EDGE('',*,*,#16597,.T.);
#23367=ORIENTED_EDGE('',*,*,#16598,.T.);
#23368=ORIENTED_EDGE('',*,*,#16599,.T.);
#23369=ORIENTED_EDGE('',*,*,#16598,.F.);
#23370=ORIENTED_EDGE('',*,*,#16600,.F.);
#23371=ORIENTED_EDGE('',*,*,#16601,.T.);
#23372=ORIENTED_EDGE('',*,*,#16599,.F.);
#23373=ORIENTED_EDGE('',*,*,#16601,.F.);
#23374=ORIENTED_EDGE('',*,*,#16467,.F.);
#23375=ORIENTED_EDGE('',*,*,#16602,.F.);
#23376=ORIENTED_EDGE('',*,*,#16594,.F.);
#23377=ORIENTED_EDGE('',*,*,#16462,.F.);
#23378=ORIENTED_EDGE('',*,*,#16603,.F.);
#23379=ORIENTED_EDGE('',*,*,#16597,.F.);
#23380=ORIENTED_EDGE('',*,*,#16590,.T.);
#23381=ORIENTED_EDGE('',*,*,#16604,.T.);
#23382=ORIENTED_EDGE('',*,*,#16600,.T.);
#23383=ORIENTED_EDGE('',*,*,#16604,.F.);
#23384=ORIENTED_EDGE('',*,*,#16579,.T.);
#23385=ORIENTED_EDGE('',*,*,#16605,.T.);
#23386=ORIENTED_EDGE('',*,*,#16606,.T.);
#23387=ORIENTED_EDGE('',*,*,#16605,.F.);
#23388=ORIENTED_EDGE('',*,*,#16607,.F.);
#23389=ORIENTED_EDGE('',*,*,#16608,.T.);
#23390=ORIENTED_EDGE('',*,*,#16606,.F.);
#23391=ORIENTED_EDGE('',*,*,#16608,.F.);
#23392=ORIENTED_EDGE('',*,*,#16609,.T.);
#23393=ORIENTED_EDGE('',*,*,#16610,.T.);
#23394=ORIENTED_EDGE('',*,*,#16607,.T.);
#23395=ORIENTED_EDGE('',*,*,#16610,.F.);
#23396=ORIENTED_EDGE('',*,*,#16532,.F.);
#23397=ORIENTED_EDGE('',*,*,#16611,.F.);
#23398=ORIENTED_EDGE('',*,*,#16520,.F.);
#23399=ORIENTED_EDGE('',*,*,#16525,.F.);
#23400=ORIENTED_EDGE('',*,*,#16612,.F.);
#23401=ORIENTED_EDGE('',*,*,#16609,.F.);
#23402=ORIENTED_EDGE('',*,*,#16603,.T.);
#23403=ORIENTED_EDGE('',*,*,#16613,.T.);
#23404=ORIENTED_EDGE('',*,*,#16614,.T.);
#23405=ORIENTED_EDGE('',*,*,#16613,.F.);
#23406=ORIENTED_EDGE('',*,*,#16615,.F.);
#23407=ORIENTED_EDGE('',*,*,#16616,.T.);
#23408=ORIENTED_EDGE('',*,*,#16614,.F.);
#23409=ORIENTED_EDGE('',*,*,#16616,.F.);
#23410=ORIENTED_EDGE('',*,*,#16591,.T.);
#23411=ORIENTED_EDGE('',*,*,#16617,.T.);
#23412=ORIENTED_EDGE('',*,*,#16615,.T.);
#23413=ORIENTED_EDGE('',*,*,#16617,.F.);
#23414=ORIENTED_EDGE('',*,*,#16580,.T.);
#23415=ORIENTED_EDGE('',*,*,#16618,.T.);
#23416=ORIENTED_EDGE('',*,*,#16619,.T.);
#23417=ORIENTED_EDGE('',*,*,#16618,.F.);
#23418=ORIENTED_EDGE('',*,*,#16620,.F.);
#23419=ORIENTED_EDGE('',*,*,#16621,.T.);
#23420=ORIENTED_EDGE('',*,*,#16619,.F.);
#23421=ORIENTED_EDGE('',*,*,#16621,.F.);
#23422=ORIENTED_EDGE('',*,*,#16612,.T.);
#23423=ORIENTED_EDGE('',*,*,#16622,.T.);
#23424=ORIENTED_EDGE('',*,*,#16620,.T.);
#23425=ORIENTED_EDGE('',*,*,#16622,.F.);
#23426=ORIENTED_EDGE('',*,*,#16566,.T.);
#23427=ORIENTED_EDGE('',*,*,#16623,.T.);
#23428=ORIENTED_EDGE('',*,*,#16624,.T.);
#23429=ORIENTED_EDGE('',*,*,#16623,.F.);
#23430=ORIENTED_EDGE('',*,*,#16624,.F.);
#23431=ORIENTED_EDGE('',*,*,#16625,.T.);
#23432=ORIENTED_EDGE('',*,*,#16626,.F.);
#23433=ORIENTED_EDGE('',*,*,#16625,.F.);
#23434=ORIENTED_EDGE('',*,*,#16567,.T.);
#23435=ORIENTED_EDGE('',*,*,#16627,.T.);
#23436=ORIENTED_EDGE('',*,*,#16628,.T.);
#23437=ORIENTED_EDGE('',*,*,#16627,.F.);
#23438=ORIENTED_EDGE('',*,*,#16628,.F.);
#23439=ORIENTED_EDGE('',*,*,#16629,.T.);
#23440=ORIENTED_EDGE('',*,*,#16630,.F.);
#23441=ORIENTED_EDGE('',*,*,#16629,.F.);
#23442=ORIENTED_EDGE('',*,*,#16447,.T.);
#23443=ORIENTED_EDGE('',*,*,#16631,.T.);
#23444=ORIENTED_EDGE('',*,*,#16632,.T.);
#23445=ORIENTED_EDGE('',*,*,#16633,.T.);
#23446=ORIENTED_EDGE('',*,*,#16634,.T.);
#23447=ORIENTED_EDGE('',*,*,#16635,.T.);
#23448=ORIENTED_EDGE('',*,*,#16632,.F.);
#23449=ORIENTED_EDGE('',*,*,#16636,.T.);
#23450=ORIENTED_EDGE('',*,*,#16637,.T.);
#23451=ORIENTED_EDGE('',*,*,#16638,.T.);
#23452=ORIENTED_EDGE('',*,*,#16634,.F.);
#23453=ORIENTED_EDGE('',*,*,#16639,.T.);
#23454=ORIENTED_EDGE('',*,*,#16640,.T.);
#23455=ORIENTED_EDGE('',*,*,#16641,.T.);
#23456=ORIENTED_EDGE('',*,*,#16637,.F.);
#23457=ORIENTED_EDGE('',*,*,#16642,.T.);
#23458=ORIENTED_EDGE('',*,*,#16503,.F.);
#23459=ORIENTED_EDGE('',*,*,#16643,.T.);
#23460=ORIENTED_EDGE('',*,*,#16640,.F.);
#23461=ORIENTED_EDGE('',*,*,#16644,.T.);
#23462=ORIENTED_EDGE('',*,*,#16644,.F.);
#23463=ORIENTED_EDGE('',*,*,#16642,.F.);
#23464=ORIENTED_EDGE('',*,*,#16639,.F.);
#23465=ORIENTED_EDGE('',*,*,#16636,.F.);
#23466=ORIENTED_EDGE('',*,*,#16631,.F.);
#23467=ORIENTED_EDGE('',*,*,#16446,.T.);
#23468=ORIENTED_EDGE('',*,*,#16424,.F.);
#23469=ORIENTED_EDGE('',*,*,#16420,.T.);
#23470=ORIENTED_EDGE('',*,*,#16416,.F.);
#23471=ORIENTED_EDGE('',*,*,#16645,.T.);
#23472=ORIENTED_EDGE('',*,*,#16646,.F.);
#23473=ORIENTED_EDGE('',*,*,#16647,.F.);
#23474=ORIENTED_EDGE('',*,*,#16648,.F.);
#23475=ORIENTED_EDGE('',*,*,#16649,.F.);
#23476=ORIENTED_EDGE('',*,*,#16650,.F.);
#23477=ORIENTED_EDGE('',*,*,#16491,.T.);
#23478=ORIENTED_EDGE('',*,*,#16408,.F.);
#23479=ORIENTED_EDGE('',*,*,#16412,.T.);
#23480=ORIENTED_EDGE('',*,*,#16413,.F.);
#23481=ORIENTED_EDGE('',*,*,#16504,.T.);
#23482=ORIENTED_EDGE('',*,*,#16651,.F.);
#23483=ORIENTED_EDGE('',*,*,#16578,.T.);
#23484=ORIENTED_EDGE('',*,*,#16581,.F.);
#23485=ORIENTED_EDGE('',*,*,#16570,.T.);
#23486=ORIENTED_EDGE('',*,*,#16521,.F.);
#23487=ORIENTED_EDGE('',*,*,#16611,.T.);
#23488=ORIENTED_EDGE('',*,*,#16531,.F.);
#23489=ORIENTED_EDGE('',*,*,#16569,.T.);
#23490=ORIENTED_EDGE('',*,*,#16574,.F.);
#23491=ORIENTED_EDGE('',*,*,#16593,.T.);
#23492=ORIENTED_EDGE('',*,*,#16595,.F.);
#23493=ORIENTED_EDGE('',*,*,#16602,.T.);
#23494=ORIENTED_EDGE('',*,*,#16466,.F.);
#23495=ORIENTED_EDGE('',*,*,#16596,.T.);
#23496=ORIENTED_EDGE('',*,*,#16585,.F.);
#23497=ORIENTED_EDGE('',*,*,#16589,.T.);
#23498=ORIENTED_EDGE('',*,*,#16475,.F.);
#23499=ORIENTED_EDGE('',*,*,#16652,.F.);
#23500=ORIENTED_EDGE('',*,*,#16492,.T.);
#23501=ORIENTED_EDGE('',*,*,#16650,.T.);
#23502=ORIENTED_EDGE('',*,*,#16653,.T.);
#23503=ORIENTED_EDGE('',*,*,#16654,.T.);
#23504=ORIENTED_EDGE('',*,*,#16655,.T.);
#23505=ORIENTED_EDGE('',*,*,#16656,.T.);
#23506=ORIENTED_EDGE('',*,*,#16653,.F.);
#23507=ORIENTED_EDGE('',*,*,#16649,.T.);
#23508=ORIENTED_EDGE('',*,*,#16657,.T.);
#23509=ORIENTED_EDGE('',*,*,#16658,.T.);
#23510=ORIENTED_EDGE('',*,*,#16655,.F.);
#23511=ORIENTED_EDGE('',*,*,#16648,.T.);
#23512=ORIENTED_EDGE('',*,*,#16659,.T.);
#23513=ORIENTED_EDGE('',*,*,#16660,.T.);
#23514=ORIENTED_EDGE('',*,*,#16657,.F.);
#23515=ORIENTED_EDGE('',*,*,#16647,.T.);
#23516=ORIENTED_EDGE('',*,*,#16661,.F.);
#23517=ORIENTED_EDGE('',*,*,#16662,.T.);
#23518=ORIENTED_EDGE('',*,*,#16659,.F.);
#23519=ORIENTED_EDGE('',*,*,#16646,.T.);
#23520=ORIENTED_EDGE('',*,*,#16652,.T.);
#23521=ORIENTED_EDGE('',*,*,#16663,.T.);
#23522=ORIENTED_EDGE('',*,*,#16630,.T.);
#23523=ORIENTED_EDGE('',*,*,#16663,.F.);
#23524=ORIENTED_EDGE('',*,*,#16651,.T.);
#23525=ORIENTED_EDGE('',*,*,#16664,.T.);
#23526=ORIENTED_EDGE('',*,*,#16626,.T.);
#23527=ORIENTED_EDGE('',*,*,#16664,.F.);
#23528=ORIENTED_EDGE('',*,*,#16430,.F.);
#23529=ORIENTED_EDGE('',*,*,#16437,.F.);
#23530=ORIENTED_EDGE('',*,*,#16443,.F.);
#23531=ORIENTED_EDGE('',*,*,#16665,.F.);
#23532=ORIENTED_EDGE('',*,*,#16426,.F.);
#23533=ORIENTED_EDGE('',*,*,#16665,.T.);
#23534=ORIENTED_EDGE('',*,*,#16442,.F.);
#23535=ORIENTED_EDGE('',*,*,#16449,.F.);
#23536=ORIENTED_EDGE('',*,*,#16666,.F.);
#23537=ORIENTED_EDGE('',*,*,#16667,.F.);
#23538=ORIENTED_EDGE('',*,*,#16419,.F.);
#23539=ORIENTED_EDGE('',*,*,#16588,.F.);
#23540=ORIENTED_EDGE('',*,*,#16427,.F.);
#23541=ORIENTED_EDGE('',*,*,#16667,.T.);
#23542=ORIENTED_EDGE('',*,*,#16668,.T.);
#23543=ORIENTED_EDGE('',*,*,#16661,.T.);
#23544=ORIENTED_EDGE('',*,*,#16645,.F.);
#23545=ORIENTED_EDGE('',*,*,#16635,.F.);
#23546=ORIENTED_EDGE('',*,*,#16669,.T.);
#23547=ORIENTED_EDGE('',*,*,#16565,.T.);
#23548=ORIENTED_EDGE('',*,*,#16670,.T.);
#23549=ORIENTED_EDGE('',*,*,#16638,.F.);
#23550=ORIENTED_EDGE('',*,*,#16671,.T.);
#23551=ORIENTED_EDGE('',*,*,#16563,.T.);
#23552=ORIENTED_EDGE('',*,*,#16669,.F.);
#23553=ORIENTED_EDGE('',*,*,#16641,.F.);
#23554=ORIENTED_EDGE('',*,*,#16672,.T.);
#23555=ORIENTED_EDGE('',*,*,#16561,.T.);
#23556=ORIENTED_EDGE('',*,*,#16671,.F.);
#23557=ORIENTED_EDGE('',*,*,#16502,.F.);
#23558=ORIENTED_EDGE('',*,*,#16496,.T.);
#23559=ORIENTED_EDGE('',*,*,#16493,.F.);
#23560=ORIENTED_EDGE('',*,*,#16654,.F.);
#23561=ORIENTED_EDGE('',*,*,#16673,.T.);
#23562=ORIENTED_EDGE('',*,*,#16558,.T.);
#23563=ORIENTED_EDGE('',*,*,#16672,.F.);
#23564=ORIENTED_EDGE('',*,*,#16643,.F.);
#23565=ORIENTED_EDGE('',*,*,#16656,.F.);
#23566=ORIENTED_EDGE('',*,*,#16674,.T.);
#23567=ORIENTED_EDGE('',*,*,#16675,.T.);
#23568=ORIENTED_EDGE('',*,*,#16673,.F.);
#23569=ORIENTED_EDGE('',*,*,#16658,.F.);
#23570=ORIENTED_EDGE('',*,*,#16676,.T.);
#23571=ORIENTED_EDGE('',*,*,#16677,.T.);
#23572=ORIENTED_EDGE('',*,*,#16674,.F.);
#23573=ORIENTED_EDGE('',*,*,#16660,.F.);
#23574=ORIENTED_EDGE('',*,*,#16678,.T.);
#23575=ORIENTED_EDGE('',*,*,#16679,.T.);
#23576=ORIENTED_EDGE('',*,*,#16676,.F.);
#23577=ORIENTED_EDGE('',*,*,#16633,.F.);
#23578=ORIENTED_EDGE('',*,*,#16670,.F.);
#23579=ORIENTED_EDGE('',*,*,#16680,.T.);
#23580=ORIENTED_EDGE('',*,*,#16678,.F.);
#23581=ORIENTED_EDGE('',*,*,#16662,.F.);
#23582=ORIENTED_EDGE('',*,*,#16668,.F.);
#23583=ORIENTED_EDGE('',*,*,#16666,.T.);
#23584=ORIENTED_EDGE('',*,*,#16448,.F.);
#23585=ORIENTED_EDGE('',*,*,#16544,.F.);
#23586=ORIENTED_EDGE('',*,*,#16681,.F.);
#23587=ORIENTED_EDGE('',*,*,#16677,.F.);
#23588=ORIENTED_EDGE('',*,*,#16682,.F.);
#23589=ORIENTED_EDGE('',*,*,#16541,.F.);
#23590=ORIENTED_EDGE('',*,*,#16682,.T.);
#23591=ORIENTED_EDGE('',*,*,#16679,.F.);
#23592=ORIENTED_EDGE('',*,*,#16683,.T.);
#23593=ORIENTED_EDGE('',*,*,#16538,.F.);
#23594=ORIENTED_EDGE('',*,*,#16683,.F.);
#23595=ORIENTED_EDGE('',*,*,#16680,.F.);
#23596=ORIENTED_EDGE('',*,*,#16564,.F.);
#23597=ORIENTED_EDGE('',*,*,#16547,.F.);
#23598=ORIENTED_EDGE('',*,*,#16559,.T.);
#23599=ORIENTED_EDGE('',*,*,#16675,.F.);
#23600=ORIENTED_EDGE('',*,*,#16681,.T.);
#23601=ORIENTED_EDGE('',*,*,#16684,.F.);
#23602=ORIENTED_EDGE('',*,*,#16685,.T.);
#23603=ORIENTED_EDGE('',*,*,#16684,.T.);
#23604=ORIENTED_EDGE('',*,*,#16685,.F.);
#23605=ORIENTED_EDGE('',*,*,#16686,.F.);
#23606=ORIENTED_EDGE('',*,*,#16687,.F.);
#23607=ORIENTED_EDGE('',*,*,#16688,.F.);
#23608=ORIENTED_EDGE('',*,*,#16689,.F.);
#23609=ORIENTED_EDGE('',*,*,#16690,.F.);
#23610=ORIENTED_EDGE('',*,*,#16691,.F.);
#23611=ORIENTED_EDGE('',*,*,#16692,.F.);
#23612=ORIENTED_EDGE('',*,*,#16693,.F.);
#23613=ORIENTED_EDGE('',*,*,#16694,.F.);
#23614=ORIENTED_EDGE('',*,*,#16695,.F.);
#23615=ORIENTED_EDGE('',*,*,#16694,.T.);
#23616=ORIENTED_EDGE('',*,*,#16696,.T.);
#23617=ORIENTED_EDGE('',*,*,#16690,.T.);
#23618=ORIENTED_EDGE('',*,*,#16695,.T.);
#23619=ORIENTED_EDGE('',*,*,#16696,.F.);
#23620=ORIENTED_EDGE('',*,*,#16693,.T.);
#23621=ORIENTED_EDGE('',*,*,#16692,.T.);
#23622=ORIENTED_EDGE('',*,*,#16697,.T.);
#23623=ORIENTED_EDGE('',*,*,#16691,.T.);
#23624=ORIENTED_EDGE('',*,*,#16697,.F.);
#23625=ORIENTED_EDGE('',*,*,#16687,.T.);
#23626=ORIENTED_EDGE('',*,*,#16698,.F.);
#23627=ORIENTED_EDGE('',*,*,#16699,.F.);
#23628=ORIENTED_EDGE('',*,*,#16700,.T.);
#23629=ORIENTED_EDGE('',*,*,#16699,.T.);
#23630=ORIENTED_EDGE('',*,*,#16700,.F.);
#23631=ORIENTED_EDGE('',*,*,#16701,.T.);
#23632=ORIENTED_EDGE('',*,*,#16702,.F.);
#23633=ORIENTED_EDGE('',*,*,#16703,.F.);
#23634=ORIENTED_EDGE('',*,*,#16704,.F.);
#23635=ORIENTED_EDGE('',*,*,#16705,.F.);
#23636=ORIENTED_EDGE('',*,*,#16706,.F.);
#23637=ORIENTED_EDGE('',*,*,#16707,.F.);
#23638=ORIENTED_EDGE('',*,*,#16708,.F.);
#23639=ORIENTED_EDGE('',*,*,#16704,.T.);
#23640=ORIENTED_EDGE('',*,*,#16709,.T.);
#23641=ORIENTED_EDGE('',*,*,#16710,.T.);
#23642=ORIENTED_EDGE('',*,*,#16703,.T.);
#23643=ORIENTED_EDGE('',*,*,#16711,.F.);
#23644=ORIENTED_EDGE('',*,*,#16709,.F.);
#23645=ORIENTED_EDGE('',*,*,#16702,.T.);
#23646=ORIENTED_EDGE('',*,*,#16701,.F.);
#23647=ORIENTED_EDGE('',*,*,#16707,.T.);
#23648=ORIENTED_EDGE('',*,*,#16712,.F.);
#23649=ORIENTED_EDGE('',*,*,#16711,.T.);
#23650=ORIENTED_EDGE('',*,*,#16688,.T.);
#23651=ORIENTED_EDGE('',*,*,#16698,.T.);
#23652=ORIENTED_EDGE('',*,*,#16686,.T.);
#23653=ORIENTED_EDGE('',*,*,#16713,.T.);
#23654=ORIENTED_EDGE('',*,*,#16705,.T.);
#23655=ORIENTED_EDGE('',*,*,#16710,.F.);
#23656=ORIENTED_EDGE('',*,*,#16712,.T.);
#23657=ORIENTED_EDGE('',*,*,#16706,.T.);
#23658=ORIENTED_EDGE('',*,*,#16713,.F.);
#23659=ORIENTED_EDGE('',*,*,#16689,.T.);
#23660=ORIENTED_EDGE('',*,*,#16708,.T.);
#23661=ORIENTED_EDGE('',*,*,#16714,.F.);
#23662=ORIENTED_EDGE('',*,*,#16715,.T.);
#23663=ORIENTED_EDGE('',*,*,#16716,.T.);
#23664=ORIENTED_EDGE('',*,*,#16717,.T.);
#23665=ORIENTED_EDGE('',*,*,#16718,.F.);
#23666=ORIENTED_EDGE('',*,*,#16719,.T.);
#23667=ORIENTED_EDGE('',*,*,#16714,.T.);
#23668=ORIENTED_EDGE('',*,*,#16720,.T.);
#23669=ORIENTED_EDGE('',*,*,#16721,.F.);
#23670=ORIENTED_EDGE('',*,*,#16722,.T.);
#23671=ORIENTED_EDGE('',*,*,#16718,.T.);
#23672=ORIENTED_EDGE('',*,*,#16723,.T.);
#23673=ORIENTED_EDGE('',*,*,#16724,.F.);
#23674=ORIENTED_EDGE('',*,*,#16725,.T.);
#23675=ORIENTED_EDGE('',*,*,#16721,.T.);
#23676=ORIENTED_EDGE('',*,*,#16726,.T.);
#23677=ORIENTED_EDGE('',*,*,#16727,.F.);
#23678=ORIENTED_EDGE('',*,*,#16728,.T.);
#23679=ORIENTED_EDGE('',*,*,#16724,.T.);
#23680=ORIENTED_EDGE('',*,*,#16729,.T.);
#23681=ORIENTED_EDGE('',*,*,#16730,.F.);
#23682=ORIENTED_EDGE('',*,*,#16731,.T.);
#23683=ORIENTED_EDGE('',*,*,#16727,.T.);
#23684=ORIENTED_EDGE('',*,*,#16732,.T.);
#23685=ORIENTED_EDGE('',*,*,#16733,.F.);
#23686=ORIENTED_EDGE('',*,*,#16734,.T.);
#23687=ORIENTED_EDGE('',*,*,#16730,.T.);
#23688=ORIENTED_EDGE('',*,*,#16735,.T.);
#23689=ORIENTED_EDGE('',*,*,#16736,.F.);
#23690=ORIENTED_EDGE('',*,*,#16737,.T.);
#23691=ORIENTED_EDGE('',*,*,#16733,.T.);
#23692=ORIENTED_EDGE('',*,*,#16738,.T.);
#23693=ORIENTED_EDGE('',*,*,#16739,.F.);
#23694=ORIENTED_EDGE('',*,*,#16740,.T.);
#23695=ORIENTED_EDGE('',*,*,#16736,.T.);
#23696=ORIENTED_EDGE('',*,*,#16741,.T.);
#23697=ORIENTED_EDGE('',*,*,#16742,.F.);
#23698=ORIENTED_EDGE('',*,*,#16743,.T.);
#23699=ORIENTED_EDGE('',*,*,#16739,.T.);
#23700=ORIENTED_EDGE('',*,*,#16744,.T.);
#23701=ORIENTED_EDGE('',*,*,#16745,.F.);
#23702=ORIENTED_EDGE('',*,*,#16746,.T.);
#23703=ORIENTED_EDGE('',*,*,#16742,.T.);
#23704=ORIENTED_EDGE('',*,*,#16747,.T.);
#23705=ORIENTED_EDGE('',*,*,#16748,.F.);
#23706=ORIENTED_EDGE('',*,*,#16749,.T.);
#23707=ORIENTED_EDGE('',*,*,#16750,.T.);
#23708=ORIENTED_EDGE('',*,*,#16751,.F.);
#23709=ORIENTED_EDGE('',*,*,#16752,.F.);
#23710=ORIENTED_EDGE('',*,*,#16753,.T.);
#23711=ORIENTED_EDGE('',*,*,#16748,.T.);
#23712=ORIENTED_EDGE('',*,*,#16754,.F.);
#23713=ORIENTED_EDGE('',*,*,#16755,.F.);
#23714=ORIENTED_EDGE('',*,*,#16756,.T.);
#23715=ORIENTED_EDGE('',*,*,#16752,.T.);
#23716=ORIENTED_EDGE('',*,*,#16757,.F.);
#23717=ORIENTED_EDGE('',*,*,#16758,.F.);
#23718=ORIENTED_EDGE('',*,*,#16759,.T.);
#23719=ORIENTED_EDGE('',*,*,#16755,.T.);
#23720=ORIENTED_EDGE('',*,*,#16760,.F.);
#23721=ORIENTED_EDGE('',*,*,#16761,.F.);
#23722=ORIENTED_EDGE('',*,*,#16762,.T.);
#23723=ORIENTED_EDGE('',*,*,#16758,.T.);
#23724=ORIENTED_EDGE('',*,*,#16763,.F.);
#23725=ORIENTED_EDGE('',*,*,#16764,.F.);
#23726=ORIENTED_EDGE('',*,*,#16765,.T.);
#23727=ORIENTED_EDGE('',*,*,#16761,.T.);
#23728=ORIENTED_EDGE('',*,*,#16766,.F.);
#23729=ORIENTED_EDGE('',*,*,#16767,.F.);
#23730=ORIENTED_EDGE('',*,*,#16768,.T.);
#23731=ORIENTED_EDGE('',*,*,#16764,.T.);
#23732=ORIENTED_EDGE('',*,*,#16769,.F.);
#23733=ORIENTED_EDGE('',*,*,#16770,.F.);
#23734=ORIENTED_EDGE('',*,*,#16771,.T.);
#23735=ORIENTED_EDGE('',*,*,#16767,.T.);
#23736=ORIENTED_EDGE('',*,*,#16772,.F.);
#23737=ORIENTED_EDGE('',*,*,#16773,.F.);
#23738=ORIENTED_EDGE('',*,*,#16774,.T.);
#23739=ORIENTED_EDGE('',*,*,#16770,.T.);
#23740=ORIENTED_EDGE('',*,*,#16775,.F.);
#23741=ORIENTED_EDGE('',*,*,#16776,.F.);
#23742=ORIENTED_EDGE('',*,*,#16777,.T.);
#23743=ORIENTED_EDGE('',*,*,#16773,.T.);
#23744=ORIENTED_EDGE('',*,*,#16778,.F.);
#23745=ORIENTED_EDGE('',*,*,#16779,.F.);
#23746=ORIENTED_EDGE('',*,*,#16780,.T.);
#23747=ORIENTED_EDGE('',*,*,#16776,.T.);
#23748=ORIENTED_EDGE('',*,*,#16781,.F.);
#23749=ORIENTED_EDGE('',*,*,#16782,.F.);
#23750=ORIENTED_EDGE('',*,*,#16783,.F.);
#23751=ORIENTED_EDGE('',*,*,#16784,.F.);
#23752=ORIENTED_EDGE('',*,*,#16785,.F.);
#23753=ORIENTED_EDGE('',*,*,#16786,.F.);
#23754=ORIENTED_EDGE('',*,*,#16787,.F.);
#23755=ORIENTED_EDGE('',*,*,#16788,.F.);
#23756=ORIENTED_EDGE('',*,*,#16789,.T.);
#23757=ORIENTED_EDGE('',*,*,#16788,.T.);
#23758=ORIENTED_EDGE('',*,*,#16790,.F.);
#23759=ORIENTED_EDGE('',*,*,#16791,.F.);
#23760=ORIENTED_EDGE('',*,*,#16792,.F.);
#23761=ORIENTED_EDGE('',*,*,#16793,.F.);
#23762=ORIENTED_EDGE('',*,*,#16794,.F.);
#23763=ORIENTED_EDGE('',*,*,#16782,.T.);
#23764=ORIENTED_EDGE('',*,*,#16789,.F.);
#23765=ORIENTED_EDGE('',*,*,#16795,.T.);
#23766=ORIENTED_EDGE('',*,*,#16785,.T.);
#23767=ORIENTED_EDGE('',*,*,#16796,.T.);
#23768=ORIENTED_EDGE('',*,*,#16792,.T.);
#23769=ORIENTED_EDGE('',*,*,#16797,.T.);
#23770=ORIENTED_EDGE('',*,*,#16783,.T.);
#23771=ORIENTED_EDGE('',*,*,#16794,.T.);
#23772=ORIENTED_EDGE('',*,*,#16798,.T.);
#23773=ORIENTED_EDGE('',*,*,#16784,.T.);
#23774=ORIENTED_EDGE('',*,*,#16798,.F.);
#23775=ORIENTED_EDGE('',*,*,#16793,.T.);
#23776=ORIENTED_EDGE('',*,*,#16796,.F.);
#23777=ORIENTED_EDGE('',*,*,#16786,.T.);
#23778=ORIENTED_EDGE('',*,*,#16797,.F.);
#23779=ORIENTED_EDGE('',*,*,#16791,.T.);
#23780=ORIENTED_EDGE('',*,*,#16799,.F.);
#23781=ORIENTED_EDGE('',*,*,#16790,.T.);
#23782=ORIENTED_EDGE('',*,*,#16787,.T.);
#23783=ORIENTED_EDGE('',*,*,#16799,.T.);
#23784=ORIENTED_EDGE('',*,*,#16800,.F.);
#23785=ORIENTED_EDGE('',*,*,#16801,.F.);
#23786=ORIENTED_EDGE('',*,*,#16750,.F.);
#23787=ORIENTED_EDGE('',*,*,#16802,.F.);
#23788=ORIENTED_EDGE('',*,*,#16803,.F.);
#23789=ORIENTED_EDGE('',*,*,#16804,.F.);
#23790=ORIENTED_EDGE('',*,*,#16805,.T.);
#23791=ORIENTED_EDGE('',*,*,#16800,.T.);
#23792=ORIENTED_EDGE('',*,*,#16805,.F.);
#23793=ORIENTED_EDGE('',*,*,#16795,.F.);
#23794=ORIENTED_EDGE('',*,*,#16806,.T.);
#23795=ORIENTED_EDGE('',*,*,#16804,.T.);
#23796=ORIENTED_EDGE('',*,*,#16806,.F.);
#23797=ORIENTED_EDGE('',*,*,#16802,.T.);
#23798=ORIENTED_EDGE('',*,*,#16749,.F.);
#23799=ORIENTED_EDGE('',*,*,#16753,.F.);
#23800=ORIENTED_EDGE('',*,*,#16756,.F.);
#23801=ORIENTED_EDGE('',*,*,#16759,.F.);
#23802=ORIENTED_EDGE('',*,*,#16762,.F.);
#23803=ORIENTED_EDGE('',*,*,#16765,.F.);
#23804=ORIENTED_EDGE('',*,*,#16768,.F.);
#23805=ORIENTED_EDGE('',*,*,#16771,.F.);
#23806=ORIENTED_EDGE('',*,*,#16774,.F.);
#23807=ORIENTED_EDGE('',*,*,#16777,.F.);
#23808=ORIENTED_EDGE('',*,*,#16780,.F.);
#23809=ORIENTED_EDGE('',*,*,#16807,.F.);
#23810=ORIENTED_EDGE('',*,*,#16808,.F.);
#23811=ORIENTED_EDGE('',*,*,#16715,.F.);
#23812=ORIENTED_EDGE('',*,*,#16719,.F.);
#23813=ORIENTED_EDGE('',*,*,#16722,.F.);
#23814=ORIENTED_EDGE('',*,*,#16725,.F.);
#23815=ORIENTED_EDGE('',*,*,#16728,.F.);
#23816=ORIENTED_EDGE('',*,*,#16731,.F.);
#23817=ORIENTED_EDGE('',*,*,#16734,.F.);
#23818=ORIENTED_EDGE('',*,*,#16737,.F.);
#23819=ORIENTED_EDGE('',*,*,#16740,.F.);
#23820=ORIENTED_EDGE('',*,*,#16743,.F.);
#23821=ORIENTED_EDGE('',*,*,#16746,.F.);
#23822=ORIENTED_EDGE('',*,*,#16809,.F.);
#23823=ORIENTED_EDGE('',*,*,#16779,.T.);
#23824=ORIENTED_EDGE('',*,*,#16810,.F.);
#23825=ORIENTED_EDGE('',*,*,#16811,.F.);
#23826=ORIENTED_EDGE('',*,*,#16807,.T.);
#23827=ORIENTED_EDGE('',*,*,#16801,.T.);
#23828=ORIENTED_EDGE('',*,*,#16812,.F.);
#23829=ORIENTED_EDGE('',*,*,#16747,.F.);
#23830=ORIENTED_EDGE('',*,*,#16744,.F.);
#23831=ORIENTED_EDGE('',*,*,#16741,.F.);
#23832=ORIENTED_EDGE('',*,*,#16738,.F.);
#23833=ORIENTED_EDGE('',*,*,#16735,.F.);
#23834=ORIENTED_EDGE('',*,*,#16732,.F.);
#23835=ORIENTED_EDGE('',*,*,#16729,.F.);
#23836=ORIENTED_EDGE('',*,*,#16726,.F.);
#23837=ORIENTED_EDGE('',*,*,#16723,.F.);
#23838=ORIENTED_EDGE('',*,*,#16720,.F.);
#23839=ORIENTED_EDGE('',*,*,#16717,.F.);
#23840=ORIENTED_EDGE('',*,*,#16813,.F.);
#23841=ORIENTED_EDGE('',*,*,#16810,.T.);
#23842=ORIENTED_EDGE('',*,*,#16781,.T.);
#23843=ORIENTED_EDGE('',*,*,#16778,.T.);
#23844=ORIENTED_EDGE('',*,*,#16775,.T.);
#23845=ORIENTED_EDGE('',*,*,#16772,.T.);
#23846=ORIENTED_EDGE('',*,*,#16769,.T.);
#23847=ORIENTED_EDGE('',*,*,#16766,.T.);
#23848=ORIENTED_EDGE('',*,*,#16763,.T.);
#23849=ORIENTED_EDGE('',*,*,#16760,.T.);
#23850=ORIENTED_EDGE('',*,*,#16757,.T.);
#23851=ORIENTED_EDGE('',*,*,#16754,.T.);
#23852=ORIENTED_EDGE('',*,*,#16751,.T.);
#23853=ORIENTED_EDGE('',*,*,#16814,.T.);
#23854=ORIENTED_EDGE('',*,*,#16815,.T.);
#23855=ORIENTED_EDGE('',*,*,#16808,.T.);
#23856=ORIENTED_EDGE('',*,*,#16811,.T.);
#23857=ORIENTED_EDGE('',*,*,#16813,.T.);
#23858=ORIENTED_EDGE('',*,*,#16816,.F.);
#23859=ORIENTED_EDGE('',*,*,#16814,.F.);
#23860=ORIENTED_EDGE('',*,*,#16716,.F.);
#23861=ORIENTED_EDGE('',*,*,#16815,.F.);
#23862=ORIENTED_EDGE('',*,*,#16817,.T.);
#23863=ORIENTED_EDGE('',*,*,#16816,.T.);
#23864=ORIENTED_EDGE('',*,*,#16817,.F.);
#23865=ORIENTED_EDGE('',*,*,#16745,.T.);
#23866=ORIENTED_EDGE('',*,*,#16812,.T.);
#23867=ORIENTED_EDGE('',*,*,#16803,.T.);
#23868=ORIENTED_EDGE('',*,*,#16809,.T.);
#23869=ORIENTED_EDGE('',*,*,#16818,.T.);
#23870=ORIENTED_EDGE('',*,*,#16819,.T.);
#23871=ORIENTED_EDGE('',*,*,#16820,.T.);
#23872=ORIENTED_EDGE('',*,*,#16821,.T.);
#23873=ORIENTED_EDGE('',*,*,#16822,.T.);
#23874=ORIENTED_EDGE('',*,*,#16823,.T.);
#23875=ORIENTED_EDGE('',*,*,#16822,.F.);
#23876=ORIENTED_EDGE('',*,*,#16824,.F.);
#23877=ORIENTED_EDGE('',*,*,#16825,.F.);
#23878=ORIENTED_EDGE('',*,*,#16826,.F.);
#23879=ORIENTED_EDGE('',*,*,#16821,.F.);
#23880=ORIENTED_EDGE('',*,*,#16827,.F.);
#23881=ORIENTED_EDGE('',*,*,#16828,.T.);
#23882=ORIENTED_EDGE('',*,*,#16829,.F.);
#23883=ORIENTED_EDGE('',*,*,#16830,.F.);
#23884=ORIENTED_EDGE('',*,*,#16824,.T.);
#23885=ORIENTED_EDGE('',*,*,#16820,.F.);
#23886=ORIENTED_EDGE('',*,*,#16831,.T.);
#23887=ORIENTED_EDGE('',*,*,#16832,.T.);
#23888=ORIENTED_EDGE('',*,*,#16833,.T.);
#23889=ORIENTED_EDGE('',*,*,#16834,.T.);
#23890=ORIENTED_EDGE('',*,*,#16827,.T.);
#23891=ORIENTED_EDGE('',*,*,#16819,.F.);
#23892=ORIENTED_EDGE('',*,*,#16835,.F.);
#23893=ORIENTED_EDGE('',*,*,#16836,.F.);
#23894=ORIENTED_EDGE('',*,*,#16837,.F.);
#23895=ORIENTED_EDGE('',*,*,#16838,.F.);
#23896=ORIENTED_EDGE('',*,*,#16839,.F.);
#23897=ORIENTED_EDGE('',*,*,#16840,.F.);
#23898=ORIENTED_EDGE('',*,*,#16841,.F.);
#23899=ORIENTED_EDGE('',*,*,#16842,.F.);
#23900=ORIENTED_EDGE('',*,*,#16831,.F.);
#23901=ORIENTED_EDGE('',*,*,#16834,.F.);
#23902=ORIENTED_EDGE('',*,*,#16843,.F.);
#23903=ORIENTED_EDGE('',*,*,#16844,.F.);
#23904=ORIENTED_EDGE('',*,*,#16828,.F.);
#23905=ORIENTED_EDGE('',*,*,#16845,.T.);
#23906=ORIENTED_EDGE('',*,*,#16841,.T.);
#23907=ORIENTED_EDGE('',*,*,#16846,.T.);
#23908=ORIENTED_EDGE('',*,*,#16847,.T.);
#23909=ORIENTED_EDGE('',*,*,#16848,.T.);
#23910=ORIENTED_EDGE('',*,*,#16832,.F.);
#23911=ORIENTED_EDGE('',*,*,#16842,.T.);
#23912=ORIENTED_EDGE('',*,*,#16845,.F.);
#23913=ORIENTED_EDGE('',*,*,#16849,.F.);
#23914=ORIENTED_EDGE('',*,*,#16850,.T.);
#23915=ORIENTED_EDGE('',*,*,#16851,.T.);
#23916=ORIENTED_EDGE('',*,*,#16848,.F.);
#23917=ORIENTED_EDGE('',*,*,#16852,.T.);
#23918=ORIENTED_EDGE('',*,*,#16853,.T.);
#23919=ORIENTED_EDGE('',*,*,#16854,.T.);
#23920=ORIENTED_EDGE('',*,*,#16849,.T.);
#23921=ORIENTED_EDGE('',*,*,#16855,.T.);
#23922=ORIENTED_EDGE('',*,*,#16856,.T.);
#23923=ORIENTED_EDGE('',*,*,#16857,.T.);
#23924=ORIENTED_EDGE('',*,*,#16858,.T.);
#23925=ORIENTED_EDGE('',*,*,#16859,.T.);
#23926=ORIENTED_EDGE('',*,*,#16860,.T.);
#23927=ORIENTED_EDGE('',*,*,#16856,.F.);
#23928=ORIENTED_EDGE('',*,*,#16861,.F.);
#23929=ORIENTED_EDGE('',*,*,#16862,.F.);
#23930=ORIENTED_EDGE('',*,*,#16863,.F.);
#23931=ORIENTED_EDGE('',*,*,#16855,.F.);
#23932=ORIENTED_EDGE('',*,*,#16864,.F.);
#23933=ORIENTED_EDGE('',*,*,#16839,.T.);
#23934=ORIENTED_EDGE('',*,*,#16865,.T.);
#23935=ORIENTED_EDGE('',*,*,#16866,.T.);
#23936=ORIENTED_EDGE('',*,*,#16861,.T.);
#23937=ORIENTED_EDGE('',*,*,#16860,.F.);
#23938=ORIENTED_EDGE('',*,*,#16867,.T.);
#23939=ORIENTED_EDGE('',*,*,#16846,.F.);
#23940=ORIENTED_EDGE('',*,*,#16840,.T.);
#23941=ORIENTED_EDGE('',*,*,#16864,.T.);
#23942=ORIENTED_EDGE('',*,*,#16859,.F.);
#23943=ORIENTED_EDGE('',*,*,#16868,.F.);
#23944=ORIENTED_EDGE('',*,*,#16869,.T.);
#23945=ORIENTED_EDGE('',*,*,#16867,.F.);
#23946=ORIENTED_EDGE('',*,*,#16866,.F.);
#23947=ORIENTED_EDGE('',*,*,#16870,.F.);
#23948=ORIENTED_EDGE('',*,*,#16871,.T.);
#23949=ORIENTED_EDGE('',*,*,#16872,.F.);
#23950=ORIENTED_EDGE('',*,*,#16873,.F.);
#23951=ORIENTED_EDGE('',*,*,#16862,.T.);
#23952=ORIENTED_EDGE('',*,*,#16857,.F.);
#23953=ORIENTED_EDGE('',*,*,#16863,.T.);
#23954=ORIENTED_EDGE('',*,*,#16873,.T.);
#23955=ORIENTED_EDGE('',*,*,#16874,.T.);
#23956=ORIENTED_EDGE('',*,*,#16875,.T.);
#23957=ORIENTED_EDGE('',*,*,#16876,.T.);
#23958=ORIENTED_EDGE('',*,*,#16858,.F.);
#23959=ORIENTED_EDGE('',*,*,#16876,.F.);
#23960=ORIENTED_EDGE('',*,*,#16877,.T.);
#23961=ORIENTED_EDGE('',*,*,#16878,.T.);
#23962=ORIENTED_EDGE('',*,*,#16868,.T.);
#23963=ORIENTED_EDGE('',*,*,#16853,.F.);
#23964=ORIENTED_EDGE('',*,*,#16879,.F.);
#23965=ORIENTED_EDGE('',*,*,#16880,.F.);
#23966=ORIENTED_EDGE('',*,*,#16881,.T.);
#23967=ORIENTED_EDGE('',*,*,#16879,.T.);
#23968=ORIENTED_EDGE('',*,*,#16882,.T.);
#23969=ORIENTED_EDGE('',*,*,#16878,.F.);
#23970=ORIENTED_EDGE('',*,*,#16883,.T.);
#23971=ORIENTED_EDGE('',*,*,#16884,.T.);
#23972=ORIENTED_EDGE('',*,*,#16880,.T.);
#23973=ORIENTED_EDGE('',*,*,#16885,.T.);
#23974=ORIENTED_EDGE('',*,*,#16886,.T.);
#23975=ORIENTED_EDGE('',*,*,#16874,.F.);
#23976=ORIENTED_EDGE('',*,*,#16872,.T.);
#23977=ORIENTED_EDGE('',*,*,#16887,.T.);
#23978=ORIENTED_EDGE('',*,*,#16888,.T.);
#23979=ORIENTED_EDGE('',*,*,#16889,.T.);
#23980=ORIENTED_EDGE('',*,*,#16847,.F.);
#23981=ORIENTED_EDGE('',*,*,#16869,.F.);
#23982=ORIENTED_EDGE('',*,*,#16882,.F.);
#23983=ORIENTED_EDGE('',*,*,#16852,.F.);
#23984=ORIENTED_EDGE('',*,*,#16886,.F.);
#23985=ORIENTED_EDGE('',*,*,#16890,.T.);
#23986=ORIENTED_EDGE('',*,*,#16891,.T.);
#23987=ORIENTED_EDGE('',*,*,#16829,.T.);
#23988=ORIENTED_EDGE('',*,*,#16844,.T.);
#23989=ORIENTED_EDGE('',*,*,#16892,.T.);
#23990=ORIENTED_EDGE('',*,*,#16891,.F.);
#23991=ORIENTED_EDGE('',*,*,#16893,.T.);
#23992=ORIENTED_EDGE('',*,*,#16894,.T.);
#23993=ORIENTED_EDGE('',*,*,#16895,.T.);
#23994=ORIENTED_EDGE('',*,*,#16825,.T.);
#23995=ORIENTED_EDGE('',*,*,#16830,.T.);
#23996=ORIENTED_EDGE('',*,*,#16823,.F.);
#23997=ORIENTED_EDGE('',*,*,#16826,.T.);
#23998=ORIENTED_EDGE('',*,*,#16895,.F.);
#23999=ORIENTED_EDGE('',*,*,#16896,.F.);
#24000=ORIENTED_EDGE('',*,*,#16897,.T.);
#24001=ORIENTED_EDGE('',*,*,#16898,.F.);
#24002=ORIENTED_EDGE('',*,*,#16894,.F.);
#24003=ORIENTED_EDGE('',*,*,#16899,.T.);
#24004=ORIENTED_EDGE('',*,*,#16900,.T.);
#24005=ORIENTED_EDGE('',*,*,#16901,.T.);
#24006=ORIENTED_EDGE('',*,*,#16896,.T.);
#24007=ORIENTED_EDGE('',*,*,#16902,.F.);
#24008=ORIENTED_EDGE('',*,*,#16903,.F.);
#24009=ORIENTED_EDGE('',*,*,#16904,.F.);
#24010=ORIENTED_EDGE('',*,*,#16865,.F.);
#24011=ORIENTED_EDGE('',*,*,#16838,.T.);
#24012=ORIENTED_EDGE('',*,*,#16903,.T.);
#24013=ORIENTED_EDGE('',*,*,#16905,.T.);
#24014=ORIENTED_EDGE('',*,*,#16870,.T.);
#24015=ORIENTED_EDGE('',*,*,#16888,.F.);
#24016=ORIENTED_EDGE('',*,*,#16906,.F.);
#24017=ORIENTED_EDGE('',*,*,#16907,.F.);
#24018=ORIENTED_EDGE('',*,*,#16906,.T.);
#24019=ORIENTED_EDGE('',*,*,#16908,.T.);
#24020=ORIENTED_EDGE('',*,*,#16902,.T.);
#24021=ORIENTED_EDGE('',*,*,#16909,.T.);
#24022=ORIENTED_EDGE('',*,*,#16910,.F.);
#24023=ORIENTED_EDGE('',*,*,#16911,.F.);
#24024=ORIENTED_EDGE('',*,*,#16912,.F.);
#24025=ORIENTED_EDGE('',*,*,#16836,.T.);
#24026=ORIENTED_EDGE('',*,*,#16911,.T.);
#24027=ORIENTED_EDGE('',*,*,#16913,.T.);
#24028=ORIENTED_EDGE('',*,*,#16914,.T.);
#24029=ORIENTED_EDGE('',*,*,#16818,.F.);
#24030=ORIENTED_EDGE('',*,*,#16898,.T.);
#24031=ORIENTED_EDGE('',*,*,#16915,.T.);
#24032=ORIENTED_EDGE('',*,*,#16912,.T.);
#24033=ORIENTED_EDGE('',*,*,#16835,.T.);
#24034=ORIENTED_EDGE('',*,*,#16916,.F.);
#24035=ORIENTED_EDGE('',*,*,#16900,.F.);
#24036=ORIENTED_EDGE('',*,*,#16917,.F.);
#24037=ORIENTED_EDGE('',*,*,#16918,.T.);
#24038=ORIENTED_EDGE('',*,*,#16917,.T.);
#24039=ORIENTED_EDGE('',*,*,#16919,.T.);
#24040=ORIENTED_EDGE('',*,*,#16920,.T.);
#24041=ORIENTED_EDGE('',*,*,#16910,.T.);
#24042=ORIENTED_EDGE('',*,*,#16921,.T.);
#24043=ORIENTED_EDGE('',*,*,#16916,.T.);
#24044=ORIENTED_EDGE('',*,*,#16922,.T.);
#24045=ORIENTED_EDGE('',*,*,#16923,.T.);
#24046=ORIENTED_EDGE('',*,*,#16907,.T.);
#24047=ORIENTED_EDGE('',*,*,#16924,.T.);
#24048=ORIENTED_EDGE('',*,*,#16920,.F.);
#24049=ORIENTED_EDGE('',*,*,#16925,.T.);
#24050=ORIENTED_EDGE('',*,*,#16904,.T.);
#24051=ORIENTED_EDGE('',*,*,#16837,.T.);
#24052=ORIENTED_EDGE('',*,*,#16914,.F.);
#24053=ORIENTED_EDGE('',*,*,#16905,.F.);
#24054=ORIENTED_EDGE('',*,*,#16908,.F.);
#24055=ORIENTED_EDGE('',*,*,#16887,.F.);
#24056=ORIENTED_EDGE('',*,*,#16871,.F.);
#24057=ORIENTED_EDGE('',*,*,#16875,.F.);
#24058=ORIENTED_EDGE('',*,*,#16889,.F.);
#24059=ORIENTED_EDGE('',*,*,#16923,.F.);
#24060=ORIENTED_EDGE('',*,*,#16919,.F.);
#24061=ORIENTED_EDGE('',*,*,#16899,.F.);
#24062=ORIENTED_EDGE('',*,*,#16893,.F.);
#24063=ORIENTED_EDGE('',*,*,#16890,.F.);
#24064=ORIENTED_EDGE('',*,*,#16885,.F.);
#24065=ORIENTED_EDGE('',*,*,#16881,.F.);
#24066=ORIENTED_EDGE('',*,*,#16877,.F.);
#24067=ORIENTED_EDGE('',*,*,#16913,.F.);
#24068=ORIENTED_EDGE('',*,*,#16922,.F.);
#24069=ORIENTED_EDGE('',*,*,#16918,.F.);
#24070=ORIENTED_EDGE('',*,*,#16926,.T.);
#24071=ORIENTED_EDGE('',*,*,#16925,.F.);
#24072=ORIENTED_EDGE('',*,*,#16926,.F.);
#24073=ORIENTED_EDGE('',*,*,#16924,.F.);
#24074=ORIENTED_EDGE('',*,*,#16909,.F.);
#24075=ORIENTED_EDGE('',*,*,#16915,.F.);
#24076=ORIENTED_EDGE('',*,*,#16897,.F.);
#24077=ORIENTED_EDGE('',*,*,#16901,.F.);
#24078=ORIENTED_EDGE('',*,*,#16921,.F.);
#24079=ORIENTED_EDGE('',*,*,#16833,.F.);
#24080=ORIENTED_EDGE('',*,*,#16851,.F.);
#24081=ORIENTED_EDGE('',*,*,#16927,.T.);
#24082=ORIENTED_EDGE('',*,*,#16883,.F.);
#24083=ORIENTED_EDGE('',*,*,#16892,.F.);
#24084=ORIENTED_EDGE('',*,*,#16843,.T.);
#24085=ORIENTED_EDGE('',*,*,#16884,.F.);
#24086=ORIENTED_EDGE('',*,*,#16927,.F.);
#24087=ORIENTED_EDGE('',*,*,#16850,.F.);
#24088=ORIENTED_EDGE('',*,*,#16854,.F.);
#24089=ORIENTED_EDGE('',*,*,#16928,.F.);
#24090=ORIENTED_EDGE('',*,*,#16929,.T.);
#24091=ORIENTED_EDGE('',*,*,#16930,.T.);
#24092=ORIENTED_EDGE('',*,*,#16931,.T.);
#24093=ORIENTED_EDGE('',*,*,#16932,.F.);
#24094=ORIENTED_EDGE('',*,*,#16933,.T.);
#24095=ORIENTED_EDGE('',*,*,#16928,.T.);
#24096=ORIENTED_EDGE('',*,*,#16934,.T.);
#24097=ORIENTED_EDGE('',*,*,#16935,.F.);
#24098=ORIENTED_EDGE('',*,*,#16936,.T.);
#24099=ORIENTED_EDGE('',*,*,#16932,.T.);
#24100=ORIENTED_EDGE('',*,*,#16937,.T.);
#24101=ORIENTED_EDGE('',*,*,#16938,.F.);
#24102=ORIENTED_EDGE('',*,*,#16939,.T.);
#24103=ORIENTED_EDGE('',*,*,#16935,.T.);
#24104=ORIENTED_EDGE('',*,*,#16940,.T.);
#24105=ORIENTED_EDGE('',*,*,#16941,.F.);
#24106=ORIENTED_EDGE('',*,*,#16942,.T.);
#24107=ORIENTED_EDGE('',*,*,#16938,.T.);
#24108=ORIENTED_EDGE('',*,*,#16943,.T.);
#24109=ORIENTED_EDGE('',*,*,#16944,.F.);
#24110=ORIENTED_EDGE('',*,*,#16945,.T.);
#24111=ORIENTED_EDGE('',*,*,#16941,.T.);
#24112=ORIENTED_EDGE('',*,*,#16946,.T.);
#24113=ORIENTED_EDGE('',*,*,#16947,.F.);
#24114=ORIENTED_EDGE('',*,*,#16948,.T.);
#24115=ORIENTED_EDGE('',*,*,#16944,.T.);
#24116=ORIENTED_EDGE('',*,*,#16949,.T.);
#24117=ORIENTED_EDGE('',*,*,#16950,.F.);
#24118=ORIENTED_EDGE('',*,*,#16951,.T.);
#24119=ORIENTED_EDGE('',*,*,#16947,.T.);
#24120=ORIENTED_EDGE('',*,*,#16952,.T.);
#24121=ORIENTED_EDGE('',*,*,#16953,.F.);
#24122=ORIENTED_EDGE('',*,*,#16954,.T.);
#24123=ORIENTED_EDGE('',*,*,#16950,.T.);
#24124=ORIENTED_EDGE('',*,*,#16955,.T.);
#24125=ORIENTED_EDGE('',*,*,#16956,.F.);
#24126=ORIENTED_EDGE('',*,*,#16957,.T.);
#24127=ORIENTED_EDGE('',*,*,#16953,.T.);
#24128=ORIENTED_EDGE('',*,*,#16958,.T.);
#24129=ORIENTED_EDGE('',*,*,#16959,.F.);
#24130=ORIENTED_EDGE('',*,*,#16960,.T.);
#24131=ORIENTED_EDGE('',*,*,#16956,.T.);
#24132=ORIENTED_EDGE('',*,*,#16961,.T.);
#24133=ORIENTED_EDGE('',*,*,#16962,.F.);
#24134=ORIENTED_EDGE('',*,*,#16963,.T.);
#24135=ORIENTED_EDGE('',*,*,#16959,.T.);
#24136=ORIENTED_EDGE('',*,*,#16964,.T.);
#24137=ORIENTED_EDGE('',*,*,#16965,.F.);
#24138=ORIENTED_EDGE('',*,*,#16966,.T.);
#24139=ORIENTED_EDGE('',*,*,#16962,.T.);
#24140=ORIENTED_EDGE('',*,*,#16967,.T.);
#24141=ORIENTED_EDGE('',*,*,#16968,.F.);
#24142=ORIENTED_EDGE('',*,*,#16969,.T.);
#24143=ORIENTED_EDGE('',*,*,#16965,.T.);
#24144=ORIENTED_EDGE('',*,*,#16970,.T.);
#24145=ORIENTED_EDGE('',*,*,#16971,.F.);
#24146=ORIENTED_EDGE('',*,*,#16972,.T.);
#24147=ORIENTED_EDGE('',*,*,#16968,.T.);
#24148=ORIENTED_EDGE('',*,*,#16973,.T.);
#24149=ORIENTED_EDGE('',*,*,#16974,.F.);
#24150=ORIENTED_EDGE('',*,*,#16975,.T.);
#24151=ORIENTED_EDGE('',*,*,#16971,.T.);
#24152=ORIENTED_EDGE('',*,*,#16976,.T.);
#24153=ORIENTED_EDGE('',*,*,#16977,.F.);
#24154=ORIENTED_EDGE('',*,*,#16978,.T.);
#24155=ORIENTED_EDGE('',*,*,#16974,.T.);
#24156=ORIENTED_EDGE('',*,*,#16979,.T.);
#24157=ORIENTED_EDGE('',*,*,#16980,.F.);
#24158=ORIENTED_EDGE('',*,*,#16981,.T.);
#24159=ORIENTED_EDGE('',*,*,#16977,.T.);
#24160=ORIENTED_EDGE('',*,*,#16982,.T.);
#24161=ORIENTED_EDGE('',*,*,#16983,.F.);
#24162=ORIENTED_EDGE('',*,*,#16984,.T.);
#24163=ORIENTED_EDGE('',*,*,#16980,.T.);
#24164=ORIENTED_EDGE('',*,*,#16985,.T.);
#24165=ORIENTED_EDGE('',*,*,#16986,.F.);
#24166=ORIENTED_EDGE('',*,*,#16987,.T.);
#24167=ORIENTED_EDGE('',*,*,#16983,.T.);
#24168=ORIENTED_EDGE('',*,*,#16988,.T.);
#24169=ORIENTED_EDGE('',*,*,#16989,.F.);
#24170=ORIENTED_EDGE('',*,*,#16990,.T.);
#24171=ORIENTED_EDGE('',*,*,#16986,.T.);
#24172=ORIENTED_EDGE('',*,*,#16991,.T.);
#24173=ORIENTED_EDGE('',*,*,#16992,.F.);
#24174=ORIENTED_EDGE('',*,*,#16993,.T.);
#24175=ORIENTED_EDGE('',*,*,#16989,.T.);
#24176=ORIENTED_EDGE('',*,*,#16994,.T.);
#24177=ORIENTED_EDGE('',*,*,#16995,.F.);
#24178=ORIENTED_EDGE('',*,*,#16996,.T.);
#24179=ORIENTED_EDGE('',*,*,#16992,.T.);
#24180=ORIENTED_EDGE('',*,*,#16997,.T.);
#24181=ORIENTED_EDGE('',*,*,#16998,.F.);
#24182=ORIENTED_EDGE('',*,*,#16999,.T.);
#24183=ORIENTED_EDGE('',*,*,#16995,.T.);
#24184=ORIENTED_EDGE('',*,*,#17000,.T.);
#24185=ORIENTED_EDGE('',*,*,#17001,.F.);
#24186=ORIENTED_EDGE('',*,*,#17002,.T.);
#24187=ORIENTED_EDGE('',*,*,#16998,.T.);
#24188=ORIENTED_EDGE('',*,*,#17003,.T.);
#24189=ORIENTED_EDGE('',*,*,#17004,.F.);
#24190=ORIENTED_EDGE('',*,*,#17005,.T.);
#24191=ORIENTED_EDGE('',*,*,#17001,.T.);
#24192=ORIENTED_EDGE('',*,*,#17006,.T.);
#24193=ORIENTED_EDGE('',*,*,#17007,.F.);
#24194=ORIENTED_EDGE('',*,*,#17008,.T.);
#24195=ORIENTED_EDGE('',*,*,#17004,.T.);
#24196=ORIENTED_EDGE('',*,*,#17009,.T.);
#24197=ORIENTED_EDGE('',*,*,#17010,.F.);
#24198=ORIENTED_EDGE('',*,*,#17011,.T.);
#24199=ORIENTED_EDGE('',*,*,#17007,.T.);
#24200=ORIENTED_EDGE('',*,*,#17012,.T.);
#24201=ORIENTED_EDGE('',*,*,#17013,.F.);
#24202=ORIENTED_EDGE('',*,*,#17014,.T.);
#24203=ORIENTED_EDGE('',*,*,#17010,.T.);
#24204=ORIENTED_EDGE('',*,*,#17015,.T.);
#24205=ORIENTED_EDGE('',*,*,#17016,.F.);
#24206=ORIENTED_EDGE('',*,*,#17017,.T.);
#24207=ORIENTED_EDGE('',*,*,#17013,.T.);
#24208=ORIENTED_EDGE('',*,*,#17018,.T.);
#24209=ORIENTED_EDGE('',*,*,#17019,.F.);
#24210=ORIENTED_EDGE('',*,*,#17020,.T.);
#24211=ORIENTED_EDGE('',*,*,#17016,.T.);
#24212=ORIENTED_EDGE('',*,*,#17021,.T.);
#24213=ORIENTED_EDGE('',*,*,#17022,.F.);
#24214=ORIENTED_EDGE('',*,*,#17023,.T.);
#24215=ORIENTED_EDGE('',*,*,#17019,.T.);
#24216=ORIENTED_EDGE('',*,*,#17024,.T.);
#24217=ORIENTED_EDGE('',*,*,#17025,.F.);
#24218=ORIENTED_EDGE('',*,*,#17026,.T.);
#24219=ORIENTED_EDGE('',*,*,#17022,.T.);
#24220=ORIENTED_EDGE('',*,*,#17027,.T.);
#24221=ORIENTED_EDGE('',*,*,#17028,.F.);
#24222=ORIENTED_EDGE('',*,*,#17029,.T.);
#24223=ORIENTED_EDGE('',*,*,#17025,.T.);
#24224=ORIENTED_EDGE('',*,*,#17030,.T.);
#24225=ORIENTED_EDGE('',*,*,#17031,.F.);
#24226=ORIENTED_EDGE('',*,*,#17032,.T.);
#24227=ORIENTED_EDGE('',*,*,#17028,.T.);
#24228=ORIENTED_EDGE('',*,*,#17033,.T.);
#24229=ORIENTED_EDGE('',*,*,#17034,.F.);
#24230=ORIENTED_EDGE('',*,*,#17035,.T.);
#24231=ORIENTED_EDGE('',*,*,#17031,.T.);
#24232=ORIENTED_EDGE('',*,*,#17036,.T.);
#24233=ORIENTED_EDGE('',*,*,#17037,.F.);
#24234=ORIENTED_EDGE('',*,*,#17038,.T.);
#24235=ORIENTED_EDGE('',*,*,#17034,.T.);
#24236=ORIENTED_EDGE('',*,*,#17039,.T.);
#24237=ORIENTED_EDGE('',*,*,#17040,.F.);
#24238=ORIENTED_EDGE('',*,*,#17041,.T.);
#24239=ORIENTED_EDGE('',*,*,#17037,.T.);
#24240=ORIENTED_EDGE('',*,*,#17042,.T.);
#24241=ORIENTED_EDGE('',*,*,#17043,.F.);
#24242=ORIENTED_EDGE('',*,*,#17044,.T.);
#24243=ORIENTED_EDGE('',*,*,#17040,.T.);
#24244=ORIENTED_EDGE('',*,*,#17045,.T.);
#24245=ORIENTED_EDGE('',*,*,#17046,.F.);
#24246=ORIENTED_EDGE('',*,*,#17047,.T.);
#24247=ORIENTED_EDGE('',*,*,#17043,.T.);
#24248=ORIENTED_EDGE('',*,*,#17048,.T.);
#24249=ORIENTED_EDGE('',*,*,#17049,.F.);
#24250=ORIENTED_EDGE('',*,*,#17050,.T.);
#24251=ORIENTED_EDGE('',*,*,#17046,.T.);
#24252=ORIENTED_EDGE('',*,*,#17051,.T.);
#24253=ORIENTED_EDGE('',*,*,#17052,.F.);
#24254=ORIENTED_EDGE('',*,*,#17053,.T.);
#24255=ORIENTED_EDGE('',*,*,#17049,.T.);
#24256=ORIENTED_EDGE('',*,*,#17054,.T.);
#24257=ORIENTED_EDGE('',*,*,#17055,.F.);
#24258=ORIENTED_EDGE('',*,*,#17056,.T.);
#24259=ORIENTED_EDGE('',*,*,#17052,.T.);
#24260=ORIENTED_EDGE('',*,*,#17057,.T.);
#24261=ORIENTED_EDGE('',*,*,#17058,.F.);
#24262=ORIENTED_EDGE('',*,*,#17059,.T.);
#24263=ORIENTED_EDGE('',*,*,#17055,.T.);
#24264=ORIENTED_EDGE('',*,*,#17060,.T.);
#24265=ORIENTED_EDGE('',*,*,#17061,.F.);
#24266=ORIENTED_EDGE('',*,*,#17062,.T.);
#24267=ORIENTED_EDGE('',*,*,#17058,.T.);
#24268=ORIENTED_EDGE('',*,*,#17063,.T.);
#24269=ORIENTED_EDGE('',*,*,#17064,.F.);
#24270=ORIENTED_EDGE('',*,*,#17065,.T.);
#24271=ORIENTED_EDGE('',*,*,#17061,.T.);
#24272=ORIENTED_EDGE('',*,*,#17066,.T.);
#24273=ORIENTED_EDGE('',*,*,#17067,.F.);
#24274=ORIENTED_EDGE('',*,*,#17068,.T.);
#24275=ORIENTED_EDGE('',*,*,#17064,.T.);
#24276=ORIENTED_EDGE('',*,*,#17069,.T.);
#24277=ORIENTED_EDGE('',*,*,#17070,.F.);
#24278=ORIENTED_EDGE('',*,*,#17071,.T.);
#24279=ORIENTED_EDGE('',*,*,#17067,.T.);
#24280=ORIENTED_EDGE('',*,*,#17072,.T.);
#24281=ORIENTED_EDGE('',*,*,#17073,.F.);
#24282=ORIENTED_EDGE('',*,*,#17074,.T.);
#24283=ORIENTED_EDGE('',*,*,#17070,.T.);
#24284=ORIENTED_EDGE('',*,*,#17075,.T.);
#24285=ORIENTED_EDGE('',*,*,#17076,.F.);
#24286=ORIENTED_EDGE('',*,*,#17077,.T.);
#24287=ORIENTED_EDGE('',*,*,#17073,.T.);
#24288=ORIENTED_EDGE('',*,*,#17078,.T.);
#24289=ORIENTED_EDGE('',*,*,#17079,.F.);
#24290=ORIENTED_EDGE('',*,*,#17080,.T.);
#24291=ORIENTED_EDGE('',*,*,#17076,.T.);
#24292=ORIENTED_EDGE('',*,*,#17081,.T.);
#24293=ORIENTED_EDGE('',*,*,#17082,.F.);
#24294=ORIENTED_EDGE('',*,*,#17083,.T.);
#24295=ORIENTED_EDGE('',*,*,#17079,.T.);
#24296=ORIENTED_EDGE('',*,*,#17084,.T.);
#24297=ORIENTED_EDGE('',*,*,#17085,.F.);
#24298=ORIENTED_EDGE('',*,*,#17086,.T.);
#24299=ORIENTED_EDGE('',*,*,#17082,.T.);
#24300=ORIENTED_EDGE('',*,*,#17087,.T.);
#24301=ORIENTED_EDGE('',*,*,#17088,.F.);
#24302=ORIENTED_EDGE('',*,*,#17089,.T.);
#24303=ORIENTED_EDGE('',*,*,#17085,.T.);
#24304=ORIENTED_EDGE('',*,*,#17090,.T.);
#24305=ORIENTED_EDGE('',*,*,#17091,.F.);
#24306=ORIENTED_EDGE('',*,*,#17092,.T.);
#24307=ORIENTED_EDGE('',*,*,#17088,.T.);
#24308=ORIENTED_EDGE('',*,*,#17093,.T.);
#24309=ORIENTED_EDGE('',*,*,#17094,.F.);
#24310=ORIENTED_EDGE('',*,*,#17095,.T.);
#24311=ORIENTED_EDGE('',*,*,#17091,.T.);
#24312=ORIENTED_EDGE('',*,*,#17096,.T.);
#24313=ORIENTED_EDGE('',*,*,#17097,.F.);
#24314=ORIENTED_EDGE('',*,*,#17098,.T.);
#24315=ORIENTED_EDGE('',*,*,#17094,.T.);
#24316=ORIENTED_EDGE('',*,*,#17099,.T.);
#24317=ORIENTED_EDGE('',*,*,#17100,.F.);
#24318=ORIENTED_EDGE('',*,*,#17101,.T.);
#24319=ORIENTED_EDGE('',*,*,#17097,.T.);
#24320=ORIENTED_EDGE('',*,*,#17102,.T.);
#24321=ORIENTED_EDGE('',*,*,#17103,.F.);
#24322=ORIENTED_EDGE('',*,*,#17104,.T.);
#24323=ORIENTED_EDGE('',*,*,#17100,.T.);
#24324=ORIENTED_EDGE('',*,*,#17105,.T.);
#24325=ORIENTED_EDGE('',*,*,#17106,.F.);
#24326=ORIENTED_EDGE('',*,*,#17107,.F.);
#24327=ORIENTED_EDGE('',*,*,#17108,.T.);
#24328=ORIENTED_EDGE('',*,*,#17103,.T.);
#24329=ORIENTED_EDGE('',*,*,#17109,.T.);
#24330=ORIENTED_EDGE('',*,*,#17110,.F.);
#24331=ORIENTED_EDGE('',*,*,#17111,.T.);
#24332=ORIENTED_EDGE('',*,*,#17112,.F.);
#24333=ORIENTED_EDGE('',*,*,#17113,.F.);
#24334=ORIENTED_EDGE('',*,*,#17114,.F.);
#24335=ORIENTED_EDGE('',*,*,#17115,.T.);
#24336=ORIENTED_EDGE('',*,*,#17110,.T.);
#24337=ORIENTED_EDGE('',*,*,#17116,.F.);
#24338=ORIENTED_EDGE('',*,*,#17117,.F.);
#24339=ORIENTED_EDGE('',*,*,#17118,.T.);
#24340=ORIENTED_EDGE('',*,*,#17114,.T.);
#24341=ORIENTED_EDGE('',*,*,#17119,.F.);
#24342=ORIENTED_EDGE('',*,*,#17120,.F.);
#24343=ORIENTED_EDGE('',*,*,#17121,.T.);
#24344=ORIENTED_EDGE('',*,*,#17117,.T.);
#24345=ORIENTED_EDGE('',*,*,#17122,.F.);
#24346=ORIENTED_EDGE('',*,*,#17123,.F.);
#24347=ORIENTED_EDGE('',*,*,#17124,.T.);
#24348=ORIENTED_EDGE('',*,*,#17120,.T.);
#24349=ORIENTED_EDGE('',*,*,#17125,.F.);
#24350=ORIENTED_EDGE('',*,*,#17126,.F.);
#24351=ORIENTED_EDGE('',*,*,#17127,.T.);
#24352=ORIENTED_EDGE('',*,*,#17123,.T.);
#24353=ORIENTED_EDGE('',*,*,#17128,.F.);
#24354=ORIENTED_EDGE('',*,*,#17129,.F.);
#24355=ORIENTED_EDGE('',*,*,#17130,.T.);
#24356=ORIENTED_EDGE('',*,*,#17126,.T.);
#24357=ORIENTED_EDGE('',*,*,#17131,.F.);
#24358=ORIENTED_EDGE('',*,*,#17132,.F.);
#24359=ORIENTED_EDGE('',*,*,#17133,.T.);
#24360=ORIENTED_EDGE('',*,*,#17129,.T.);
#24361=ORIENTED_EDGE('',*,*,#17134,.F.);
#24362=ORIENTED_EDGE('',*,*,#17135,.F.);
#24363=ORIENTED_EDGE('',*,*,#17136,.T.);
#24364=ORIENTED_EDGE('',*,*,#17132,.T.);
#24365=ORIENTED_EDGE('',*,*,#17137,.F.);
#24366=ORIENTED_EDGE('',*,*,#17138,.F.);
#24367=ORIENTED_EDGE('',*,*,#17139,.T.);
#24368=ORIENTED_EDGE('',*,*,#17135,.T.);
#24369=ORIENTED_EDGE('',*,*,#17140,.F.);
#24370=ORIENTED_EDGE('',*,*,#17141,.F.);
#24371=ORIENTED_EDGE('',*,*,#17142,.T.);
#24372=ORIENTED_EDGE('',*,*,#17138,.T.);
#24373=ORIENTED_EDGE('',*,*,#17143,.F.);
#24374=ORIENTED_EDGE('',*,*,#17144,.F.);
#24375=ORIENTED_EDGE('',*,*,#17145,.T.);
#24376=ORIENTED_EDGE('',*,*,#17141,.T.);
#24377=ORIENTED_EDGE('',*,*,#17146,.F.);
#24378=ORIENTED_EDGE('',*,*,#17147,.F.);
#24379=ORIENTED_EDGE('',*,*,#17148,.T.);
#24380=ORIENTED_EDGE('',*,*,#17144,.T.);
#24381=ORIENTED_EDGE('',*,*,#17149,.F.);
#24382=ORIENTED_EDGE('',*,*,#17150,.F.);
#24383=ORIENTED_EDGE('',*,*,#17151,.T.);
#24384=ORIENTED_EDGE('',*,*,#17147,.T.);
#24385=ORIENTED_EDGE('',*,*,#17152,.F.);
#24386=ORIENTED_EDGE('',*,*,#17153,.F.);
#24387=ORIENTED_EDGE('',*,*,#17154,.T.);
#24388=ORIENTED_EDGE('',*,*,#17150,.T.);
#24389=ORIENTED_EDGE('',*,*,#17155,.F.);
#24390=ORIENTED_EDGE('',*,*,#17156,.F.);
#24391=ORIENTED_EDGE('',*,*,#17157,.T.);
#24392=ORIENTED_EDGE('',*,*,#17153,.T.);
#24393=ORIENTED_EDGE('',*,*,#17158,.F.);
#24394=ORIENTED_EDGE('',*,*,#17159,.F.);
#24395=ORIENTED_EDGE('',*,*,#17160,.T.);
#24396=ORIENTED_EDGE('',*,*,#17156,.T.);
#24397=ORIENTED_EDGE('',*,*,#17161,.F.);
#24398=ORIENTED_EDGE('',*,*,#17162,.F.);
#24399=ORIENTED_EDGE('',*,*,#17163,.T.);
#24400=ORIENTED_EDGE('',*,*,#17159,.T.);
#24401=ORIENTED_EDGE('',*,*,#17164,.F.);
#24402=ORIENTED_EDGE('',*,*,#17165,.F.);
#24403=ORIENTED_EDGE('',*,*,#17166,.T.);
#24404=ORIENTED_EDGE('',*,*,#17162,.T.);
#24405=ORIENTED_EDGE('',*,*,#17167,.F.);
#24406=ORIENTED_EDGE('',*,*,#17168,.F.);
#24407=ORIENTED_EDGE('',*,*,#17169,.T.);
#24408=ORIENTED_EDGE('',*,*,#17165,.T.);
#24409=ORIENTED_EDGE('',*,*,#17170,.F.);
#24410=ORIENTED_EDGE('',*,*,#17171,.F.);
#24411=ORIENTED_EDGE('',*,*,#17172,.T.);
#24412=ORIENTED_EDGE('',*,*,#17168,.T.);
#24413=ORIENTED_EDGE('',*,*,#17173,.F.);
#24414=ORIENTED_EDGE('',*,*,#17174,.F.);
#24415=ORIENTED_EDGE('',*,*,#17175,.T.);
#24416=ORIENTED_EDGE('',*,*,#17171,.T.);
#24417=ORIENTED_EDGE('',*,*,#17176,.F.);
#24418=ORIENTED_EDGE('',*,*,#17177,.F.);
#24419=ORIENTED_EDGE('',*,*,#17178,.T.);
#24420=ORIENTED_EDGE('',*,*,#17174,.T.);
#24421=ORIENTED_EDGE('',*,*,#17179,.F.);
#24422=ORIENTED_EDGE('',*,*,#17180,.F.);
#24423=ORIENTED_EDGE('',*,*,#17181,.T.);
#24424=ORIENTED_EDGE('',*,*,#17177,.T.);
#24425=ORIENTED_EDGE('',*,*,#17182,.F.);
#24426=ORIENTED_EDGE('',*,*,#17183,.F.);
#24427=ORIENTED_EDGE('',*,*,#17184,.T.);
#24428=ORIENTED_EDGE('',*,*,#17180,.T.);
#24429=ORIENTED_EDGE('',*,*,#17185,.F.);
#24430=ORIENTED_EDGE('',*,*,#17186,.F.);
#24431=ORIENTED_EDGE('',*,*,#17187,.T.);
#24432=ORIENTED_EDGE('',*,*,#17183,.T.);
#24433=ORIENTED_EDGE('',*,*,#17188,.F.);
#24434=ORIENTED_EDGE('',*,*,#17189,.F.);
#24435=ORIENTED_EDGE('',*,*,#17190,.T.);
#24436=ORIENTED_EDGE('',*,*,#17186,.T.);
#24437=ORIENTED_EDGE('',*,*,#17191,.F.);
#24438=ORIENTED_EDGE('',*,*,#17192,.F.);
#24439=ORIENTED_EDGE('',*,*,#17193,.T.);
#24440=ORIENTED_EDGE('',*,*,#17189,.T.);
#24441=ORIENTED_EDGE('',*,*,#17194,.F.);
#24442=ORIENTED_EDGE('',*,*,#17195,.F.);
#24443=ORIENTED_EDGE('',*,*,#17196,.T.);
#24444=ORIENTED_EDGE('',*,*,#17192,.T.);
#24445=ORIENTED_EDGE('',*,*,#17197,.F.);
#24446=ORIENTED_EDGE('',*,*,#17198,.F.);
#24447=ORIENTED_EDGE('',*,*,#17199,.T.);
#24448=ORIENTED_EDGE('',*,*,#17195,.T.);
#24449=ORIENTED_EDGE('',*,*,#17200,.F.);
#24450=ORIENTED_EDGE('',*,*,#17201,.F.);
#24451=ORIENTED_EDGE('',*,*,#17202,.T.);
#24452=ORIENTED_EDGE('',*,*,#17198,.T.);
#24453=ORIENTED_EDGE('',*,*,#17203,.F.);
#24454=ORIENTED_EDGE('',*,*,#17204,.F.);
#24455=ORIENTED_EDGE('',*,*,#17205,.T.);
#24456=ORIENTED_EDGE('',*,*,#17201,.T.);
#24457=ORIENTED_EDGE('',*,*,#17206,.F.);
#24458=ORIENTED_EDGE('',*,*,#17207,.F.);
#24459=ORIENTED_EDGE('',*,*,#17208,.T.);
#24460=ORIENTED_EDGE('',*,*,#17204,.T.);
#24461=ORIENTED_EDGE('',*,*,#17209,.F.);
#24462=ORIENTED_EDGE('',*,*,#17210,.F.);
#24463=ORIENTED_EDGE('',*,*,#17211,.T.);
#24464=ORIENTED_EDGE('',*,*,#17207,.T.);
#24465=ORIENTED_EDGE('',*,*,#17212,.F.);
#24466=ORIENTED_EDGE('',*,*,#17213,.F.);
#24467=ORIENTED_EDGE('',*,*,#17214,.T.);
#24468=ORIENTED_EDGE('',*,*,#17210,.T.);
#24469=ORIENTED_EDGE('',*,*,#17215,.F.);
#24470=ORIENTED_EDGE('',*,*,#17216,.F.);
#24471=ORIENTED_EDGE('',*,*,#17217,.T.);
#24472=ORIENTED_EDGE('',*,*,#17213,.T.);
#24473=ORIENTED_EDGE('',*,*,#17218,.F.);
#24474=ORIENTED_EDGE('',*,*,#17219,.F.);
#24475=ORIENTED_EDGE('',*,*,#17220,.T.);
#24476=ORIENTED_EDGE('',*,*,#17216,.T.);
#24477=ORIENTED_EDGE('',*,*,#17221,.F.);
#24478=ORIENTED_EDGE('',*,*,#17222,.F.);
#24479=ORIENTED_EDGE('',*,*,#17223,.T.);
#24480=ORIENTED_EDGE('',*,*,#17219,.T.);
#24481=ORIENTED_EDGE('',*,*,#17224,.F.);
#24482=ORIENTED_EDGE('',*,*,#17225,.F.);
#24483=ORIENTED_EDGE('',*,*,#17226,.T.);
#24484=ORIENTED_EDGE('',*,*,#17222,.T.);
#24485=ORIENTED_EDGE('',*,*,#17227,.F.);
#24486=ORIENTED_EDGE('',*,*,#17228,.F.);
#24487=ORIENTED_EDGE('',*,*,#17229,.T.);
#24488=ORIENTED_EDGE('',*,*,#17225,.T.);
#24489=ORIENTED_EDGE('',*,*,#17230,.F.);
#24490=ORIENTED_EDGE('',*,*,#17231,.F.);
#24491=ORIENTED_EDGE('',*,*,#17232,.T.);
#24492=ORIENTED_EDGE('',*,*,#17228,.T.);
#24493=ORIENTED_EDGE('',*,*,#17233,.F.);
#24494=ORIENTED_EDGE('',*,*,#17234,.F.);
#24495=ORIENTED_EDGE('',*,*,#17235,.T.);
#24496=ORIENTED_EDGE('',*,*,#17231,.T.);
#24497=ORIENTED_EDGE('',*,*,#17236,.F.);
#24498=ORIENTED_EDGE('',*,*,#17237,.F.);
#24499=ORIENTED_EDGE('',*,*,#17238,.T.);
#24500=ORIENTED_EDGE('',*,*,#17234,.T.);
#24501=ORIENTED_EDGE('',*,*,#17239,.F.);
#24502=ORIENTED_EDGE('',*,*,#17240,.F.);
#24503=ORIENTED_EDGE('',*,*,#17241,.T.);
#24504=ORIENTED_EDGE('',*,*,#17237,.T.);
#24505=ORIENTED_EDGE('',*,*,#17242,.F.);
#24506=ORIENTED_EDGE('',*,*,#17243,.F.);
#24507=ORIENTED_EDGE('',*,*,#17244,.T.);
#24508=ORIENTED_EDGE('',*,*,#17240,.T.);
#24509=ORIENTED_EDGE('',*,*,#17245,.F.);
#24510=ORIENTED_EDGE('',*,*,#17246,.F.);
#24511=ORIENTED_EDGE('',*,*,#17247,.T.);
#24512=ORIENTED_EDGE('',*,*,#17243,.T.);
#24513=ORIENTED_EDGE('',*,*,#17248,.F.);
#24514=ORIENTED_EDGE('',*,*,#17249,.F.);
#24515=ORIENTED_EDGE('',*,*,#17250,.T.);
#24516=ORIENTED_EDGE('',*,*,#17246,.T.);
#24517=ORIENTED_EDGE('',*,*,#17251,.F.);
#24518=ORIENTED_EDGE('',*,*,#17252,.F.);
#24519=ORIENTED_EDGE('',*,*,#17253,.T.);
#24520=ORIENTED_EDGE('',*,*,#17249,.T.);
#24521=ORIENTED_EDGE('',*,*,#17254,.F.);
#24522=ORIENTED_EDGE('',*,*,#17255,.F.);
#24523=ORIENTED_EDGE('',*,*,#17256,.T.);
#24524=ORIENTED_EDGE('',*,*,#17252,.T.);
#24525=ORIENTED_EDGE('',*,*,#17257,.F.);
#24526=ORIENTED_EDGE('',*,*,#17258,.F.);
#24527=ORIENTED_EDGE('',*,*,#17259,.T.);
#24528=ORIENTED_EDGE('',*,*,#17255,.T.);
#24529=ORIENTED_EDGE('',*,*,#17260,.F.);
#24530=ORIENTED_EDGE('',*,*,#17261,.F.);
#24531=ORIENTED_EDGE('',*,*,#17262,.T.);
#24532=ORIENTED_EDGE('',*,*,#17258,.T.);
#24533=ORIENTED_EDGE('',*,*,#17263,.F.);
#24534=ORIENTED_EDGE('',*,*,#17264,.F.);
#24535=ORIENTED_EDGE('',*,*,#17265,.T.);
#24536=ORIENTED_EDGE('',*,*,#17261,.T.);
#24537=ORIENTED_EDGE('',*,*,#17266,.F.);
#24538=ORIENTED_EDGE('',*,*,#17267,.F.);
#24539=ORIENTED_EDGE('',*,*,#17268,.T.);
#24540=ORIENTED_EDGE('',*,*,#17264,.T.);
#24541=ORIENTED_EDGE('',*,*,#17269,.F.);
#24542=ORIENTED_EDGE('',*,*,#17270,.F.);
#24543=ORIENTED_EDGE('',*,*,#17271,.T.);
#24544=ORIENTED_EDGE('',*,*,#17267,.T.);
#24545=ORIENTED_EDGE('',*,*,#17272,.F.);
#24546=ORIENTED_EDGE('',*,*,#17273,.F.);
#24547=ORIENTED_EDGE('',*,*,#17274,.T.);
#24548=ORIENTED_EDGE('',*,*,#17270,.T.);
#24549=ORIENTED_EDGE('',*,*,#17275,.F.);
#24550=ORIENTED_EDGE('',*,*,#17276,.F.);
#24551=ORIENTED_EDGE('',*,*,#17277,.T.);
#24552=ORIENTED_EDGE('',*,*,#17273,.T.);
#24553=ORIENTED_EDGE('',*,*,#17278,.F.);
#24554=ORIENTED_EDGE('',*,*,#17279,.F.);
#24555=ORIENTED_EDGE('',*,*,#17280,.T.);
#24556=ORIENTED_EDGE('',*,*,#17276,.T.);
#24557=ORIENTED_EDGE('',*,*,#17281,.F.);
#24558=ORIENTED_EDGE('',*,*,#17282,.F.);
#24559=ORIENTED_EDGE('',*,*,#17283,.T.);
#24560=ORIENTED_EDGE('',*,*,#17279,.T.);
#24561=ORIENTED_EDGE('',*,*,#17284,.F.);
#24562=ORIENTED_EDGE('',*,*,#17285,.F.);
#24563=ORIENTED_EDGE('',*,*,#17286,.T.);
#24564=ORIENTED_EDGE('',*,*,#17282,.T.);
#24565=ORIENTED_EDGE('',*,*,#17287,.F.);
#24566=ORIENTED_EDGE('',*,*,#17288,.F.);
#24567=ORIENTED_EDGE('',*,*,#17289,.T.);
#24568=ORIENTED_EDGE('',*,*,#17290,.T.);
#24569=ORIENTED_EDGE('',*,*,#17291,.F.);
#24570=ORIENTED_EDGE('',*,*,#17292,.F.);
#24571=ORIENTED_EDGE('',*,*,#17293,.T.);
#24572=ORIENTED_EDGE('',*,*,#17294,.T.);
#24573=ORIENTED_EDGE('',*,*,#17289,.F.);
#24574=ORIENTED_EDGE('',*,*,#17295,.F.);
#24575=ORIENTED_EDGE('',*,*,#17296,.T.);
#24576=ORIENTED_EDGE('',*,*,#17297,.T.);
#24577=ORIENTED_EDGE('',*,*,#17293,.F.);
#24578=ORIENTED_EDGE('',*,*,#17298,.F.);
#24579=ORIENTED_EDGE('',*,*,#17299,.T.);
#24580=ORIENTED_EDGE('',*,*,#17300,.T.);
#24581=ORIENTED_EDGE('',*,*,#17296,.F.);
#24582=ORIENTED_EDGE('',*,*,#17301,.F.);
#24583=ORIENTED_EDGE('',*,*,#17302,.T.);
#24584=ORIENTED_EDGE('',*,*,#17303,.T.);
#24585=ORIENTED_EDGE('',*,*,#17299,.F.);
#24586=ORIENTED_EDGE('',*,*,#17304,.F.);
#24587=ORIENTED_EDGE('',*,*,#17305,.T.);
#24588=ORIENTED_EDGE('',*,*,#17306,.T.);
#24589=ORIENTED_EDGE('',*,*,#17302,.F.);
#24590=ORIENTED_EDGE('',*,*,#17307,.F.);
#24591=ORIENTED_EDGE('',*,*,#17308,.T.);
#24592=ORIENTED_EDGE('',*,*,#17309,.T.);
#24593=ORIENTED_EDGE('',*,*,#17305,.F.);
#24594=ORIENTED_EDGE('',*,*,#17310,.F.);
#24595=ORIENTED_EDGE('',*,*,#17311,.T.);
#24596=ORIENTED_EDGE('',*,*,#17312,.T.);
#24597=ORIENTED_EDGE('',*,*,#17308,.F.);
#24598=ORIENTED_EDGE('',*,*,#17313,.F.);
#24599=ORIENTED_EDGE('',*,*,#17291,.T.);
#24600=ORIENTED_EDGE('',*,*,#17314,.T.);
#24601=ORIENTED_EDGE('',*,*,#17311,.F.);
#24602=ORIENTED_EDGE('',*,*,#17315,.F.);
#24603=ORIENTED_EDGE('',*,*,#17316,.T.);
#24604=ORIENTED_EDGE('',*,*,#17317,.T.);
#24605=ORIENTED_EDGE('',*,*,#17318,.F.);
#24606=ORIENTED_EDGE('',*,*,#17319,.F.);
#24607=ORIENTED_EDGE('',*,*,#17320,.T.);
#24608=ORIENTED_EDGE('',*,*,#17321,.T.);
#24609=ORIENTED_EDGE('',*,*,#17316,.F.);
#24610=ORIENTED_EDGE('',*,*,#17322,.F.);
#24611=ORIENTED_EDGE('',*,*,#17323,.T.);
#24612=ORIENTED_EDGE('',*,*,#17324,.T.);
#24613=ORIENTED_EDGE('',*,*,#17320,.F.);
#24614=ORIENTED_EDGE('',*,*,#17325,.F.);
#24615=ORIENTED_EDGE('',*,*,#17326,.T.);
#24616=ORIENTED_EDGE('',*,*,#17327,.T.);
#24617=ORIENTED_EDGE('',*,*,#17323,.F.);
#24618=ORIENTED_EDGE('',*,*,#17328,.F.);
#24619=ORIENTED_EDGE('',*,*,#17329,.T.);
#24620=ORIENTED_EDGE('',*,*,#17330,.T.);
#24621=ORIENTED_EDGE('',*,*,#17326,.F.);
#24622=ORIENTED_EDGE('',*,*,#17331,.F.);
#24623=ORIENTED_EDGE('',*,*,#17332,.T.);
#24624=ORIENTED_EDGE('',*,*,#17333,.T.);
#24625=ORIENTED_EDGE('',*,*,#17329,.F.);
#24626=ORIENTED_EDGE('',*,*,#17334,.F.);
#24627=ORIENTED_EDGE('',*,*,#17335,.T.);
#24628=ORIENTED_EDGE('',*,*,#17336,.T.);
#24629=ORIENTED_EDGE('',*,*,#17332,.F.);
#24630=ORIENTED_EDGE('',*,*,#17337,.F.);
#24631=ORIENTED_EDGE('',*,*,#17318,.T.);
#24632=ORIENTED_EDGE('',*,*,#17338,.T.);
#24633=ORIENTED_EDGE('',*,*,#17335,.F.);
#24634=ORIENTED_EDGE('',*,*,#17339,.F.);
#24635=ORIENTED_EDGE('',*,*,#17340,.T.);
#24636=ORIENTED_EDGE('',*,*,#17341,.T.);
#24637=ORIENTED_EDGE('',*,*,#17342,.F.);
#24638=ORIENTED_EDGE('',*,*,#17343,.F.);
#24639=ORIENTED_EDGE('',*,*,#17344,.T.);
#24640=ORIENTED_EDGE('',*,*,#17345,.T.);
#24641=ORIENTED_EDGE('',*,*,#17340,.F.);
#24642=ORIENTED_EDGE('',*,*,#17346,.F.);
#24643=ORIENTED_EDGE('',*,*,#17347,.T.);
#24644=ORIENTED_EDGE('',*,*,#17348,.T.);
#24645=ORIENTED_EDGE('',*,*,#17344,.F.);
#24646=ORIENTED_EDGE('',*,*,#17349,.F.);
#24647=ORIENTED_EDGE('',*,*,#17350,.T.);
#24648=ORIENTED_EDGE('',*,*,#17351,.T.);
#24649=ORIENTED_EDGE('',*,*,#17347,.F.);
#24650=ORIENTED_EDGE('',*,*,#17352,.F.);
#24651=ORIENTED_EDGE('',*,*,#17353,.T.);
#24652=ORIENTED_EDGE('',*,*,#17354,.T.);
#24653=ORIENTED_EDGE('',*,*,#17350,.F.);
#24654=ORIENTED_EDGE('',*,*,#17355,.F.);
#24655=ORIENTED_EDGE('',*,*,#17356,.T.);
#24656=ORIENTED_EDGE('',*,*,#17357,.T.);
#24657=ORIENTED_EDGE('',*,*,#17353,.F.);
#24658=ORIENTED_EDGE('',*,*,#17358,.F.);
#24659=ORIENTED_EDGE('',*,*,#17359,.T.);
#24660=ORIENTED_EDGE('',*,*,#17360,.T.);
#24661=ORIENTED_EDGE('',*,*,#17356,.F.);
#24662=ORIENTED_EDGE('',*,*,#17361,.F.);
#24663=ORIENTED_EDGE('',*,*,#17362,.T.);
#24664=ORIENTED_EDGE('',*,*,#17363,.T.);
#24665=ORIENTED_EDGE('',*,*,#17359,.F.);
#24666=ORIENTED_EDGE('',*,*,#17364,.F.);
#24667=ORIENTED_EDGE('',*,*,#17365,.T.);
#24668=ORIENTED_EDGE('',*,*,#17366,.T.);
#24669=ORIENTED_EDGE('',*,*,#17362,.F.);
#24670=ORIENTED_EDGE('',*,*,#17367,.F.);
#24671=ORIENTED_EDGE('',*,*,#17368,.T.);
#24672=ORIENTED_EDGE('',*,*,#17369,.T.);
#24673=ORIENTED_EDGE('',*,*,#17365,.F.);
#24674=ORIENTED_EDGE('',*,*,#17370,.F.);
#24675=ORIENTED_EDGE('',*,*,#17371,.T.);
#24676=ORIENTED_EDGE('',*,*,#17372,.T.);
#24677=ORIENTED_EDGE('',*,*,#17368,.F.);
#24678=ORIENTED_EDGE('',*,*,#17373,.F.);
#24679=ORIENTED_EDGE('',*,*,#17374,.T.);
#24680=ORIENTED_EDGE('',*,*,#17375,.T.);
#24681=ORIENTED_EDGE('',*,*,#17371,.F.);
#24682=ORIENTED_EDGE('',*,*,#17376,.F.);
#24683=ORIENTED_EDGE('',*,*,#17377,.T.);
#24684=ORIENTED_EDGE('',*,*,#17378,.T.);
#24685=ORIENTED_EDGE('',*,*,#17374,.F.);
#24686=ORIENTED_EDGE('',*,*,#17379,.F.);
#24687=ORIENTED_EDGE('',*,*,#17380,.T.);
#24688=ORIENTED_EDGE('',*,*,#17381,.T.);
#24689=ORIENTED_EDGE('',*,*,#17377,.F.);
#24690=ORIENTED_EDGE('',*,*,#17382,.F.);
#24691=ORIENTED_EDGE('',*,*,#17383,.T.);
#24692=ORIENTED_EDGE('',*,*,#17384,.T.);
#24693=ORIENTED_EDGE('',*,*,#17380,.F.);
#24694=ORIENTED_EDGE('',*,*,#17385,.F.);
#24695=ORIENTED_EDGE('',*,*,#17342,.T.);
#24696=ORIENTED_EDGE('',*,*,#17386,.T.);
#24697=ORIENTED_EDGE('',*,*,#17383,.F.);
#24698=ORIENTED_EDGE('',*,*,#17386,.F.);
#24699=ORIENTED_EDGE('',*,*,#17341,.F.);
#24700=ORIENTED_EDGE('',*,*,#17345,.F.);
#24701=ORIENTED_EDGE('',*,*,#17348,.F.);
#24702=ORIENTED_EDGE('',*,*,#17351,.F.);
#24703=ORIENTED_EDGE('',*,*,#17354,.F.);
#24704=ORIENTED_EDGE('',*,*,#17357,.F.);
#24705=ORIENTED_EDGE('',*,*,#17360,.F.);
#24706=ORIENTED_EDGE('',*,*,#17363,.F.);
#24707=ORIENTED_EDGE('',*,*,#17366,.F.);
#24708=ORIENTED_EDGE('',*,*,#17369,.F.);
#24709=ORIENTED_EDGE('',*,*,#17372,.F.);
#24710=ORIENTED_EDGE('',*,*,#17375,.F.);
#24711=ORIENTED_EDGE('',*,*,#17378,.F.);
#24712=ORIENTED_EDGE('',*,*,#17381,.F.);
#24713=ORIENTED_EDGE('',*,*,#17384,.F.);
#24714=ORIENTED_EDGE('',*,*,#17338,.F.);
#24715=ORIENTED_EDGE('',*,*,#17317,.F.);
#24716=ORIENTED_EDGE('',*,*,#17321,.F.);
#24717=ORIENTED_EDGE('',*,*,#17324,.F.);
#24718=ORIENTED_EDGE('',*,*,#17327,.F.);
#24719=ORIENTED_EDGE('',*,*,#17330,.F.);
#24720=ORIENTED_EDGE('',*,*,#17333,.F.);
#24721=ORIENTED_EDGE('',*,*,#17336,.F.);
#24722=ORIENTED_EDGE('',*,*,#17314,.F.);
#24723=ORIENTED_EDGE('',*,*,#17290,.F.);
#24724=ORIENTED_EDGE('',*,*,#17294,.F.);
#24725=ORIENTED_EDGE('',*,*,#17297,.F.);
#24726=ORIENTED_EDGE('',*,*,#17300,.F.);
#24727=ORIENTED_EDGE('',*,*,#17303,.F.);
#24728=ORIENTED_EDGE('',*,*,#17306,.F.);
#24729=ORIENTED_EDGE('',*,*,#17309,.F.);
#24730=ORIENTED_EDGE('',*,*,#17312,.F.);
#24731=ORIENTED_EDGE('',*,*,#17387,.F.);
#24732=ORIENTED_EDGE('',*,*,#17388,.T.);
#24733=ORIENTED_EDGE('',*,*,#17389,.T.);
#24734=ORIENTED_EDGE('',*,*,#17390,.F.);
#24735=ORIENTED_EDGE('',*,*,#17391,.F.);
#24736=ORIENTED_EDGE('',*,*,#17392,.T.);
#24737=ORIENTED_EDGE('',*,*,#17393,.T.);
#24738=ORIENTED_EDGE('',*,*,#17388,.F.);
#24739=ORIENTED_EDGE('',*,*,#17394,.F.);
#24740=ORIENTED_EDGE('',*,*,#17395,.T.);
#24741=ORIENTED_EDGE('',*,*,#17396,.T.);
#24742=ORIENTED_EDGE('',*,*,#17392,.F.);
#24743=ORIENTED_EDGE('',*,*,#17397,.F.);
#24744=ORIENTED_EDGE('',*,*,#17390,.T.);
#24745=ORIENTED_EDGE('',*,*,#17398,.T.);
#24746=ORIENTED_EDGE('',*,*,#17395,.F.);
#24747=ORIENTED_EDGE('',*,*,#17398,.F.);
#24748=ORIENTED_EDGE('',*,*,#17389,.F.);
#24749=ORIENTED_EDGE('',*,*,#17393,.F.);
#24750=ORIENTED_EDGE('',*,*,#17396,.F.);
#24751=ORIENTED_EDGE('',*,*,#17399,.F.);
#24752=ORIENTED_EDGE('',*,*,#17400,.T.);
#24753=ORIENTED_EDGE('',*,*,#17401,.T.);
#24754=ORIENTED_EDGE('',*,*,#17402,.F.);
#24755=ORIENTED_EDGE('',*,*,#17403,.F.);
#24756=ORIENTED_EDGE('',*,*,#17404,.T.);
#24757=ORIENTED_EDGE('',*,*,#17405,.T.);
#24758=ORIENTED_EDGE('',*,*,#17400,.F.);
#24759=ORIENTED_EDGE('',*,*,#17406,.F.);
#24760=ORIENTED_EDGE('',*,*,#17407,.T.);
#24761=ORIENTED_EDGE('',*,*,#17408,.T.);
#24762=ORIENTED_EDGE('',*,*,#17404,.F.);
#24763=ORIENTED_EDGE('',*,*,#17409,.F.);
#24764=ORIENTED_EDGE('',*,*,#17410,.T.);
#24765=ORIENTED_EDGE('',*,*,#17411,.T.);
#24766=ORIENTED_EDGE('',*,*,#17407,.F.);
#24767=ORIENTED_EDGE('',*,*,#17412,.F.);
#24768=ORIENTED_EDGE('',*,*,#17413,.T.);
#24769=ORIENTED_EDGE('',*,*,#17414,.T.);
#24770=ORIENTED_EDGE('',*,*,#17410,.F.);
#24771=ORIENTED_EDGE('',*,*,#17415,.F.);
#24772=ORIENTED_EDGE('',*,*,#17416,.T.);
#24773=ORIENTED_EDGE('',*,*,#17417,.T.);
#24774=ORIENTED_EDGE('',*,*,#17413,.F.);
#24775=ORIENTED_EDGE('',*,*,#17418,.F.);
#24776=ORIENTED_EDGE('',*,*,#17419,.T.);
#24777=ORIENTED_EDGE('',*,*,#17420,.T.);
#24778=ORIENTED_EDGE('',*,*,#17416,.F.);
#24779=ORIENTED_EDGE('',*,*,#17421,.F.);
#24780=ORIENTED_EDGE('',*,*,#17422,.T.);
#24781=ORIENTED_EDGE('',*,*,#17423,.T.);
#24782=ORIENTED_EDGE('',*,*,#17419,.F.);
#24783=ORIENTED_EDGE('',*,*,#17424,.F.);
#24784=ORIENTED_EDGE('',*,*,#17402,.T.);
#24785=ORIENTED_EDGE('',*,*,#17425,.T.);
#24786=ORIENTED_EDGE('',*,*,#17422,.F.);
#24787=ORIENTED_EDGE('',*,*,#17426,.F.);
#24788=ORIENTED_EDGE('',*,*,#17427,.T.);
#24789=ORIENTED_EDGE('',*,*,#17428,.T.);
#24790=ORIENTED_EDGE('',*,*,#17429,.F.);
#24791=ORIENTED_EDGE('',*,*,#17430,.F.);
#24792=ORIENTED_EDGE('',*,*,#17431,.T.);
#24793=ORIENTED_EDGE('',*,*,#17432,.T.);
#24794=ORIENTED_EDGE('',*,*,#17427,.F.);
#24795=ORIENTED_EDGE('',*,*,#17433,.F.);
#24796=ORIENTED_EDGE('',*,*,#17434,.T.);
#24797=ORIENTED_EDGE('',*,*,#17435,.T.);
#24798=ORIENTED_EDGE('',*,*,#17431,.F.);
#24799=ORIENTED_EDGE('',*,*,#17436,.F.);
#24800=ORIENTED_EDGE('',*,*,#17437,.T.);
#24801=ORIENTED_EDGE('',*,*,#17438,.T.);
#24802=ORIENTED_EDGE('',*,*,#17434,.F.);
#24803=ORIENTED_EDGE('',*,*,#17439,.F.);
#24804=ORIENTED_EDGE('',*,*,#17440,.T.);
#24805=ORIENTED_EDGE('',*,*,#17441,.T.);
#24806=ORIENTED_EDGE('',*,*,#17437,.F.);
#24807=ORIENTED_EDGE('',*,*,#17442,.F.);
#24808=ORIENTED_EDGE('',*,*,#17443,.T.);
#24809=ORIENTED_EDGE('',*,*,#17444,.T.);
#24810=ORIENTED_EDGE('',*,*,#17440,.F.);
#24811=ORIENTED_EDGE('',*,*,#17445,.F.);
#24812=ORIENTED_EDGE('',*,*,#17446,.T.);
#24813=ORIENTED_EDGE('',*,*,#17447,.T.);
#24814=ORIENTED_EDGE('',*,*,#17443,.F.);
#24815=ORIENTED_EDGE('',*,*,#17448,.F.);
#24816=ORIENTED_EDGE('',*,*,#17429,.T.);
#24817=ORIENTED_EDGE('',*,*,#17449,.T.);
#24818=ORIENTED_EDGE('',*,*,#17446,.F.);
#24819=ORIENTED_EDGE('',*,*,#17450,.F.);
#24820=ORIENTED_EDGE('',*,*,#17451,.T.);
#24821=ORIENTED_EDGE('',*,*,#17452,.T.);
#24822=ORIENTED_EDGE('',*,*,#17453,.F.);
#24823=ORIENTED_EDGE('',*,*,#17454,.F.);
#24824=ORIENTED_EDGE('',*,*,#17455,.T.);
#24825=ORIENTED_EDGE('',*,*,#17456,.T.);
#24826=ORIENTED_EDGE('',*,*,#17451,.F.);
#24827=ORIENTED_EDGE('',*,*,#17457,.F.);
#24828=ORIENTED_EDGE('',*,*,#17458,.T.);
#24829=ORIENTED_EDGE('',*,*,#17459,.T.);
#24830=ORIENTED_EDGE('',*,*,#17455,.F.);
#24831=ORIENTED_EDGE('',*,*,#17460,.F.);
#24832=ORIENTED_EDGE('',*,*,#17461,.T.);
#24833=ORIENTED_EDGE('',*,*,#17462,.T.);
#24834=ORIENTED_EDGE('',*,*,#17458,.F.);
#24835=ORIENTED_EDGE('',*,*,#17463,.F.);
#24836=ORIENTED_EDGE('',*,*,#17464,.T.);
#24837=ORIENTED_EDGE('',*,*,#17465,.T.);
#24838=ORIENTED_EDGE('',*,*,#17461,.F.);
#24839=ORIENTED_EDGE('',*,*,#17466,.F.);
#24840=ORIENTED_EDGE('',*,*,#17467,.T.);
#24841=ORIENTED_EDGE('',*,*,#17468,.T.);
#24842=ORIENTED_EDGE('',*,*,#17464,.F.);
#24843=ORIENTED_EDGE('',*,*,#17469,.F.);
#24844=ORIENTED_EDGE('',*,*,#17470,.T.);
#24845=ORIENTED_EDGE('',*,*,#17471,.T.);
#24846=ORIENTED_EDGE('',*,*,#17467,.F.);
#24847=ORIENTED_EDGE('',*,*,#17472,.F.);
#24848=ORIENTED_EDGE('',*,*,#17473,.T.);
#24849=ORIENTED_EDGE('',*,*,#17474,.T.);
#24850=ORIENTED_EDGE('',*,*,#17470,.F.);
#24851=ORIENTED_EDGE('',*,*,#17475,.F.);
#24852=ORIENTED_EDGE('',*,*,#17476,.T.);
#24853=ORIENTED_EDGE('',*,*,#17477,.T.);
#24854=ORIENTED_EDGE('',*,*,#17473,.F.);
#24855=ORIENTED_EDGE('',*,*,#17478,.F.);
#24856=ORIENTED_EDGE('',*,*,#17479,.T.);
#24857=ORIENTED_EDGE('',*,*,#17480,.T.);
#24858=ORIENTED_EDGE('',*,*,#17476,.F.);
#24859=ORIENTED_EDGE('',*,*,#17481,.F.);
#24860=ORIENTED_EDGE('',*,*,#17482,.T.);
#24861=ORIENTED_EDGE('',*,*,#17483,.T.);
#24862=ORIENTED_EDGE('',*,*,#17479,.F.);
#24863=ORIENTED_EDGE('',*,*,#17484,.F.);
#24864=ORIENTED_EDGE('',*,*,#17485,.T.);
#24865=ORIENTED_EDGE('',*,*,#17486,.T.);
#24866=ORIENTED_EDGE('',*,*,#17482,.F.);
#24867=ORIENTED_EDGE('',*,*,#17487,.F.);
#24868=ORIENTED_EDGE('',*,*,#17488,.T.);
#24869=ORIENTED_EDGE('',*,*,#17489,.T.);
#24870=ORIENTED_EDGE('',*,*,#17485,.F.);
#24871=ORIENTED_EDGE('',*,*,#17490,.F.);
#24872=ORIENTED_EDGE('',*,*,#17491,.T.);
#24873=ORIENTED_EDGE('',*,*,#17492,.T.);
#24874=ORIENTED_EDGE('',*,*,#17488,.F.);
#24875=ORIENTED_EDGE('',*,*,#17493,.F.);
#24876=ORIENTED_EDGE('',*,*,#17494,.T.);
#24877=ORIENTED_EDGE('',*,*,#17495,.T.);
#24878=ORIENTED_EDGE('',*,*,#17491,.F.);
#24879=ORIENTED_EDGE('',*,*,#17496,.F.);
#24880=ORIENTED_EDGE('',*,*,#17453,.T.);
#24881=ORIENTED_EDGE('',*,*,#17497,.T.);
#24882=ORIENTED_EDGE('',*,*,#17494,.F.);
#24883=ORIENTED_EDGE('',*,*,#17497,.F.);
#24884=ORIENTED_EDGE('',*,*,#17452,.F.);
#24885=ORIENTED_EDGE('',*,*,#17456,.F.);
#24886=ORIENTED_EDGE('',*,*,#17459,.F.);
#24887=ORIENTED_EDGE('',*,*,#17462,.F.);
#24888=ORIENTED_EDGE('',*,*,#17465,.F.);
#24889=ORIENTED_EDGE('',*,*,#17468,.F.);
#24890=ORIENTED_EDGE('',*,*,#17471,.F.);
#24891=ORIENTED_EDGE('',*,*,#17474,.F.);
#24892=ORIENTED_EDGE('',*,*,#17477,.F.);
#24893=ORIENTED_EDGE('',*,*,#17480,.F.);
#24894=ORIENTED_EDGE('',*,*,#17483,.F.);
#24895=ORIENTED_EDGE('',*,*,#17486,.F.);
#24896=ORIENTED_EDGE('',*,*,#17489,.F.);
#24897=ORIENTED_EDGE('',*,*,#17492,.F.);
#24898=ORIENTED_EDGE('',*,*,#17495,.F.);
#24899=ORIENTED_EDGE('',*,*,#17449,.F.);
#24900=ORIENTED_EDGE('',*,*,#17428,.F.);
#24901=ORIENTED_EDGE('',*,*,#17432,.F.);
#24902=ORIENTED_EDGE('',*,*,#17435,.F.);
#24903=ORIENTED_EDGE('',*,*,#17438,.F.);
#24904=ORIENTED_EDGE('',*,*,#17441,.F.);
#24905=ORIENTED_EDGE('',*,*,#17444,.F.);
#24906=ORIENTED_EDGE('',*,*,#17447,.F.);
#24907=ORIENTED_EDGE('',*,*,#17425,.F.);
#24908=ORIENTED_EDGE('',*,*,#17401,.F.);
#24909=ORIENTED_EDGE('',*,*,#17405,.F.);
#24910=ORIENTED_EDGE('',*,*,#17408,.F.);
#24911=ORIENTED_EDGE('',*,*,#17411,.F.);
#24912=ORIENTED_EDGE('',*,*,#17414,.F.);
#24913=ORIENTED_EDGE('',*,*,#17417,.F.);
#24914=ORIENTED_EDGE('',*,*,#17420,.F.);
#24915=ORIENTED_EDGE('',*,*,#17423,.F.);
#24916=ORIENTED_EDGE('',*,*,#17426,.T.);
#24917=ORIENTED_EDGE('',*,*,#17448,.T.);
#24918=ORIENTED_EDGE('',*,*,#17445,.T.);
#24919=ORIENTED_EDGE('',*,*,#17442,.T.);
#24920=ORIENTED_EDGE('',*,*,#17439,.T.);
#24921=ORIENTED_EDGE('',*,*,#17436,.T.);
#24922=ORIENTED_EDGE('',*,*,#17433,.T.);
#24923=ORIENTED_EDGE('',*,*,#17430,.T.);
#24924=ORIENTED_EDGE('',*,*,#17399,.T.);
#24925=ORIENTED_EDGE('',*,*,#17424,.T.);
#24926=ORIENTED_EDGE('',*,*,#17421,.T.);
#24927=ORIENTED_EDGE('',*,*,#17418,.T.);
#24928=ORIENTED_EDGE('',*,*,#17415,.T.);
#24929=ORIENTED_EDGE('',*,*,#17412,.T.);
#24930=ORIENTED_EDGE('',*,*,#17409,.T.);
#24931=ORIENTED_EDGE('',*,*,#17406,.T.);
#24932=ORIENTED_EDGE('',*,*,#17403,.T.);
#24933=ORIENTED_EDGE('',*,*,#17315,.T.);
#24934=ORIENTED_EDGE('',*,*,#17337,.T.);
#24935=ORIENTED_EDGE('',*,*,#17334,.T.);
#24936=ORIENTED_EDGE('',*,*,#17331,.T.);
#24937=ORIENTED_EDGE('',*,*,#17328,.T.);
#24938=ORIENTED_EDGE('',*,*,#17325,.T.);
#24939=ORIENTED_EDGE('',*,*,#17322,.T.);
#24940=ORIENTED_EDGE('',*,*,#17319,.T.);
#24941=ORIENTED_EDGE('',*,*,#17288,.T.);
#24942=ORIENTED_EDGE('',*,*,#17313,.T.);
#24943=ORIENTED_EDGE('',*,*,#17310,.T.);
#24944=ORIENTED_EDGE('',*,*,#17307,.T.);
#24945=ORIENTED_EDGE('',*,*,#17304,.T.);
#24946=ORIENTED_EDGE('',*,*,#17301,.T.);
#24947=ORIENTED_EDGE('',*,*,#17298,.T.);
#24948=ORIENTED_EDGE('',*,*,#17295,.T.);
#24949=ORIENTED_EDGE('',*,*,#17292,.T.);
#24950=ORIENTED_EDGE('',*,*,#17112,.T.);
#24951=ORIENTED_EDGE('',*,*,#17498,.T.);
#24952=ORIENTED_EDGE('',*,*,#17499,.F.);
#24953=ORIENTED_EDGE('',*,*,#17500,.F.);
#24954=ORIENTED_EDGE('',*,*,#17501,.T.);
#24955=ORIENTED_EDGE('',*,*,#17501,.F.);
#24956=ORIENTED_EDGE('',*,*,#17502,.F.);
#24957=ORIENTED_EDGE('',*,*,#17109,.F.);
#24958=ORIENTED_EDGE('',*,*,#17105,.F.);
#24959=ORIENTED_EDGE('',*,*,#17102,.F.);
#24960=ORIENTED_EDGE('',*,*,#17099,.F.);
#24961=ORIENTED_EDGE('',*,*,#17096,.F.);
#24962=ORIENTED_EDGE('',*,*,#17093,.F.);
#24963=ORIENTED_EDGE('',*,*,#17090,.F.);
#24964=ORIENTED_EDGE('',*,*,#17087,.F.);
#24965=ORIENTED_EDGE('',*,*,#17084,.F.);
#24966=ORIENTED_EDGE('',*,*,#17081,.F.);
#24967=ORIENTED_EDGE('',*,*,#17078,.F.);
#24968=ORIENTED_EDGE('',*,*,#17075,.F.);
#24969=ORIENTED_EDGE('',*,*,#17072,.F.);
#24970=ORIENTED_EDGE('',*,*,#17069,.F.);
#24971=ORIENTED_EDGE('',*,*,#17066,.F.);
#24972=ORIENTED_EDGE('',*,*,#17063,.F.);
#24973=ORIENTED_EDGE('',*,*,#17060,.F.);
#24974=ORIENTED_EDGE('',*,*,#17057,.F.);
#24975=ORIENTED_EDGE('',*,*,#17054,.F.);
#24976=ORIENTED_EDGE('',*,*,#17051,.F.);
#24977=ORIENTED_EDGE('',*,*,#17048,.F.);
#24978=ORIENTED_EDGE('',*,*,#17045,.F.);
#24979=ORIENTED_EDGE('',*,*,#17042,.F.);
#24980=ORIENTED_EDGE('',*,*,#17039,.F.);
#24981=ORIENTED_EDGE('',*,*,#17036,.F.);
#24982=ORIENTED_EDGE('',*,*,#17033,.F.);
#24983=ORIENTED_EDGE('',*,*,#17030,.F.);
#24984=ORIENTED_EDGE('',*,*,#17027,.F.);
#24985=ORIENTED_EDGE('',*,*,#17024,.F.);
#24986=ORIENTED_EDGE('',*,*,#17021,.F.);
#24987=ORIENTED_EDGE('',*,*,#17018,.F.);
#24988=ORIENTED_EDGE('',*,*,#17015,.F.);
#24989=ORIENTED_EDGE('',*,*,#17012,.F.);
#24990=ORIENTED_EDGE('',*,*,#17009,.F.);
#24991=ORIENTED_EDGE('',*,*,#17006,.F.);
#24992=ORIENTED_EDGE('',*,*,#17003,.F.);
#24993=ORIENTED_EDGE('',*,*,#17000,.F.);
#24994=ORIENTED_EDGE('',*,*,#16997,.F.);
#24995=ORIENTED_EDGE('',*,*,#16994,.F.);
#24996=ORIENTED_EDGE('',*,*,#16991,.F.);
#24997=ORIENTED_EDGE('',*,*,#16988,.F.);
#24998=ORIENTED_EDGE('',*,*,#16985,.F.);
#24999=ORIENTED_EDGE('',*,*,#16982,.F.);
#25000=ORIENTED_EDGE('',*,*,#16979,.F.);
#25001=ORIENTED_EDGE('',*,*,#16976,.F.);
#25002=ORIENTED_EDGE('',*,*,#16973,.F.);
#25003=ORIENTED_EDGE('',*,*,#16970,.F.);
#25004=ORIENTED_EDGE('',*,*,#16967,.F.);
#25005=ORIENTED_EDGE('',*,*,#16964,.F.);
#25006=ORIENTED_EDGE('',*,*,#16961,.F.);
#25007=ORIENTED_EDGE('',*,*,#16958,.F.);
#25008=ORIENTED_EDGE('',*,*,#16955,.F.);
#25009=ORIENTED_EDGE('',*,*,#16952,.F.);
#25010=ORIENTED_EDGE('',*,*,#16949,.F.);
#25011=ORIENTED_EDGE('',*,*,#16946,.F.);
#25012=ORIENTED_EDGE('',*,*,#16943,.F.);
#25013=ORIENTED_EDGE('',*,*,#16940,.F.);
#25014=ORIENTED_EDGE('',*,*,#16937,.F.);
#25015=ORIENTED_EDGE('',*,*,#16934,.F.);
#25016=ORIENTED_EDGE('',*,*,#16931,.F.);
#25017=ORIENTED_EDGE('',*,*,#17503,.F.);
#25018=ORIENTED_EDGE('',*,*,#17504,.T.);
#25019=ORIENTED_EDGE('',*,*,#17287,.T.);
#25020=ORIENTED_EDGE('',*,*,#17284,.T.);
#25021=ORIENTED_EDGE('',*,*,#17281,.T.);
#25022=ORIENTED_EDGE('',*,*,#17278,.T.);
#25023=ORIENTED_EDGE('',*,*,#17275,.T.);
#25024=ORIENTED_EDGE('',*,*,#17272,.T.);
#25025=ORIENTED_EDGE('',*,*,#17269,.T.);
#25026=ORIENTED_EDGE('',*,*,#17266,.T.);
#25027=ORIENTED_EDGE('',*,*,#17263,.T.);
#25028=ORIENTED_EDGE('',*,*,#17260,.T.);
#25029=ORIENTED_EDGE('',*,*,#17257,.T.);
#25030=ORIENTED_EDGE('',*,*,#17254,.T.);
#25031=ORIENTED_EDGE('',*,*,#17251,.T.);
#25032=ORIENTED_EDGE('',*,*,#17248,.T.);
#25033=ORIENTED_EDGE('',*,*,#17245,.T.);
#25034=ORIENTED_EDGE('',*,*,#17242,.T.);
#25035=ORIENTED_EDGE('',*,*,#17239,.T.);
#25036=ORIENTED_EDGE('',*,*,#17236,.T.);
#25037=ORIENTED_EDGE('',*,*,#17233,.T.);
#25038=ORIENTED_EDGE('',*,*,#17230,.T.);
#25039=ORIENTED_EDGE('',*,*,#17227,.T.);
#25040=ORIENTED_EDGE('',*,*,#17224,.T.);
#25041=ORIENTED_EDGE('',*,*,#17221,.T.);
#25042=ORIENTED_EDGE('',*,*,#17218,.T.);
#25043=ORIENTED_EDGE('',*,*,#17215,.T.);
#25044=ORIENTED_EDGE('',*,*,#17212,.T.);
#25045=ORIENTED_EDGE('',*,*,#17209,.T.);
#25046=ORIENTED_EDGE('',*,*,#17206,.T.);
#25047=ORIENTED_EDGE('',*,*,#17203,.T.);
#25048=ORIENTED_EDGE('',*,*,#17200,.T.);
#25049=ORIENTED_EDGE('',*,*,#17197,.T.);
#25050=ORIENTED_EDGE('',*,*,#17194,.T.);
#25051=ORIENTED_EDGE('',*,*,#17191,.T.);
#25052=ORIENTED_EDGE('',*,*,#17188,.T.);
#25053=ORIENTED_EDGE('',*,*,#17185,.T.);
#25054=ORIENTED_EDGE('',*,*,#17182,.T.);
#25055=ORIENTED_EDGE('',*,*,#17179,.T.);
#25056=ORIENTED_EDGE('',*,*,#17176,.T.);
#25057=ORIENTED_EDGE('',*,*,#17173,.T.);
#25058=ORIENTED_EDGE('',*,*,#17170,.T.);
#25059=ORIENTED_EDGE('',*,*,#17167,.T.);
#25060=ORIENTED_EDGE('',*,*,#17164,.T.);
#25061=ORIENTED_EDGE('',*,*,#17161,.T.);
#25062=ORIENTED_EDGE('',*,*,#17158,.T.);
#25063=ORIENTED_EDGE('',*,*,#17155,.T.);
#25064=ORIENTED_EDGE('',*,*,#17152,.T.);
#25065=ORIENTED_EDGE('',*,*,#17149,.T.);
#25066=ORIENTED_EDGE('',*,*,#17146,.T.);
#25067=ORIENTED_EDGE('',*,*,#17143,.T.);
#25068=ORIENTED_EDGE('',*,*,#17140,.T.);
#25069=ORIENTED_EDGE('',*,*,#17137,.T.);
#25070=ORIENTED_EDGE('',*,*,#17134,.T.);
#25071=ORIENTED_EDGE('',*,*,#17131,.T.);
#25072=ORIENTED_EDGE('',*,*,#17128,.T.);
#25073=ORIENTED_EDGE('',*,*,#17125,.T.);
#25074=ORIENTED_EDGE('',*,*,#17122,.T.);
#25075=ORIENTED_EDGE('',*,*,#17119,.T.);
#25076=ORIENTED_EDGE('',*,*,#17116,.T.);
#25077=ORIENTED_EDGE('',*,*,#17113,.T.);
#25078=ORIENTED_EDGE('',*,*,#17505,.T.);
#25079=ORIENTED_EDGE('',*,*,#17506,.T.);
#25080=ORIENTED_EDGE('',*,*,#17507,.T.);
#25081=ORIENTED_EDGE('',*,*,#17508,.T.);
#25082=ORIENTED_EDGE('',*,*,#17503,.T.);
#25083=ORIENTED_EDGE('',*,*,#17285,.T.);
#25084=ORIENTED_EDGE('',*,*,#17504,.F.);
#25085=ORIENTED_EDGE('',*,*,#17508,.F.);
#25086=ORIENTED_EDGE('',*,*,#17509,.T.);
#25087=ORIENTED_EDGE('',*,*,#17498,.F.);
#25088=ORIENTED_EDGE('',*,*,#17111,.F.);
#25089=ORIENTED_EDGE('',*,*,#17115,.F.);
#25090=ORIENTED_EDGE('',*,*,#17118,.F.);
#25091=ORIENTED_EDGE('',*,*,#17121,.F.);
#25092=ORIENTED_EDGE('',*,*,#17124,.F.);
#25093=ORIENTED_EDGE('',*,*,#17127,.F.);
#25094=ORIENTED_EDGE('',*,*,#17130,.F.);
#25095=ORIENTED_EDGE('',*,*,#17133,.F.);
#25096=ORIENTED_EDGE('',*,*,#17136,.F.);
#25097=ORIENTED_EDGE('',*,*,#17139,.F.);
#25098=ORIENTED_EDGE('',*,*,#17142,.F.);
#25099=ORIENTED_EDGE('',*,*,#17145,.F.);
#25100=ORIENTED_EDGE('',*,*,#17148,.F.);
#25101=ORIENTED_EDGE('',*,*,#17151,.F.);
#25102=ORIENTED_EDGE('',*,*,#17154,.F.);
#25103=ORIENTED_EDGE('',*,*,#17157,.F.);
#25104=ORIENTED_EDGE('',*,*,#17160,.F.);
#25105=ORIENTED_EDGE('',*,*,#17163,.F.);
#25106=ORIENTED_EDGE('',*,*,#17166,.F.);
#25107=ORIENTED_EDGE('',*,*,#17169,.F.);
#25108=ORIENTED_EDGE('',*,*,#17172,.F.);
#25109=ORIENTED_EDGE('',*,*,#17175,.F.);
#25110=ORIENTED_EDGE('',*,*,#17178,.F.);
#25111=ORIENTED_EDGE('',*,*,#17181,.F.);
#25112=ORIENTED_EDGE('',*,*,#17184,.F.);
#25113=ORIENTED_EDGE('',*,*,#17187,.F.);
#25114=ORIENTED_EDGE('',*,*,#17190,.F.);
#25115=ORIENTED_EDGE('',*,*,#17193,.F.);
#25116=ORIENTED_EDGE('',*,*,#17196,.F.);
#25117=ORIENTED_EDGE('',*,*,#17199,.F.);
#25118=ORIENTED_EDGE('',*,*,#17202,.F.);
#25119=ORIENTED_EDGE('',*,*,#17205,.F.);
#25120=ORIENTED_EDGE('',*,*,#17208,.F.);
#25121=ORIENTED_EDGE('',*,*,#17211,.F.);
#25122=ORIENTED_EDGE('',*,*,#17214,.F.);
#25123=ORIENTED_EDGE('',*,*,#17217,.F.);
#25124=ORIENTED_EDGE('',*,*,#17220,.F.);
#25125=ORIENTED_EDGE('',*,*,#17223,.F.);
#25126=ORIENTED_EDGE('',*,*,#17226,.F.);
#25127=ORIENTED_EDGE('',*,*,#17229,.F.);
#25128=ORIENTED_EDGE('',*,*,#17232,.F.);
#25129=ORIENTED_EDGE('',*,*,#17235,.F.);
#25130=ORIENTED_EDGE('',*,*,#17238,.F.);
#25131=ORIENTED_EDGE('',*,*,#17241,.F.);
#25132=ORIENTED_EDGE('',*,*,#17244,.F.);
#25133=ORIENTED_EDGE('',*,*,#17247,.F.);
#25134=ORIENTED_EDGE('',*,*,#17250,.F.);
#25135=ORIENTED_EDGE('',*,*,#17253,.F.);
#25136=ORIENTED_EDGE('',*,*,#17256,.F.);
#25137=ORIENTED_EDGE('',*,*,#17259,.F.);
#25138=ORIENTED_EDGE('',*,*,#17262,.F.);
#25139=ORIENTED_EDGE('',*,*,#17265,.F.);
#25140=ORIENTED_EDGE('',*,*,#17268,.F.);
#25141=ORIENTED_EDGE('',*,*,#17271,.F.);
#25142=ORIENTED_EDGE('',*,*,#17274,.F.);
#25143=ORIENTED_EDGE('',*,*,#17277,.F.);
#25144=ORIENTED_EDGE('',*,*,#17280,.F.);
#25145=ORIENTED_EDGE('',*,*,#17283,.F.);
#25146=ORIENTED_EDGE('',*,*,#17286,.F.);
#25147=ORIENTED_EDGE('',*,*,#17509,.F.);
#25148=ORIENTED_EDGE('',*,*,#17507,.F.);
#25149=ORIENTED_EDGE('',*,*,#16929,.F.);
#25150=ORIENTED_EDGE('',*,*,#16933,.F.);
#25151=ORIENTED_EDGE('',*,*,#16936,.F.);
#25152=ORIENTED_EDGE('',*,*,#16939,.F.);
#25153=ORIENTED_EDGE('',*,*,#16942,.F.);
#25154=ORIENTED_EDGE('',*,*,#16945,.F.);
#25155=ORIENTED_EDGE('',*,*,#16948,.F.);
#25156=ORIENTED_EDGE('',*,*,#16951,.F.);
#25157=ORIENTED_EDGE('',*,*,#16954,.F.);
#25158=ORIENTED_EDGE('',*,*,#16957,.F.);
#25159=ORIENTED_EDGE('',*,*,#16960,.F.);
#25160=ORIENTED_EDGE('',*,*,#16963,.F.);
#25161=ORIENTED_EDGE('',*,*,#16966,.F.);
#25162=ORIENTED_EDGE('',*,*,#16969,.F.);
#25163=ORIENTED_EDGE('',*,*,#16972,.F.);
#25164=ORIENTED_EDGE('',*,*,#16975,.F.);
#25165=ORIENTED_EDGE('',*,*,#16978,.F.);
#25166=ORIENTED_EDGE('',*,*,#16981,.F.);
#25167=ORIENTED_EDGE('',*,*,#16984,.F.);
#25168=ORIENTED_EDGE('',*,*,#16987,.F.);
#25169=ORIENTED_EDGE('',*,*,#16990,.F.);
#25170=ORIENTED_EDGE('',*,*,#16993,.F.);
#25171=ORIENTED_EDGE('',*,*,#16996,.F.);
#25172=ORIENTED_EDGE('',*,*,#16999,.F.);
#25173=ORIENTED_EDGE('',*,*,#17002,.F.);
#25174=ORIENTED_EDGE('',*,*,#17005,.F.);
#25175=ORIENTED_EDGE('',*,*,#17008,.F.);
#25176=ORIENTED_EDGE('',*,*,#17011,.F.);
#25177=ORIENTED_EDGE('',*,*,#17014,.F.);
#25178=ORIENTED_EDGE('',*,*,#17017,.F.);
#25179=ORIENTED_EDGE('',*,*,#17020,.F.);
#25180=ORIENTED_EDGE('',*,*,#17023,.F.);
#25181=ORIENTED_EDGE('',*,*,#17026,.F.);
#25182=ORIENTED_EDGE('',*,*,#17029,.F.);
#25183=ORIENTED_EDGE('',*,*,#17032,.F.);
#25184=ORIENTED_EDGE('',*,*,#17035,.F.);
#25185=ORIENTED_EDGE('',*,*,#17038,.F.);
#25186=ORIENTED_EDGE('',*,*,#17041,.F.);
#25187=ORIENTED_EDGE('',*,*,#17044,.F.);
#25188=ORIENTED_EDGE('',*,*,#17047,.F.);
#25189=ORIENTED_EDGE('',*,*,#17050,.F.);
#25190=ORIENTED_EDGE('',*,*,#17053,.F.);
#25191=ORIENTED_EDGE('',*,*,#17056,.F.);
#25192=ORIENTED_EDGE('',*,*,#17059,.F.);
#25193=ORIENTED_EDGE('',*,*,#17062,.F.);
#25194=ORIENTED_EDGE('',*,*,#17065,.F.);
#25195=ORIENTED_EDGE('',*,*,#17068,.F.);
#25196=ORIENTED_EDGE('',*,*,#17071,.F.);
#25197=ORIENTED_EDGE('',*,*,#17074,.F.);
#25198=ORIENTED_EDGE('',*,*,#17077,.F.);
#25199=ORIENTED_EDGE('',*,*,#17080,.F.);
#25200=ORIENTED_EDGE('',*,*,#17083,.F.);
#25201=ORIENTED_EDGE('',*,*,#17086,.F.);
#25202=ORIENTED_EDGE('',*,*,#17089,.F.);
#25203=ORIENTED_EDGE('',*,*,#17092,.F.);
#25204=ORIENTED_EDGE('',*,*,#17095,.F.);
#25205=ORIENTED_EDGE('',*,*,#17098,.F.);
#25206=ORIENTED_EDGE('',*,*,#17101,.F.);
#25207=ORIENTED_EDGE('',*,*,#17104,.F.);
#25208=ORIENTED_EDGE('',*,*,#17108,.F.);
#25209=ORIENTED_EDGE('',*,*,#17510,.T.);
#25210=ORIENTED_EDGE('',*,*,#17511,.T.);
#25211=ORIENTED_EDGE('',*,*,#17499,.T.);
#25212=ORIENTED_EDGE('',*,*,#17107,.T.);
#25213=ORIENTED_EDGE('',*,*,#17512,.T.);
#25214=ORIENTED_EDGE('',*,*,#17500,.T.);
#25215=ORIENTED_EDGE('',*,*,#17511,.F.);
#25216=ORIENTED_EDGE('',*,*,#17513,.F.);
#25217=ORIENTED_EDGE('',*,*,#17514,.F.);
#25218=ORIENTED_EDGE('',*,*,#17515,.F.);
#25219=ORIENTED_EDGE('',*,*,#17516,.F.);
#25220=ORIENTED_EDGE('',*,*,#17517,.F.);
#25221=ORIENTED_EDGE('',*,*,#17518,.F.);
#25222=ORIENTED_EDGE('',*,*,#17510,.F.);
#25223=ORIENTED_EDGE('',*,*,#17106,.T.);
#25224=ORIENTED_EDGE('',*,*,#17502,.T.);
#25225=ORIENTED_EDGE('',*,*,#17512,.F.);
#25226=ORIENTED_EDGE('',*,*,#17519,.F.);
#25227=ORIENTED_EDGE('',*,*,#17520,.F.);
#25228=ORIENTED_EDGE('',*,*,#17521,.F.);
#25229=ORIENTED_EDGE('',*,*,#17522,.F.);
#25230=ORIENTED_EDGE('',*,*,#17523,.F.);
#25231=ORIENTED_EDGE('',*,*,#17524,.T.);
#25232=ORIENTED_EDGE('',*,*,#17525,.F.);
#25233=ORIENTED_EDGE('',*,*,#17524,.F.);
#25234=ORIENTED_EDGE('',*,*,#17526,.F.);
#25235=ORIENTED_EDGE('',*,*,#17527,.F.);
#25236=ORIENTED_EDGE('',*,*,#17522,.T.);
#25237=ORIENTED_EDGE('',*,*,#17528,.F.);
#25238=ORIENTED_EDGE('',*,*,#17517,.T.);
#25239=ORIENTED_EDGE('',*,*,#17529,.T.);
#25240=ORIENTED_EDGE('',*,*,#17521,.T.);
#25241=ORIENTED_EDGE('',*,*,#17530,.F.);
#25242=ORIENTED_EDGE('',*,*,#17518,.T.);
#25243=ORIENTED_EDGE('',*,*,#17528,.T.);
#25244=ORIENTED_EDGE('',*,*,#17520,.T.);
#25245=ORIENTED_EDGE('',*,*,#17531,.F.);
#25246=ORIENTED_EDGE('',*,*,#17513,.T.);
#25247=ORIENTED_EDGE('',*,*,#17530,.T.);
#25248=ORIENTED_EDGE('',*,*,#17519,.T.);
#25249=ORIENTED_EDGE('',*,*,#17532,.F.);
#25250=ORIENTED_EDGE('',*,*,#17514,.T.);
#25251=ORIENTED_EDGE('',*,*,#17531,.T.);
#25252=ORIENTED_EDGE('',*,*,#17527,.T.);
#25253=ORIENTED_EDGE('',*,*,#17533,.F.);
#25254=ORIENTED_EDGE('',*,*,#17515,.T.);
#25255=ORIENTED_EDGE('',*,*,#17532,.T.);
#25256=ORIENTED_EDGE('',*,*,#17526,.T.);
#25257=ORIENTED_EDGE('',*,*,#17523,.T.);
#25258=ORIENTED_EDGE('',*,*,#17529,.F.);
#25259=ORIENTED_EDGE('',*,*,#17516,.T.);
#25260=ORIENTED_EDGE('',*,*,#17533,.T.);
#25261=ORIENTED_EDGE('',*,*,#17525,.T.);
#25262=ORIENTED_EDGE('',*,*,#17450,.T.);
#25263=ORIENTED_EDGE('',*,*,#17496,.T.);
#25264=ORIENTED_EDGE('',*,*,#17493,.T.);
#25265=ORIENTED_EDGE('',*,*,#17490,.T.);
#25266=ORIENTED_EDGE('',*,*,#17487,.T.);
#25267=ORIENTED_EDGE('',*,*,#17484,.T.);
#25268=ORIENTED_EDGE('',*,*,#17481,.T.);
#25269=ORIENTED_EDGE('',*,*,#17478,.T.);
#25270=ORIENTED_EDGE('',*,*,#17475,.T.);
#25271=ORIENTED_EDGE('',*,*,#17472,.T.);
#25272=ORIENTED_EDGE('',*,*,#17469,.T.);
#25273=ORIENTED_EDGE('',*,*,#17466,.T.);
#25274=ORIENTED_EDGE('',*,*,#17463,.T.);
#25275=ORIENTED_EDGE('',*,*,#17460,.T.);
#25276=ORIENTED_EDGE('',*,*,#17457,.T.);
#25277=ORIENTED_EDGE('',*,*,#17454,.T.);
#25278=ORIENTED_EDGE('',*,*,#17387,.T.);
#25279=ORIENTED_EDGE('',*,*,#17397,.T.);
#25280=ORIENTED_EDGE('',*,*,#17394,.T.);
#25281=ORIENTED_EDGE('',*,*,#17391,.T.);
#25282=ORIENTED_EDGE('',*,*,#17339,.T.);
#25283=ORIENTED_EDGE('',*,*,#17385,.T.);
#25284=ORIENTED_EDGE('',*,*,#17382,.T.);
#25285=ORIENTED_EDGE('',*,*,#17379,.T.);
#25286=ORIENTED_EDGE('',*,*,#17376,.T.);
#25287=ORIENTED_EDGE('',*,*,#17373,.T.);
#25288=ORIENTED_EDGE('',*,*,#17370,.T.);
#25289=ORIENTED_EDGE('',*,*,#17367,.T.);
#25290=ORIENTED_EDGE('',*,*,#17364,.T.);
#25291=ORIENTED_EDGE('',*,*,#17361,.T.);
#25292=ORIENTED_EDGE('',*,*,#17358,.T.);
#25293=ORIENTED_EDGE('',*,*,#17355,.T.);
#25294=ORIENTED_EDGE('',*,*,#17352,.T.);
#25295=ORIENTED_EDGE('',*,*,#17349,.T.);
#25296=ORIENTED_EDGE('',*,*,#17346,.T.);
#25297=ORIENTED_EDGE('',*,*,#17343,.T.);
#25298=ORIENTED_EDGE('',*,*,#17534,.F.);
#25299=ORIENTED_EDGE('',*,*,#17505,.F.);
#25300=ORIENTED_EDGE('',*,*,#16930,.F.);
#25301=ORIENTED_EDGE('',*,*,#17506,.F.);
#25302=ORIENTED_EDGE('',*,*,#17535,.T.);
#25303=ORIENTED_EDGE('',*,*,#17534,.T.);
#25304=ORIENTED_EDGE('',*,*,#17535,.F.);
#25305=ORIENTED_EDGE('',*,*,#17536,.T.);
#25306=ORIENTED_EDGE('',*,*,#17537,.T.);
#25307=ORIENTED_EDGE('',*,*,#17538,.T.);
#25308=ORIENTED_EDGE('',*,*,#17537,.F.);
#25309=ORIENTED_EDGE('',*,*,#17539,.F.);
#25310=ORIENTED_EDGE('',*,*,#17540,.T.);
#25311=ORIENTED_EDGE('',*,*,#17536,.F.);
#25312=ORIENTED_EDGE('',*,*,#17540,.F.);
#25313=ORIENTED_EDGE('',*,*,#17541,.T.);
#25314=ORIENTED_EDGE('',*,*,#17538,.F.);
#25315=ORIENTED_EDGE('',*,*,#17542,.T.);
#25316=ORIENTED_EDGE('',*,*,#17543,.T.);
#25317=ORIENTED_EDGE('',*,*,#17539,.T.);
#25318=ORIENTED_EDGE('',*,*,#17543,.F.);
#25319=ORIENTED_EDGE('',*,*,#17544,.T.);
#25320=ORIENTED_EDGE('',*,*,#17542,.F.);
#25321=ORIENTED_EDGE('',*,*,#17541,.F.);
#25322=ORIENTED_EDGE('',*,*,#17545,.T.);
#25323=ORIENTED_EDGE('',*,*,#17546,.F.);
#25324=ORIENTED_EDGE('',*,*,#17547,.F.);
#25325=ORIENTED_EDGE('',*,*,#17548,.F.);
#25326=ORIENTED_EDGE('',*,*,#17549,.F.);
#25327=ORIENTED_EDGE('',*,*,#17550,.F.);
#25328=ORIENTED_EDGE('',*,*,#17551,.F.);
#25329=ORIENTED_EDGE('',*,*,#17552,.F.);
#25330=ORIENTED_EDGE('',*,*,#17545,.F.);
#25331=ORIENTED_EDGE('',*,*,#17550,.T.);
#25332=ORIENTED_EDGE('',*,*,#17553,.T.);
#25333=ORIENTED_EDGE('',*,*,#17554,.T.);
#25334=ORIENTED_EDGE('',*,*,#17555,.F.);
#25335=ORIENTED_EDGE('',*,*,#17549,.T.);
#25336=ORIENTED_EDGE('',*,*,#17556,.T.);
#25337=ORIENTED_EDGE('',*,*,#17557,.T.);
#25338=ORIENTED_EDGE('',*,*,#17553,.F.);
#25339=ORIENTED_EDGE('',*,*,#17548,.T.);
#25340=ORIENTED_EDGE('',*,*,#17558,.T.);
#25341=ORIENTED_EDGE('',*,*,#17559,.T.);
#25342=ORIENTED_EDGE('',*,*,#17556,.F.);
#25343=ORIENTED_EDGE('',*,*,#17554,.F.);
#25344=ORIENTED_EDGE('',*,*,#17557,.F.);
#25345=ORIENTED_EDGE('',*,*,#17559,.F.);
#25346=ORIENTED_EDGE('',*,*,#17560,.F.);
#25347=ORIENTED_EDGE('',*,*,#17561,.F.);
#25348=ORIENTED_EDGE('',*,*,#17562,.T.);
#25349=ORIENTED_EDGE('',*,*,#17544,.F.);
#25350=ORIENTED_EDGE('',*,*,#17562,.F.);
#25351=ORIENTED_EDGE('',*,*,#17563,.F.);
#25352=ORIENTED_EDGE('',*,*,#17564,.F.);
#25353=ORIENTED_EDGE('',*,*,#17547,.T.);
#25354=ORIENTED_EDGE('',*,*,#17565,.T.);
#25355=ORIENTED_EDGE('',*,*,#17560,.T.);
#25356=ORIENTED_EDGE('',*,*,#17558,.F.);
#25357=ORIENTED_EDGE('',*,*,#17551,.T.);
#25358=ORIENTED_EDGE('',*,*,#17555,.T.);
#25359=ORIENTED_EDGE('',*,*,#17564,.T.);
#25360=ORIENTED_EDGE('',*,*,#17566,.F.);
#25361=ORIENTED_EDGE('',*,*,#17546,.T.);
#25362=ORIENTED_EDGE('',*,*,#17552,.T.);
#25363=ORIENTED_EDGE('',*,*,#17566,.T.);
#25364=ORIENTED_EDGE('',*,*,#17563,.T.);
#25365=ORIENTED_EDGE('',*,*,#17561,.T.);
#25366=ORIENTED_EDGE('',*,*,#17565,.F.);
#25367=ORIENTED_EDGE('',*,*,#17567,.T.);
#25368=ORIENTED_EDGE('',*,*,#17568,.T.);
#25369=ORIENTED_EDGE('',*,*,#17569,.F.);
#25370=ORIENTED_EDGE('',*,*,#17568,.F.);
#25371=ORIENTED_EDGE('',*,*,#17570,.F.);
#25372=ORIENTED_EDGE('',*,*,#17569,.T.);
#25373=ORIENTED_EDGE('',*,*,#17571,.F.);
#25374=ORIENTED_EDGE('',*,*,#17572,.T.);
#25375=ORIENTED_EDGE('',*,*,#17570,.T.);
#25376=ORIENTED_EDGE('',*,*,#17572,.F.);
#25377=ORIENTED_EDGE('',*,*,#17573,.F.);
#25378=ORIENTED_EDGE('',*,*,#17574,.T.);
#25379=ORIENTED_EDGE('',*,*,#17571,.T.);
#25380=ORIENTED_EDGE('',*,*,#17574,.F.);
#25381=ORIENTED_EDGE('',*,*,#17573,.T.);
#25382=ORIENTED_EDGE('',*,*,#17575,.F.);
#25383=ORIENTED_EDGE('',*,*,#17575,.T.);
#25384=ORIENTED_EDGE('',*,*,#17576,.T.);
#25385=ORIENTED_EDGE('',*,*,#17567,.F.);
#25386=ORIENTED_EDGE('',*,*,#17576,.F.);
#25387=ORIENTED_EDGE('',*,*,#17577,.T.);
#25388=ORIENTED_EDGE('',*,*,#17578,.T.);
#25389=ORIENTED_EDGE('',*,*,#17579,.T.);
#25390=ORIENTED_EDGE('',*,*,#17580,.T.);
#25391=ORIENTED_EDGE('',*,*,#17578,.F.);
#25392=ORIENTED_EDGE('',*,*,#17579,.F.);
#25393=ORIENTED_EDGE('',*,*,#17580,.F.);
#25394=ORIENTED_EDGE('',*,*,#17581,.T.);
#25395=ORIENTED_EDGE('',*,*,#17582,.F.);
#25396=ORIENTED_EDGE('',*,*,#17583,.F.);
#25397=ORIENTED_EDGE('',*,*,#17581,.F.);
#25398=ORIENTED_EDGE('',*,*,#17577,.F.);
#25399=ORIENTED_EDGE('',*,*,#17582,.T.);
#25400=ORIENTED_EDGE('',*,*,#17583,.T.);
#25401=ORIENTED_EDGE('',*,*,#17584,.T.);
#25402=ORIENTED_EDGE('',*,*,#17585,.T.);
#25403=ORIENTED_EDGE('',*,*,#17586,.T.);
#25404=ORIENTED_EDGE('',*,*,#17584,.F.);
#25405=ORIENTED_EDGE('',*,*,#17585,.F.);
#25406=ORIENTED_EDGE('',*,*,#17586,.F.);
#25407=ORIENTED_EDGE('',*,*,#17587,.T.);
#25408=ORIENTED_EDGE('',*,*,#17588,.T.);
#25409=ORIENTED_EDGE('',*,*,#17587,.F.);
#25410=ORIENTED_EDGE('',*,*,#17589,.T.);
#25411=ORIENTED_EDGE('',*,*,#17590,.T.);
#25412=ORIENTED_EDGE('',*,*,#17591,.T.);
#25413=ORIENTED_EDGE('',*,*,#17590,.F.);
#25414=ORIENTED_EDGE('',*,*,#17592,.F.);
#25415=ORIENTED_EDGE('',*,*,#17593,.T.);
#25416=ORIENTED_EDGE('',*,*,#17591,.F.);
#25417=ORIENTED_EDGE('',*,*,#17593,.F.);
#25418=ORIENTED_EDGE('',*,*,#17594,.T.);
#25419=ORIENTED_EDGE('',*,*,#17595,.F.);
#25420=ORIENTED_EDGE('',*,*,#17596,.F.);
#25421=ORIENTED_EDGE('',*,*,#17597,.F.);
#25422=ORIENTED_EDGE('',*,*,#17589,.F.);
#25423=ORIENTED_EDGE('',*,*,#17598,.T.);
#25424=ORIENTED_EDGE('',*,*,#17599,.T.);
#25425=ORIENTED_EDGE('',*,*,#17592,.T.);
#25426=ORIENTED_EDGE('',*,*,#17599,.F.);
#25427=ORIENTED_EDGE('',*,*,#17600,.T.);
#25428=ORIENTED_EDGE('',*,*,#17601,.F.);
#25429=ORIENTED_EDGE('',*,*,#17602,.F.);
#25430=ORIENTED_EDGE('',*,*,#17603,.F.);
#25431=ORIENTED_EDGE('',*,*,#17598,.F.);
#25432=ORIENTED_EDGE('',*,*,#17604,.T.);
#25433=ORIENTED_EDGE('',*,*,#17605,.T.);
#25434=ORIENTED_EDGE('',*,*,#17606,.T.);
#25435=ORIENTED_EDGE('',*,*,#17607,.T.);
#25436=ORIENTED_EDGE('',*,*,#17606,.F.);
#25437=ORIENTED_EDGE('',*,*,#17608,.T.);
#25438=ORIENTED_EDGE('',*,*,#17609,.T.);
#25439=ORIENTED_EDGE('',*,*,#17604,.F.);
#25440=ORIENTED_EDGE('',*,*,#17605,.F.);
#25441=ORIENTED_EDGE('',*,*,#17609,.F.);
#25442=ORIENTED_EDGE('',*,*,#17607,.F.);
#25443=ORIENTED_EDGE('',*,*,#17610,.T.);
#25444=ORIENTED_EDGE('',*,*,#17588,.F.);
#25445=ORIENTED_EDGE('',*,*,#17611,.T.);
#25446=ORIENTED_EDGE('',*,*,#17612,.T.);
#25447=ORIENTED_EDGE('',*,*,#17613,.T.);
#25448=ORIENTED_EDGE('',*,*,#17611,.F.);
#25449=ORIENTED_EDGE('',*,*,#17613,.F.);
#25450=ORIENTED_EDGE('',*,*,#17614,.F.);
#25451=ORIENTED_EDGE('',*,*,#17612,.F.);
#25452=ORIENTED_EDGE('',*,*,#17614,.T.);
#25453=ORIENTED_EDGE('',*,*,#17615,.T.);
#25454=ORIENTED_EDGE('',*,*,#17616,.T.);
#25455=ORIENTED_EDGE('',*,*,#17615,.F.);
#25456=ORIENTED_EDGE('',*,*,#17616,.F.);
#25457=ORIENTED_EDGE('',*,*,#17617,.T.);
#25458=ORIENTED_EDGE('',*,*,#17618,.T.);
#25459=ORIENTED_EDGE('',*,*,#17619,.T.);
#25460=ORIENTED_EDGE('',*,*,#17617,.F.);
#25461=ORIENTED_EDGE('',*,*,#17619,.F.);
#25462=ORIENTED_EDGE('',*,*,#17620,.F.);
#25463=ORIENTED_EDGE('',*,*,#17618,.F.);
#25464=ORIENTED_EDGE('',*,*,#17620,.T.);
#25465=ORIENTED_EDGE('',*,*,#17621,.T.);
#25466=ORIENTED_EDGE('',*,*,#17622,.T.);
#25467=ORIENTED_EDGE('',*,*,#17621,.F.);
#25468=ORIENTED_EDGE('',*,*,#17622,.F.);
#25469=ORIENTED_EDGE('',*,*,#17623,.T.);
#25470=ORIENTED_EDGE('',*,*,#17624,.T.);
#25471=ORIENTED_EDGE('',*,*,#17625,.T.);
#25472=ORIENTED_EDGE('',*,*,#17623,.F.);
#25473=ORIENTED_EDGE('',*,*,#17625,.F.);
#25474=ORIENTED_EDGE('',*,*,#17608,.F.);
#25475=ORIENTED_EDGE('',*,*,#17624,.F.);
#25476=ORIENTED_EDGE('',*,*,#17626,.F.);
#25477=ORIENTED_EDGE('',*,*,#17627,.F.);
#25478=ORIENTED_EDGE('',*,*,#17600,.F.);
#25479=ORIENTED_EDGE('',*,*,#17628,.F.);
#25480=ORIENTED_EDGE('',*,*,#17629,.F.);
#25481=ORIENTED_EDGE('',*,*,#17630,.F.);
#25482=ORIENTED_EDGE('',*,*,#17594,.F.);
#25483=ORIENTED_EDGE('',*,*,#17631,.F.);
#25484=ORIENTED_EDGE('',*,*,#17632,.F.);
#25485=ORIENTED_EDGE('',*,*,#17633,.F.);
#25486=ORIENTED_EDGE('',*,*,#17634,.T.);
#25487=ORIENTED_EDGE('',*,*,#17626,.T.);
#25488=ORIENTED_EDGE('',*,*,#17634,.F.);
#25489=ORIENTED_EDGE('',*,*,#17635,.F.);
#25490=ORIENTED_EDGE('',*,*,#17636,.T.);
#25491=ORIENTED_EDGE('',*,*,#17633,.T.);
#25492=ORIENTED_EDGE('',*,*,#17636,.F.);
#25493=ORIENTED_EDGE('',*,*,#17637,.F.);
#25494=ORIENTED_EDGE('',*,*,#17638,.T.);
#25495=ORIENTED_EDGE('',*,*,#17635,.T.);
#25496=ORIENTED_EDGE('',*,*,#17638,.F.);
#25497=ORIENTED_EDGE('',*,*,#17637,.T.);
#25498=ORIENTED_EDGE('',*,*,#17639,.F.);
#25499=ORIENTED_EDGE('',*,*,#17610,.F.);
#25500=ORIENTED_EDGE('',*,*,#17640,.T.);
#25501=ORIENTED_EDGE('',*,*,#17639,.T.);
#25502=ORIENTED_EDGE('',*,*,#17640,.F.);
#25503=ORIENTED_EDGE('',*,*,#17630,.T.);
#25504=ORIENTED_EDGE('',*,*,#17641,.T.);
#25505=ORIENTED_EDGE('',*,*,#17642,.T.);
#25506=ORIENTED_EDGE('',*,*,#17595,.T.);
#25507=ORIENTED_EDGE('',*,*,#17629,.T.);
#25508=ORIENTED_EDGE('',*,*,#17643,.F.);
#25509=ORIENTED_EDGE('',*,*,#17644,.T.);
#25510=ORIENTED_EDGE('',*,*,#17641,.F.);
#25511=ORIENTED_EDGE('',*,*,#17628,.T.);
#25512=ORIENTED_EDGE('',*,*,#17603,.T.);
#25513=ORIENTED_EDGE('',*,*,#17645,.F.);
#25514=ORIENTED_EDGE('',*,*,#17643,.T.);
#25515=ORIENTED_EDGE('',*,*,#17646,.T.);
#25516=ORIENTED_EDGE('',*,*,#17596,.T.);
#25517=ORIENTED_EDGE('',*,*,#17642,.F.);
#25518=ORIENTED_EDGE('',*,*,#17647,.T.);
#25519=ORIENTED_EDGE('',*,*,#17631,.T.);
#25520=ORIENTED_EDGE('',*,*,#17597,.T.);
#25521=ORIENTED_EDGE('',*,*,#17646,.F.);
#25522=ORIENTED_EDGE('',*,*,#17648,.T.);
#25523=ORIENTED_EDGE('',*,*,#17647,.F.);
#25524=ORIENTED_EDGE('',*,*,#17644,.F.);
#25525=ORIENTED_EDGE('',*,*,#17649,.F.);
#25526=ORIENTED_EDGE('',*,*,#17650,.T.);
#25527=ORIENTED_EDGE('',*,*,#17627,.T.);
#25528=ORIENTED_EDGE('',*,*,#17651,.T.);
#25529=ORIENTED_EDGE('',*,*,#17652,.T.);
#25530=ORIENTED_EDGE('',*,*,#17601,.T.);
#25531=ORIENTED_EDGE('',*,*,#17652,.F.);
#25532=ORIENTED_EDGE('',*,*,#17649,.T.);
#25533=ORIENTED_EDGE('',*,*,#17645,.T.);
#25534=ORIENTED_EDGE('',*,*,#17602,.T.);
#25535=ORIENTED_EDGE('',*,*,#17632,.T.);
#25536=ORIENTED_EDGE('',*,*,#17648,.F.);
#25537=ORIENTED_EDGE('',*,*,#17650,.F.);
#25538=ORIENTED_EDGE('',*,*,#17651,.F.);
#25539=ORIENTED_EDGE('',*,*,#17653,.T.);
#25540=ORIENTED_EDGE('',*,*,#17654,.T.);
#25541=ORIENTED_EDGE('',*,*,#17655,.T.);
#25542=ORIENTED_EDGE('',*,*,#17654,.F.);
#25543=ORIENTED_EDGE('',*,*,#17656,.F.);
#25544=ORIENTED_EDGE('',*,*,#17657,.F.);
#25545=ORIENTED_EDGE('',*,*,#17658,.F.);
#25546=ORIENTED_EDGE('',*,*,#17659,.F.);
#25547=ORIENTED_EDGE('',*,*,#17660,.F.);
#25548=ORIENTED_EDGE('',*,*,#17661,.F.);
#25549=ORIENTED_EDGE('',*,*,#17662,.F.);
#25550=ORIENTED_EDGE('',*,*,#17663,.F.);
#25551=ORIENTED_EDGE('',*,*,#17664,.F.);
#25552=ORIENTED_EDGE('',*,*,#17665,.F.);
#25553=ORIENTED_EDGE('',*,*,#17666,.F.);
#25554=ORIENTED_EDGE('',*,*,#17667,.F.);
#25555=ORIENTED_EDGE('',*,*,#17668,.F.);
#25556=ORIENTED_EDGE('',*,*,#17669,.F.);
#25557=ORIENTED_EDGE('',*,*,#17653,.F.);
#25558=ORIENTED_EDGE('',*,*,#17655,.F.);
#25559=ORIENTED_EDGE('',*,*,#17670,.T.);
#25560=ORIENTED_EDGE('',*,*,#17671,.F.);
#25561=ORIENTED_EDGE('',*,*,#17670,.F.);
#25562=ORIENTED_EDGE('',*,*,#17660,.T.);
#25563=ORIENTED_EDGE('',*,*,#17672,.T.);
#25564=ORIENTED_EDGE('',*,*,#17673,.T.);
#25565=ORIENTED_EDGE('',*,*,#17672,.F.);
#25566=ORIENTED_EDGE('',*,*,#17673,.F.);
#25567=ORIENTED_EDGE('',*,*,#17674,.T.);
#25568=ORIENTED_EDGE('',*,*,#17675,.F.);
#25569=ORIENTED_EDGE('',*,*,#17674,.F.);
#25570=ORIENTED_EDGE('',*,*,#17669,.T.);
#25571=ORIENTED_EDGE('',*,*,#17676,.T.);
#25572=ORIENTED_EDGE('',*,*,#17677,.T.);
#25573=ORIENTED_EDGE('',*,*,#17676,.F.);
#25574=ORIENTED_EDGE('',*,*,#17677,.F.);
#25575=ORIENTED_EDGE('',*,*,#17678,.T.);
#25576=ORIENTED_EDGE('',*,*,#17679,.F.);
#25577=ORIENTED_EDGE('',*,*,#17678,.F.);
#25578=ORIENTED_EDGE('',*,*,#17661,.T.);
#25579=ORIENTED_EDGE('',*,*,#17680,.T.);
#25580=ORIENTED_EDGE('',*,*,#17681,.T.);
#25581=ORIENTED_EDGE('',*,*,#17680,.F.);
#25582=ORIENTED_EDGE('',*,*,#17681,.F.);
#25583=ORIENTED_EDGE('',*,*,#17682,.T.);
#25584=ORIENTED_EDGE('',*,*,#17683,.F.);
#25585=ORIENTED_EDGE('',*,*,#17682,.F.);
#25586=ORIENTED_EDGE('',*,*,#17668,.T.);
#25587=ORIENTED_EDGE('',*,*,#17684,.T.);
#25588=ORIENTED_EDGE('',*,*,#17685,.T.);
#25589=ORIENTED_EDGE('',*,*,#17684,.F.);
#25590=ORIENTED_EDGE('',*,*,#17685,.F.);
#25591=ORIENTED_EDGE('',*,*,#17686,.T.);
#25592=ORIENTED_EDGE('',*,*,#17687,.F.);
#25593=ORIENTED_EDGE('',*,*,#17686,.F.);
#25594=ORIENTED_EDGE('',*,*,#17662,.T.);
#25595=ORIENTED_EDGE('',*,*,#17688,.T.);
#25596=ORIENTED_EDGE('',*,*,#17689,.T.);
#25597=ORIENTED_EDGE('',*,*,#17688,.F.);
#25598=ORIENTED_EDGE('',*,*,#17689,.F.);
#25599=ORIENTED_EDGE('',*,*,#17690,.T.);
#25600=ORIENTED_EDGE('',*,*,#17691,.F.);
#25601=ORIENTED_EDGE('',*,*,#17690,.F.);
#25602=ORIENTED_EDGE('',*,*,#17667,.T.);
#25603=ORIENTED_EDGE('',*,*,#17692,.T.);
#25604=ORIENTED_EDGE('',*,*,#17693,.T.);
#25605=ORIENTED_EDGE('',*,*,#17692,.F.);
#25606=ORIENTED_EDGE('',*,*,#17693,.F.);
#25607=ORIENTED_EDGE('',*,*,#17694,.T.);
#25608=ORIENTED_EDGE('',*,*,#17695,.F.);
#25609=ORIENTED_EDGE('',*,*,#17694,.F.);
#25610=ORIENTED_EDGE('',*,*,#17696,.T.);
#25611=ORIENTED_EDGE('',*,*,#17697,.T.);
#25612=ORIENTED_EDGE('',*,*,#17698,.T.);
#25613=ORIENTED_EDGE('',*,*,#17697,.F.);
#25614=ORIENTED_EDGE('',*,*,#17699,.F.);
#25615=ORIENTED_EDGE('',*,*,#17700,.F.);
#25616=ORIENTED_EDGE('',*,*,#17701,.F.);
#25617=ORIENTED_EDGE('',*,*,#17702,.F.);
#25618=ORIENTED_EDGE('',*,*,#17703,.F.);
#25619=ORIENTED_EDGE('',*,*,#17704,.F.);
#25620=ORIENTED_EDGE('',*,*,#17705,.F.);
#25621=ORIENTED_EDGE('',*,*,#17706,.F.);
#25622=ORIENTED_EDGE('',*,*,#17707,.F.);
#25623=ORIENTED_EDGE('',*,*,#17708,.F.);
#25624=ORIENTED_EDGE('',*,*,#17709,.F.);
#25625=ORIENTED_EDGE('',*,*,#17710,.F.);
#25626=ORIENTED_EDGE('',*,*,#17711,.F.);
#25627=ORIENTED_EDGE('',*,*,#17712,.F.);
#25628=ORIENTED_EDGE('',*,*,#17696,.F.);
#25629=ORIENTED_EDGE('',*,*,#17713,.F.);
#25630=ORIENTED_EDGE('',*,*,#17714,.T.);
#25631=ORIENTED_EDGE('',*,*,#17698,.F.);
#25632=ORIENTED_EDGE('',*,*,#17714,.F.);
#25633=ORIENTED_EDGE('',*,*,#17703,.T.);
#25634=ORIENTED_EDGE('',*,*,#17715,.T.);
#25635=ORIENTED_EDGE('',*,*,#17716,.T.);
#25636=ORIENTED_EDGE('',*,*,#17715,.F.);
#25637=ORIENTED_EDGE('',*,*,#17717,.F.);
#25638=ORIENTED_EDGE('',*,*,#17718,.T.);
#25639=ORIENTED_EDGE('',*,*,#17716,.F.);
#25640=ORIENTED_EDGE('',*,*,#17718,.F.);
#25641=ORIENTED_EDGE('',*,*,#17712,.T.);
#25642=ORIENTED_EDGE('',*,*,#17719,.T.);
#25643=ORIENTED_EDGE('',*,*,#17720,.T.);
#25644=ORIENTED_EDGE('',*,*,#17719,.F.);
#25645=ORIENTED_EDGE('',*,*,#17721,.F.);
#25646=ORIENTED_EDGE('',*,*,#17722,.T.);
#25647=ORIENTED_EDGE('',*,*,#17720,.F.);
#25648=ORIENTED_EDGE('',*,*,#17722,.F.);
#25649=ORIENTED_EDGE('',*,*,#17704,.T.);
#25650=ORIENTED_EDGE('',*,*,#17723,.T.);
#25651=ORIENTED_EDGE('',*,*,#17724,.T.);
#25652=ORIENTED_EDGE('',*,*,#17723,.F.);
#25653=ORIENTED_EDGE('',*,*,#17725,.F.);
#25654=ORIENTED_EDGE('',*,*,#17726,.T.);
#25655=ORIENTED_EDGE('',*,*,#17724,.F.);
#25656=ORIENTED_EDGE('',*,*,#17726,.F.);
#25657=ORIENTED_EDGE('',*,*,#17711,.T.);
#25658=ORIENTED_EDGE('',*,*,#17727,.T.);
#25659=ORIENTED_EDGE('',*,*,#17728,.T.);
#25660=ORIENTED_EDGE('',*,*,#17727,.F.);
#25661=ORIENTED_EDGE('',*,*,#17729,.F.);
#25662=ORIENTED_EDGE('',*,*,#17730,.T.);
#25663=ORIENTED_EDGE('',*,*,#17728,.F.);
#25664=ORIENTED_EDGE('',*,*,#17730,.F.);
#25665=ORIENTED_EDGE('',*,*,#17731,.T.);
#25666=ORIENTED_EDGE('',*,*,#17699,.T.);
#25667=ORIENTED_EDGE('',*,*,#17732,.T.);
#25668=ORIENTED_EDGE('',*,*,#17733,.T.);
#25669=ORIENTED_EDGE('',*,*,#17734,.T.);
#25670=ORIENTED_EDGE('',*,*,#17735,.T.);
#25671=ORIENTED_EDGE('',*,*,#17731,.F.);
#25672=ORIENTED_EDGE('',*,*,#17736,.T.);
#25673=ORIENTED_EDGE('',*,*,#17737,.T.);
#25674=ORIENTED_EDGE('',*,*,#17738,.T.);
#25675=ORIENTED_EDGE('',*,*,#17734,.F.);
#25676=ORIENTED_EDGE('',*,*,#17739,.T.);
#25677=ORIENTED_EDGE('',*,*,#17740,.T.);
#25678=ORIENTED_EDGE('',*,*,#17741,.T.);
#25679=ORIENTED_EDGE('',*,*,#17737,.F.);
#25680=ORIENTED_EDGE('',*,*,#17742,.T.);
#25681=ORIENTED_EDGE('',*,*,#17743,.T.);
#25682=ORIENTED_EDGE('',*,*,#17656,.T.);
#25683=ORIENTED_EDGE('',*,*,#17740,.F.);
#25684=ORIENTED_EDGE('',*,*,#17744,.T.);
#25685=ORIENTED_EDGE('',*,*,#17745,.T.);
#25686=ORIENTED_EDGE('',*,*,#17746,.T.);
#25687=ORIENTED_EDGE('',*,*,#17743,.F.);
#25688=ORIENTED_EDGE('',*,*,#17747,.T.);
#25689=ORIENTED_EDGE('',*,*,#17748,.T.);
#25690=ORIENTED_EDGE('',*,*,#17749,.T.);
#25691=ORIENTED_EDGE('',*,*,#17745,.F.);
#25692=ORIENTED_EDGE('',*,*,#17750,.T.);
#25693=ORIENTED_EDGE('',*,*,#17732,.F.);
#25694=ORIENTED_EDGE('',*,*,#17751,.T.);
#25695=ORIENTED_EDGE('',*,*,#17748,.F.);
#25696=ORIENTED_EDGE('',*,*,#17752,.T.);
#25697=ORIENTED_EDGE('',*,*,#17746,.F.);
#25698=ORIENTED_EDGE('',*,*,#17753,.T.);
#25699=ORIENTED_EDGE('',*,*,#17754,.F.);
#25700=ORIENTED_EDGE('',*,*,#17657,.T.);
#25701=ORIENTED_EDGE('',*,*,#17749,.F.);
#25702=ORIENTED_EDGE('',*,*,#17755,.F.);
#25703=ORIENTED_EDGE('',*,*,#17756,.F.);
#25704=ORIENTED_EDGE('',*,*,#17753,.F.);
#25705=ORIENTED_EDGE('',*,*,#17751,.F.);
#25706=ORIENTED_EDGE('',*,*,#17702,.T.);
#25707=ORIENTED_EDGE('',*,*,#17757,.F.);
#25708=ORIENTED_EDGE('',*,*,#17755,.T.);
#25709=ORIENTED_EDGE('',*,*,#17758,.F.);
#25710=ORIENTED_EDGE('',*,*,#17759,.F.);
#25711=ORIENTED_EDGE('',*,*,#17760,.F.);
#25712=ORIENTED_EDGE('',*,*,#17761,.F.);
#25713=ORIENTED_EDGE('',*,*,#17762,.F.);
#25714=ORIENTED_EDGE('',*,*,#17763,.F.);
#25715=ORIENTED_EDGE('',*,*,#17764,.F.);
#25716=ORIENTED_EDGE('',*,*,#17765,.F.);
#25717=ORIENTED_EDGE('',*,*,#17733,.F.);
#25718=ORIENTED_EDGE('',*,*,#17752,.F.);
#25719=ORIENTED_EDGE('',*,*,#17750,.F.);
#25720=ORIENTED_EDGE('',*,*,#17747,.F.);
#25721=ORIENTED_EDGE('',*,*,#17744,.F.);
#25722=ORIENTED_EDGE('',*,*,#17742,.F.);
#25723=ORIENTED_EDGE('',*,*,#17739,.F.);
#25724=ORIENTED_EDGE('',*,*,#17736,.F.);
#25725=ORIENTED_EDGE('',*,*,#17710,.T.);
#25726=ORIENTED_EDGE('',*,*,#17766,.T.);
#25727=ORIENTED_EDGE('',*,*,#17767,.T.);
#25728=ORIENTED_EDGE('',*,*,#17766,.F.);
#25729=ORIENTED_EDGE('',*,*,#17768,.F.);
#25730=ORIENTED_EDGE('',*,*,#17769,.T.);
#25731=ORIENTED_EDGE('',*,*,#17767,.F.);
#25732=ORIENTED_EDGE('',*,*,#17769,.F.);
#25733=ORIENTED_EDGE('',*,*,#17705,.T.);
#25734=ORIENTED_EDGE('',*,*,#17770,.T.);
#25735=ORIENTED_EDGE('',*,*,#17771,.T.);
#25736=ORIENTED_EDGE('',*,*,#17770,.F.);
#25737=ORIENTED_EDGE('',*,*,#17772,.F.);
#25738=ORIENTED_EDGE('',*,*,#17773,.T.);
#25739=ORIENTED_EDGE('',*,*,#17771,.F.);
#25740=ORIENTED_EDGE('',*,*,#17773,.F.);
#25741=ORIENTED_EDGE('',*,*,#17709,.T.);
#25742=ORIENTED_EDGE('',*,*,#17774,.T.);
#25743=ORIENTED_EDGE('',*,*,#17775,.T.);
#25744=ORIENTED_EDGE('',*,*,#17774,.F.);
#25745=ORIENTED_EDGE('',*,*,#17776,.F.);
#25746=ORIENTED_EDGE('',*,*,#17777,.T.);
#25747=ORIENTED_EDGE('',*,*,#17775,.F.);
#25748=ORIENTED_EDGE('',*,*,#17777,.F.);
#25749=ORIENTED_EDGE('',*,*,#17663,.T.);
#25750=ORIENTED_EDGE('',*,*,#17778,.T.);
#25751=ORIENTED_EDGE('',*,*,#17779,.T.);
#25752=ORIENTED_EDGE('',*,*,#17778,.F.);
#25753=ORIENTED_EDGE('',*,*,#17779,.F.);
#25754=ORIENTED_EDGE('',*,*,#17780,.T.);
#25755=ORIENTED_EDGE('',*,*,#17781,.F.);
#25756=ORIENTED_EDGE('',*,*,#17780,.F.);
#25757=ORIENTED_EDGE('',*,*,#17706,.T.);
#25758=ORIENTED_EDGE('',*,*,#17782,.T.);
#25759=ORIENTED_EDGE('',*,*,#17783,.T.);
#25760=ORIENTED_EDGE('',*,*,#17782,.F.);
#25761=ORIENTED_EDGE('',*,*,#17784,.F.);
#25762=ORIENTED_EDGE('',*,*,#17785,.T.);
#25763=ORIENTED_EDGE('',*,*,#17783,.F.);
#25764=ORIENTED_EDGE('',*,*,#17785,.F.);
#25765=ORIENTED_EDGE('',*,*,#17666,.T.);
#25766=ORIENTED_EDGE('',*,*,#17786,.T.);
#25767=ORIENTED_EDGE('',*,*,#17787,.T.);
#25768=ORIENTED_EDGE('',*,*,#17786,.F.);
#25769=ORIENTED_EDGE('',*,*,#17787,.F.);
#25770=ORIENTED_EDGE('',*,*,#17788,.T.);
#25771=ORIENTED_EDGE('',*,*,#17789,.F.);
#25772=ORIENTED_EDGE('',*,*,#17788,.F.);
#25773=ORIENTED_EDGE('',*,*,#17708,.T.);
#25774=ORIENTED_EDGE('',*,*,#17790,.T.);
#25775=ORIENTED_EDGE('',*,*,#17791,.T.);
#25776=ORIENTED_EDGE('',*,*,#17790,.F.);
#25777=ORIENTED_EDGE('',*,*,#17792,.F.);
#25778=ORIENTED_EDGE('',*,*,#17793,.T.);
#25779=ORIENTED_EDGE('',*,*,#17791,.F.);
#25780=ORIENTED_EDGE('',*,*,#17793,.F.);
#25781=ORIENTED_EDGE('',*,*,#17664,.T.);
#25782=ORIENTED_EDGE('',*,*,#17794,.T.);
#25783=ORIENTED_EDGE('',*,*,#17795,.T.);
#25784=ORIENTED_EDGE('',*,*,#17794,.F.);
#25785=ORIENTED_EDGE('',*,*,#17795,.F.);
#25786=ORIENTED_EDGE('',*,*,#17796,.T.);
#25787=ORIENTED_EDGE('',*,*,#17797,.F.);
#25788=ORIENTED_EDGE('',*,*,#17796,.F.);
#25789=ORIENTED_EDGE('',*,*,#17707,.T.);
#25790=ORIENTED_EDGE('',*,*,#17798,.T.);
#25791=ORIENTED_EDGE('',*,*,#17799,.T.);
#25792=ORIENTED_EDGE('',*,*,#17798,.F.);
#25793=ORIENTED_EDGE('',*,*,#17800,.F.);
#25794=ORIENTED_EDGE('',*,*,#17801,.T.);
#25795=ORIENTED_EDGE('',*,*,#17799,.F.);
#25796=ORIENTED_EDGE('',*,*,#17801,.F.);
#25797=ORIENTED_EDGE('',*,*,#17802,.T.);
#25798=ORIENTED_EDGE('',*,*,#17803,.T.);
#25799=ORIENTED_EDGE('',*,*,#17713,.T.);
#25800=ORIENTED_EDGE('',*,*,#17803,.F.);
#25801=ORIENTED_EDGE('',*,*,#17804,.F.);
#25802=ORIENTED_EDGE('',*,*,#17805,.F.);
#25803=ORIENTED_EDGE('',*,*,#17806,.F.);
#25804=ORIENTED_EDGE('',*,*,#17807,.F.);
#25805=ORIENTED_EDGE('',*,*,#17808,.F.);
#25806=ORIENTED_EDGE('',*,*,#17809,.F.);
#25807=ORIENTED_EDGE('',*,*,#17810,.F.);
#25808=ORIENTED_EDGE('',*,*,#17811,.F.);
#25809=ORIENTED_EDGE('',*,*,#17812,.F.);
#25810=ORIENTED_EDGE('',*,*,#17813,.F.);
#25811=ORIENTED_EDGE('',*,*,#17814,.F.);
#25812=ORIENTED_EDGE('',*,*,#17815,.F.);
#25813=ORIENTED_EDGE('',*,*,#17816,.F.);
#25814=ORIENTED_EDGE('',*,*,#17817,.F.);
#25815=ORIENTED_EDGE('',*,*,#17802,.F.);
#25816=ORIENTED_EDGE('',*,*,#17808,.T.);
#25817=ORIENTED_EDGE('',*,*,#17818,.T.);
#25818=ORIENTED_EDGE('',*,*,#17717,.T.);
#25819=ORIENTED_EDGE('',*,*,#17818,.F.);
#25820=ORIENTED_EDGE('',*,*,#17817,.T.);
#25821=ORIENTED_EDGE('',*,*,#17819,.T.);
#25822=ORIENTED_EDGE('',*,*,#17721,.T.);
#25823=ORIENTED_EDGE('',*,*,#17819,.F.);
#25824=ORIENTED_EDGE('',*,*,#17809,.T.);
#25825=ORIENTED_EDGE('',*,*,#17820,.T.);
#25826=ORIENTED_EDGE('',*,*,#17725,.T.);
#25827=ORIENTED_EDGE('',*,*,#17820,.F.);
#25828=ORIENTED_EDGE('',*,*,#17816,.T.);
#25829=ORIENTED_EDGE('',*,*,#17821,.T.);
#25830=ORIENTED_EDGE('',*,*,#17729,.T.);
#25831=ORIENTED_EDGE('',*,*,#17821,.F.);
#25832=ORIENTED_EDGE('',*,*,#17665,.T.);
#25833=ORIENTED_EDGE('',*,*,#17822,.T.);
#25834=ORIENTED_EDGE('',*,*,#17823,.T.);
#25835=ORIENTED_EDGE('',*,*,#17822,.F.);
#25836=ORIENTED_EDGE('',*,*,#17823,.F.);
#25837=ORIENTED_EDGE('',*,*,#17824,.T.);
#25838=ORIENTED_EDGE('',*,*,#17825,.F.);
#25839=ORIENTED_EDGE('',*,*,#17824,.F.);
#25840=ORIENTED_EDGE('',*,*,#17826,.T.);
#25841=ORIENTED_EDGE('',*,*,#17827,.T.);
#25842=ORIENTED_EDGE('',*,*,#17671,.T.);
#25843=ORIENTED_EDGE('',*,*,#17827,.F.);
#25844=ORIENTED_EDGE('',*,*,#17828,.F.);
#25845=ORIENTED_EDGE('',*,*,#17829,.F.);
#25846=ORIENTED_EDGE('',*,*,#17830,.F.);
#25847=ORIENTED_EDGE('',*,*,#17831,.F.);
#25848=ORIENTED_EDGE('',*,*,#17832,.F.);
#25849=ORIENTED_EDGE('',*,*,#17833,.F.);
#25850=ORIENTED_EDGE('',*,*,#17834,.F.);
#25851=ORIENTED_EDGE('',*,*,#17835,.F.);
#25852=ORIENTED_EDGE('',*,*,#17836,.F.);
#25853=ORIENTED_EDGE('',*,*,#17837,.F.);
#25854=ORIENTED_EDGE('',*,*,#17838,.F.);
#25855=ORIENTED_EDGE('',*,*,#17839,.F.);
#25856=ORIENTED_EDGE('',*,*,#17840,.F.);
#25857=ORIENTED_EDGE('',*,*,#17841,.F.);
#25858=ORIENTED_EDGE('',*,*,#17826,.F.);
#25859=ORIENTED_EDGE('',*,*,#17832,.T.);
#25860=ORIENTED_EDGE('',*,*,#17842,.T.);
#25861=ORIENTED_EDGE('',*,*,#17675,.T.);
#25862=ORIENTED_EDGE('',*,*,#17842,.F.);
#25863=ORIENTED_EDGE('',*,*,#17841,.T.);
#25864=ORIENTED_EDGE('',*,*,#17843,.T.);
#25865=ORIENTED_EDGE('',*,*,#17679,.T.);
#25866=ORIENTED_EDGE('',*,*,#17843,.F.);
#25867=ORIENTED_EDGE('',*,*,#17833,.T.);
#25868=ORIENTED_EDGE('',*,*,#17844,.T.);
#25869=ORIENTED_EDGE('',*,*,#17683,.T.);
#25870=ORIENTED_EDGE('',*,*,#17844,.F.);
#25871=ORIENTED_EDGE('',*,*,#17840,.T.);
#25872=ORIENTED_EDGE('',*,*,#17845,.T.);
#25873=ORIENTED_EDGE('',*,*,#17687,.T.);
#25874=ORIENTED_EDGE('',*,*,#17845,.F.);
#25875=ORIENTED_EDGE('',*,*,#17846,.T.);
#25876=ORIENTED_EDGE('',*,*,#17828,.T.);
#25877=ORIENTED_EDGE('',*,*,#17847,.T.);
#25878=ORIENTED_EDGE('',*,*,#17758,.T.);
#25879=ORIENTED_EDGE('',*,*,#17848,.T.);
#25880=ORIENTED_EDGE('',*,*,#17849,.T.);
#25881=ORIENTED_EDGE('',*,*,#17846,.F.);
#25882=ORIENTED_EDGE('',*,*,#17765,.T.);
#25883=ORIENTED_EDGE('',*,*,#17850,.T.);
#25884=ORIENTED_EDGE('',*,*,#17851,.T.);
#25885=ORIENTED_EDGE('',*,*,#17848,.F.);
#25886=ORIENTED_EDGE('',*,*,#17764,.T.);
#25887=ORIENTED_EDGE('',*,*,#17852,.T.);
#25888=ORIENTED_EDGE('',*,*,#17853,.T.);
#25889=ORIENTED_EDGE('',*,*,#17850,.F.);
#25890=ORIENTED_EDGE('',*,*,#17763,.T.);
#25891=ORIENTED_EDGE('',*,*,#17854,.T.);
#25892=ORIENTED_EDGE('',*,*,#17804,.T.);
#25893=ORIENTED_EDGE('',*,*,#17852,.F.);
#25894=ORIENTED_EDGE('',*,*,#17762,.T.);
#25895=ORIENTED_EDGE('',*,*,#17855,.T.);
#25896=ORIENTED_EDGE('',*,*,#17856,.T.);
#25897=ORIENTED_EDGE('',*,*,#17854,.F.);
#25898=ORIENTED_EDGE('',*,*,#17761,.T.);
#25899=ORIENTED_EDGE('',*,*,#17857,.T.);
#25900=ORIENTED_EDGE('',*,*,#17858,.T.);
#25901=ORIENTED_EDGE('',*,*,#17855,.F.);
#25902=ORIENTED_EDGE('',*,*,#17760,.T.);
#25903=ORIENTED_EDGE('',*,*,#17847,.F.);
#25904=ORIENTED_EDGE('',*,*,#17859,.T.);
#25905=ORIENTED_EDGE('',*,*,#17857,.F.);
#25906=ORIENTED_EDGE('',*,*,#17759,.T.);
#25907=ORIENTED_EDGE('',*,*,#17856,.F.);
#25908=ORIENTED_EDGE('',*,*,#17860,.T.);
#25909=ORIENTED_EDGE('',*,*,#17861,.F.);
#25910=ORIENTED_EDGE('',*,*,#17805,.T.);
#25911=ORIENTED_EDGE('',*,*,#17858,.F.);
#25912=ORIENTED_EDGE('',*,*,#17862,.F.);
#25913=ORIENTED_EDGE('',*,*,#17863,.F.);
#25914=ORIENTED_EDGE('',*,*,#17860,.F.);
#25915=ORIENTED_EDGE('',*,*,#17859,.F.);
#25916=ORIENTED_EDGE('',*,*,#17831,.T.);
#25917=ORIENTED_EDGE('',*,*,#17864,.F.);
#25918=ORIENTED_EDGE('',*,*,#17862,.T.);
#25919=ORIENTED_EDGE('',*,*,#17839,.T.);
#25920=ORIENTED_EDGE('',*,*,#17865,.T.);
#25921=ORIENTED_EDGE('',*,*,#17825,.T.);
#25922=ORIENTED_EDGE('',*,*,#17865,.F.);
#25923=ORIENTED_EDGE('',*,*,#17810,.T.);
#25924=ORIENTED_EDGE('',*,*,#17866,.T.);
#25925=ORIENTED_EDGE('',*,*,#17800,.T.);
#25926=ORIENTED_EDGE('',*,*,#17866,.F.);
#25927=ORIENTED_EDGE('',*,*,#17834,.T.);
#25928=ORIENTED_EDGE('',*,*,#17867,.T.);
#25929=ORIENTED_EDGE('',*,*,#17797,.T.);
#25930=ORIENTED_EDGE('',*,*,#17867,.F.);
#25931=ORIENTED_EDGE('',*,*,#17815,.T.);
#25932=ORIENTED_EDGE('',*,*,#17868,.T.);
#25933=ORIENTED_EDGE('',*,*,#17792,.T.);
#25934=ORIENTED_EDGE('',*,*,#17868,.F.);
#25935=ORIENTED_EDGE('',*,*,#17838,.T.);
#25936=ORIENTED_EDGE('',*,*,#17869,.T.);
#25937=ORIENTED_EDGE('',*,*,#17789,.T.);
#25938=ORIENTED_EDGE('',*,*,#17869,.F.);
#25939=ORIENTED_EDGE('',*,*,#17811,.T.);
#25940=ORIENTED_EDGE('',*,*,#17870,.T.);
#25941=ORIENTED_EDGE('',*,*,#17784,.T.);
#25942=ORIENTED_EDGE('',*,*,#17870,.F.);
#25943=ORIENTED_EDGE('',*,*,#17835,.T.);
#25944=ORIENTED_EDGE('',*,*,#17871,.T.);
#25945=ORIENTED_EDGE('',*,*,#17781,.T.);
#25946=ORIENTED_EDGE('',*,*,#17871,.F.);
#25947=ORIENTED_EDGE('',*,*,#17814,.T.);
#25948=ORIENTED_EDGE('',*,*,#17872,.T.);
#25949=ORIENTED_EDGE('',*,*,#17776,.T.);
#25950=ORIENTED_EDGE('',*,*,#17872,.F.);
#25951=ORIENTED_EDGE('',*,*,#17837,.T.);
#25952=ORIENTED_EDGE('',*,*,#17873,.T.);
#25953=ORIENTED_EDGE('',*,*,#17691,.T.);
#25954=ORIENTED_EDGE('',*,*,#17873,.F.);
#25955=ORIENTED_EDGE('',*,*,#17812,.T.);
#25956=ORIENTED_EDGE('',*,*,#17874,.T.);
#25957=ORIENTED_EDGE('',*,*,#17768,.T.);
#25958=ORIENTED_EDGE('',*,*,#17874,.F.);
#25959=ORIENTED_EDGE('',*,*,#17836,.T.);
#25960=ORIENTED_EDGE('',*,*,#17875,.T.);
#25961=ORIENTED_EDGE('',*,*,#17695,.T.);
#25962=ORIENTED_EDGE('',*,*,#17875,.F.);
#25963=ORIENTED_EDGE('',*,*,#17813,.T.);
#25964=ORIENTED_EDGE('',*,*,#17876,.T.);
#25965=ORIENTED_EDGE('',*,*,#17772,.T.);
#25966=ORIENTED_EDGE('',*,*,#17876,.F.);
#25967=ORIENTED_EDGE('',*,*,#17877,.T.);
#25968=ORIENTED_EDGE('',*,*,#17878,.T.);
#25969=ORIENTED_EDGE('',*,*,#17879,.T.);
#25970=ORIENTED_EDGE('',*,*,#17880,.T.);
#25971=ORIENTED_EDGE('',*,*,#17877,.F.);
#25972=ORIENTED_EDGE('',*,*,#17881,.T.);
#25973=ORIENTED_EDGE('',*,*,#17882,.T.);
#25974=ORIENTED_EDGE('',*,*,#17883,.T.);
#25975=ORIENTED_EDGE('',*,*,#17884,.T.);
#25976=ORIENTED_EDGE('',*,*,#17885,.T.);
#25977=ORIENTED_EDGE('',*,*,#17882,.F.);
#25978=ORIENTED_EDGE('',*,*,#17886,.T.);
#25979=ORIENTED_EDGE('',*,*,#17884,.F.);
#25980=ORIENTED_EDGE('',*,*,#17887,.T.);
#25981=ORIENTED_EDGE('',*,*,#17888,.T.);
#25982=ORIENTED_EDGE('',*,*,#17830,.T.);
#25983=ORIENTED_EDGE('',*,*,#17889,.T.);
#25984=ORIENTED_EDGE('',*,*,#17864,.T.);
#25985=ORIENTED_EDGE('',*,*,#17888,.F.);
#25986=ORIENTED_EDGE('',*,*,#17890,.T.);
#25987=ORIENTED_EDGE('',*,*,#17889,.F.);
#25988=ORIENTED_EDGE('',*,*,#17891,.T.);
#25989=ORIENTED_EDGE('',*,*,#17892,.T.);
#25990=ORIENTED_EDGE('',*,*,#17863,.T.);
#25991=ORIENTED_EDGE('',*,*,#17893,.T.);
#25992=ORIENTED_EDGE('',*,*,#17861,.T.);
#25993=ORIENTED_EDGE('',*,*,#17892,.F.);
#25994=ORIENTED_EDGE('',*,*,#17894,.T.);
#25995=ORIENTED_EDGE('',*,*,#17893,.F.);
#25996=ORIENTED_EDGE('',*,*,#17895,.T.);
#25997=ORIENTED_EDGE('',*,*,#17879,.F.);
#25998=ORIENTED_EDGE('',*,*,#17806,.T.);
#25999=ORIENTED_EDGE('',*,*,#17853,.F.);
#26000=ORIENTED_EDGE('',*,*,#17807,.T.);
#26001=ORIENTED_EDGE('',*,*,#17878,.F.);
#26002=ORIENTED_EDGE('',*,*,#17896,.T.);
#26003=ORIENTED_EDGE('',*,*,#17880,.F.);
#26004=ORIENTED_EDGE('',*,*,#17895,.F.);
#26005=ORIENTED_EDGE('',*,*,#17894,.F.);
#26006=ORIENTED_EDGE('',*,*,#17891,.F.);
#26007=ORIENTED_EDGE('',*,*,#17890,.F.);
#26008=ORIENTED_EDGE('',*,*,#17887,.F.);
#26009=ORIENTED_EDGE('',*,*,#17886,.F.);
#26010=ORIENTED_EDGE('',*,*,#17881,.F.);
#26011=ORIENTED_EDGE('',*,*,#17897,.F.);
#26012=ORIENTED_EDGE('',*,*,#17898,.F.);
#26013=ORIENTED_EDGE('',*,*,#17899,.F.);
#26014=ORIENTED_EDGE('',*,*,#17900,.F.);
#26015=ORIENTED_EDGE('',*,*,#17901,.F.);
#26016=ORIENTED_EDGE('',*,*,#17902,.F.);
#26017=ORIENTED_EDGE('',*,*,#17903,.F.);
#26018=ORIENTED_EDGE('',*,*,#17904,.F.);
#26019=ORIENTED_EDGE('',*,*,#17905,.T.);
#26020=ORIENTED_EDGE('',*,*,#17906,.T.);
#26021=ORIENTED_EDGE('',*,*,#17907,.T.);
#26022=ORIENTED_EDGE('',*,*,#17897,.T.);
#26023=ORIENTED_EDGE('',*,*,#17905,.F.);
#26024=ORIENTED_EDGE('',*,*,#17904,.T.);
#26025=ORIENTED_EDGE('',*,*,#17908,.T.);
#26026=ORIENTED_EDGE('',*,*,#17909,.T.);
#26027=ORIENTED_EDGE('',*,*,#17910,.T.);
#26028=ORIENTED_EDGE('',*,*,#17911,.T.);
#26029=ORIENTED_EDGE('',*,*,#17908,.F.);
#26030=ORIENTED_EDGE('',*,*,#17903,.T.);
#26031=ORIENTED_EDGE('',*,*,#17910,.F.);
#26032=ORIENTED_EDGE('',*,*,#17902,.T.);
#26033=ORIENTED_EDGE('',*,*,#17912,.T.);
#26034=ORIENTED_EDGE('',*,*,#17701,.T.);
#26035=ORIENTED_EDGE('',*,*,#17913,.T.);
#26036=ORIENTED_EDGE('',*,*,#17757,.T.);
#26037=ORIENTED_EDGE('',*,*,#17912,.F.);
#26038=ORIENTED_EDGE('',*,*,#17901,.T.);
#26039=ORIENTED_EDGE('',*,*,#17913,.F.);
#26040=ORIENTED_EDGE('',*,*,#17900,.T.);
#26041=ORIENTED_EDGE('',*,*,#17914,.T.);
#26042=ORIENTED_EDGE('',*,*,#17756,.T.);
#26043=ORIENTED_EDGE('',*,*,#17915,.T.);
#26044=ORIENTED_EDGE('',*,*,#17754,.T.);
#26045=ORIENTED_EDGE('',*,*,#17914,.F.);
#26046=ORIENTED_EDGE('',*,*,#17899,.T.);
#26047=ORIENTED_EDGE('',*,*,#17915,.F.);
#26048=ORIENTED_EDGE('',*,*,#17898,.T.);
#26049=ORIENTED_EDGE('',*,*,#17907,.F.);
#26050=ORIENTED_EDGE('',*,*,#17658,.T.);
#26051=ORIENTED_EDGE('',*,*,#17741,.F.);
#26052=ORIENTED_EDGE('',*,*,#17659,.T.);
#26053=ORIENTED_EDGE('',*,*,#17906,.F.);
#26054=ORIENTED_EDGE('',*,*,#17916,.T.);
#26055=ORIENTED_EDGE('',*,*,#17735,.F.);
#26056=ORIENTED_EDGE('',*,*,#17917,.T.);
#26057=ORIENTED_EDGE('',*,*,#17911,.F.);
#26058=ORIENTED_EDGE('',*,*,#17700,.T.);
#26059=ORIENTED_EDGE('',*,*,#17738,.F.);
#26060=ORIENTED_EDGE('',*,*,#17916,.F.);
#26061=ORIENTED_EDGE('',*,*,#17909,.F.);
#26062=ORIENTED_EDGE('',*,*,#17917,.F.);
#26063=ORIENTED_EDGE('',*,*,#17851,.F.);
#26064=ORIENTED_EDGE('',*,*,#17896,.F.);
#26065=ORIENTED_EDGE('',*,*,#17883,.F.);
#26066=ORIENTED_EDGE('',*,*,#17918,.F.);
#26067=ORIENTED_EDGE('',*,*,#17849,.F.);
#26068=ORIENTED_EDGE('',*,*,#17918,.T.);
#26069=ORIENTED_EDGE('',*,*,#17885,.F.);
#26070=ORIENTED_EDGE('',*,*,#17829,.T.);
#26071=PLANE('',#28690);
#26072=PLANE('',#28691);
#26073=PLANE('',#28692);
#26074=PLANE('',#28693);
#26075=PLANE('',#28694);
#26076=PLANE('',#28695);
#26077=PLANE('',#28696);
#26078=PLANE('',#28697);
#26079=PLANE('',#28698);
#26080=PLANE('',#28699);
#26081=PLANE('',#28700);
#26082=PLANE('',#28701);
#26083=PLANE('',#28702);
#26084=PLANE('',#28703);
#26085=PLANE('',#28707);
#26086=PLANE('',#28727);
#26087=PLANE('',#28737);
#26088=PLANE('',#28767);
#26089=PLANE('',#28777);
#26090=PLANE('',#28780);
#26091=PLANE('',#28784);
#26092=PLANE('',#28788);
#26093=PLANE('',#28791);
#26094=PLANE('',#28794);
#26095=PLANE('',#28801);
#26096=PLANE('',#28804);
#26097=PLANE('',#28808);
#26098=PLANE('',#28811);
#26099=PLANE('',#28812);
#26100=PLANE('',#28813);
#26101=PLANE('',#28817);
#26102=PLANE('',#28834);
#26103=PLANE('',#28837);
#26104=PLANE('',#28840);
#26105=PLANE('',#28843);
#26106=PLANE('',#28848);
#26107=PLANE('',#28851);
#26108=PLANE('',#28857);
#26109=PLANE('',#28860);
#26110=PLANE('',#28863);
#26111=PLANE('',#28865);
#26112=PLANE('',#28868);
#26113=PLANE('',#28882);
#26114=PLANE('',#28886);
#26115=PLANE('',#28890);
#26116=PLANE('',#28894);
#26117=PLANE('',#28897);
#26118=PLANE('',#28900);
#26119=PLANE('',#28907);
#26120=PLANE('',#28910);
#26121=PLANE('',#28914);
#26122=PLANE('',#28918);
#26123=PLANE('',#28919);
#26124=PLANE('',#28921);
#26125=PLANE('',#28926);
#26126=PLANE('',#28937);
#26127=PLANE('',#28940);
#26128=PLANE('',#28943);
#26129=PLANE('',#28946);
#26130=PLANE('',#28951);
#26131=PLANE('',#28954);
#26132=PLANE('',#28959);
#26133=PLANE('',#28961);
#26134=PLANE('',#28963);
#26135=PLANE('',#28966);
#26136=PLANE('',#28970);
#26137=PLANE('',#28999);
#26138=PLANE('',#29003);
#26139=PLANE('',#29010);
#26140=PLANE('',#29011);
#26141=PLANE('',#29012);
#26142=PLANE('',#29013);
#26143=PLANE('',#29014);
#26144=PLANE('',#29015);
#26145=PLANE('',#29016);
#26146=PLANE('',#29017);
#26147=PLANE('',#29018);
#26148=PLANE('',#29019);
#26149=PLANE('',#29020);
#26150=PLANE('',#29021);
#26151=PLANE('',#29022);
#26152=PLANE('',#29023);
#26153=PLANE('',#29024);
#26154=PLANE('',#29025);
#26155=PLANE('',#29026);
#26156=PLANE('',#29027);
#26157=PLANE('',#29028);
#26158=PLANE('',#29029);
#26159=PLANE('',#29030);
#26160=PLANE('',#29031);
#26161=PLANE('',#29032);
#26162=PLANE('',#29033);
#26163=PLANE('',#29034);
#26164=PLANE('',#29035);
#26165=PLANE('',#29036);
#26166=PLANE('',#29037);
#26167=PLANE('',#29038);
#26168=PLANE('',#29039);
#26169=PLANE('',#29040);
#26170=PLANE('',#29041);
#26171=PLANE('',#29043);
#26172=PLANE('',#29046);
#26173=PLANE('',#29047);
#26174=PLANE('',#29048);
#26175=PLANE('',#29049);
#26176=PLANE('',#29050);
#26177=PLANE('',#29051);
#26178=PLANE('',#29052);
#26179=PLANE('',#29053);
#26180=PLANE('',#29054);
#26181=PLANE('',#29055);
#26182=PLANE('',#29056);
#26183=PLANE('',#29057);
#26184=PLANE('',#29058);
#26185=PLANE('',#29059);
#26186=PLANE('',#29060);
#26187=PLANE('',#29061);
#26188=PLANE('',#29062);
#26189=PLANE('',#29063);
#26190=PLANE('',#29064);
#26191=PLANE('',#29065);
#26192=PLANE('',#29066);
#26193=PLANE('',#29067);
#26194=PLANE('',#29068);
#26195=PLANE('',#29069);
#26196=PLANE('',#29070);
#26197=PLANE('',#29071);
#26198=PLANE('',#29072);
#26199=PLANE('',#29073);
#26200=PLANE('',#29074);
#26201=PLANE('',#29075);
#26202=PLANE('',#29076);
#26203=PLANE('',#29077);
#26204=PLANE('',#29078);
#26205=PLANE('',#29079);
#26206=PLANE('',#29080);
#26207=PLANE('',#29081);
#26208=PLANE('',#29082);
#26209=PLANE('',#29083);
#26210=PLANE('',#29084);
#26211=PLANE('',#29085);
#26212=PLANE('',#29086);
#26213=PLANE('',#29087);
#26214=PLANE('',#29088);
#26215=PLANE('',#29089);
#26216=PLANE('',#29090);
#26217=PLANE('',#29091);
#26218=PLANE('',#29092);
#26219=PLANE('',#29093);
#26220=PLANE('',#29094);
#26221=PLANE('',#29095);
#26222=PLANE('',#29096);
#26223=PLANE('',#29097);
#26224=PLANE('',#29098);
#26225=PLANE('',#29099);
#26226=PLANE('',#29100);
#26227=PLANE('',#29101);
#26228=PLANE('',#29102);
#26229=PLANE('',#29103);
#26230=PLANE('',#29104);
#26231=PLANE('',#29105);
#26232=PLANE('',#29106);
#26233=PLANE('',#29107);
#26234=PLANE('',#29108);
#26235=PLANE('',#29109);
#26236=PLANE('',#29110);
#26237=PLANE('',#29111);
#26238=PLANE('',#29112);
#26239=PLANE('',#29113);
#26240=PLANE('',#29114);
#26241=PLANE('',#29115);
#26242=PLANE('',#29116);
#26243=PLANE('',#29119);
#26244=PLANE('',#29120);
#26245=PLANE('',#29121);
#26246=PLANE('',#29122);
#26247=PLANE('',#29123);
#26248=PLANE('',#29124);
#26249=PLANE('',#29125);
#26250=PLANE('',#29126);
#26251=PLANE('',#29127);
#26252=PLANE('',#29128);
#26253=PLANE('',#29129);
#26254=PLANE('',#29130);
#26255=PLANE('',#29131);
#26256=PLANE('',#29132);
#26257=PLANE('',#29133);
#26258=PLANE('',#29134);
#26259=PLANE('',#29135);
#26260=PLANE('',#29136);
#26261=PLANE('',#29137);
#26262=PLANE('',#29138);
#26263=PLANE('',#29139);
#26264=PLANE('',#29140);
#26265=PLANE('',#29141);
#26266=PLANE('',#29142);
#26267=PLANE('',#29143);
#26268=PLANE('',#29144);
#26269=PLANE('',#29145);
#26270=PLANE('',#29146);
#26271=PLANE('',#29159);
#26272=PLANE('',#29166);
#26273=PLANE('',#29175);
#26274=PLANE('',#29176);
#26275=PLANE('',#29177);
#26276=PLANE('',#29178);
#26277=PLANE('',#29179);
#26278=PLANE('',#29180);
#26279=PLANE('',#29182);
#26280=PLANE('',#29183);
#26281=PLANE('',#29184);
#26282=PLANE('',#29185);
#26283=PLANE('',#29186);
#26284=PLANE('',#29187);
#26285=PLANE('',#29188);
#26286=PLANE('',#29189);
#26287=PLANE('',#29190);
#26288=PLANE('',#29191);
#26289=PLANE('',#29192);
#26290=PLANE('',#29193);
#26291=PLANE('',#29194);
#26292=PLANE('',#29195);
#26293=PLANE('',#29196);
#26294=PLANE('',#29197);
#26295=PLANE('',#29198);
#26296=PLANE('',#29199);
#26297=PLANE('',#29200);
#26298=PLANE('',#29201);
#26299=PLANE('',#29202);
#26300=PLANE('',#29203);
#26301=PLANE('',#29204);
#26302=PLANE('',#29205);
#26303=PLANE('',#29206);
#26304=PLANE('',#29207);
#26305=PLANE('',#29208);
#26306=PLANE('',#29209);
#26307=PLANE('',#29210);
#26308=PLANE('',#29211);
#26309=PLANE('',#29212);
#26310=PLANE('',#29213);
#26311=PLANE('',#29214);
#26312=PLANE('',#29215);
#26313=PLANE('',#29216);
#26314=PLANE('',#29217);
#26315=PLANE('',#29218);
#26316=PLANE('',#29219);
#26317=PLANE('',#29220);
#26318=PLANE('',#29221);
#26319=PLANE('',#29222);
#26320=PLANE('',#29223);
#26321=PLANE('',#29224);
#26322=PLANE('',#29225);
#26323=PLANE('',#29226);
#26324=PLANE('',#29227);
#26325=PLANE('',#29228);
#26326=PLANE('',#29229);
#26327=PLANE('',#29230);
#26328=PLANE('',#29231);
#26329=PLANE('',#29234);
#26330=PLANE('',#29235);
#26331=PLANE('',#29236);
#26332=PLANE('',#29237);
#26333=PLANE('',#29238);
#26334=PLANE('',#29241);
#26335=PLANE('',#29242);
#26336=PLANE('',#29243);
#26337=PLANE('',#29244);
#26338=PLANE('',#29245);
#26339=PLANE('',#29246);
#26340=PLANE('',#29247);
#26341=PLANE('',#29248);
#26342=PLANE('',#29249);
#26343=PLANE('',#29250);
#26344=PLANE('',#29251);
#26345=PLANE('',#29252);
#26346=PLANE('',#29253);
#26347=PLANE('',#29254);
#26348=PLANE('',#29255);
#26349=PLANE('',#29256);
#26350=PLANE('',#29257);
#26351=PLANE('',#29258);
#26352=PLANE('',#29259);
#26353=PLANE('',#29260);
#26354=PLANE('',#29263);
#26355=PLANE('',#29264);
#26356=PLANE('',#29265);
#26357=PLANE('',#29266);
#26358=PLANE('',#29267);
#26359=PLANE('',#29270);
#26360=PLANE('',#29273);
#26361=PLANE('',#29278);
#26362=PLANE('',#29279);
#26363=PLANE('',#29282);
#26364=PLANE('',#29285);
#26365=PLANE('',#29288);
#26366=PLANE('',#29293);
#26367=PLANE('',#29294);
#26368=PLANE('',#29297);
#26369=PLANE('',#29300);
#26370=PLANE('',#29301);
#26371=PLANE('',#29302);
#26372=PLANE('',#29303);
#26373=PLANE('',#29304);
#26374=PLANE('',#29305);
#26375=PLANE('',#29307);
#26376=PLANE('',#29308);
#26377=PLANE('',#29309);
#26378=PLANE('',#29310);
#26379=PLANE('',#29311);
#26380=PLANE('',#29312);
#26381=PLANE('',#29313);
#26382=PLANE('',#29314);
#26383=PLANE('',#29315);
#26384=PLANE('',#29318);
#26385=PLANE('',#29319);
#26386=PLANE('',#29320);
#26387=PLANE('',#29323);
#26388=PLANE('',#29324);
#26389=PLANE('',#29325);
#26390=PLANE('',#29336);
#26391=PLANE('',#29337);
#26392=PLANE('',#29338);
#26393=PLANE('',#29339);
#26394=PLANE('',#29340);
#26395=PLANE('',#29341);
#26396=PLANE('',#29342);
#26397=PLANE('',#29343);
#26398=PLANE('',#29344);
#26399=PLANE('',#29345);
#26400=PLANE('',#29350);
#26401=PLANE('',#29354);
#26402=PLANE('',#29358);
#26403=PLANE('',#29362);
#26404=PLANE('',#29363);
#26405=PLANE('',#29366);
#26406=PLANE('',#29369);
#26407=PLANE('',#29373);
#26408=PLANE('',#29377);
#26409=PLANE('',#29378);
#26410=PLANE('',#29381);
#26411=PLANE('',#29385);
#26412=PLANE('',#29389);
#26413=PLANE('',#29394);
#26414=PLANE('',#29397);
#26415=PLANE('',#29400);
#26416=PLANE('',#29401);
#26417=PLANE('',#29405);
#26418=PLANE('',#29409);
#26419=PLANE('',#29410);
#26420=PLANE('',#29412);
#26421=PLANE('',#29413);
#26422=PLANE('',#29417);
#26423=PLANE('',#29421);
#26424=PLANE('',#29422);
#26425=PLANE('',#29424);
#26426=PLANE('',#29428);
#26427=PLANE('',#29432);
#26428=PLANE('',#29433);
#26429=PLANE('',#29435);
#26430=PLANE('',#29439);
#26431=PLANE('',#29443);
#26432=PLANE('',#29444);
#26433=PLANE('',#29446);
#26434=PLANE('',#29448);
#26435=PLANE('',#29449);
#26436=PLANE('',#29454);
#26437=PLANE('',#29469);
#26438=PLANE('',#29471);
#26439=PLANE('',#29473);
#26440=PLANE('',#29474);
#26441=PLANE('',#29475);
#26442=PLANE('',#29477);
#26443=PLANE('',#29479);
#26444=PLANE('',#29480);
#26445=PLANE('',#29482);
#26446=PLANE('',#29494);
#26447=PLANE('',#29496);
#26448=PLANE('',#29498);
#26449=PLANE('',#29500);
#26450=PLANE('',#29507);
#26451=PLANE('',#29514);
#26452=PLANE('',#29517);
#26453=PLANE('',#29521);
#26454=PLANE('',#29525);
#26455=PLANE('',#29529);
#26456=PLANE('',#29530);
#26457=PLANE('',#29532);
#26458=PLANE('',#29534);
#26459=PLANE('',#29548);
#26460=PLANE('',#29549);
#26461=PLANE('',#29550);
#26462=PLANE('',#29552);
#26463=PLANE('',#29553);
#26464=PLANE('',#29554);
#26465=PLANE('',#29556);
#26466=PLANE('',#29557);
#26467=PLANE('',#29558);
#26468=PLANE('',#29560);
#26469=PLANE('',#29561);
#26470=PLANE('',#29562);
#26471=PLANE('',#29564);
#26472=PLANE('',#29565);
#26473=PLANE('',#29566);
#26474=PLANE('',#29568);
#26475=PLANE('',#29569);
#26476=PLANE('',#29570);
#26477=PLANE('',#29573);
#26478=PLANE('',#29574);
#26479=PLANE('',#29575);
#26480=PLANE('',#29577);
#26481=PLANE('',#29578);
#26482=PLANE('',#29579);
#26483=PLANE('',#29581);
#26484=PLANE('',#29582);
#26485=PLANE('',#29583);
#26486=PLANE('',#29585);
#26487=PLANE('',#29586);
#26488=PLANE('',#29587);
#26489=PLANE('',#29589);
#26490=PLANE('',#29590);
#26491=PLANE('',#29591);
#26492=PLANE('',#29593);
#26493=PLANE('',#29594);
#26494=PLANE('',#29595);
#26495=PLANE('',#29597);
#26496=PLANE('',#29598);
#26497=PLANE('',#29599);
#26498=PLANE('',#29601);
#26499=PLANE('',#29602);
#26500=PLANE('',#29603);
#26501=PLANE('',#29605);
#26502=PLANE('',#29606);
#26503=PLANE('',#29607);
#26504=PLANE('',#29609);
#26505=PLANE('',#29610);
#26506=PLANE('',#29611);
#26507=PLANE('',#29613);
#26508=PLANE('',#29614);
#26509=PLANE('',#29615);
#26510=PLANE('',#29617);
#26511=PLANE('',#29618);
#26512=PLANE('',#29619);
#26513=PLANE('',#29621);
#26514=PLANE('',#29622);
#26515=PLANE('',#29623);
#26516=PLANE('',#29625);
#26517=PLANE('',#29626);
#26518=PLANE('',#29627);
#26519=PLANE('',#29629);
#26520=PLANE('',#29630);
#26521=PLANE('',#29631);
#26522=PLANE('',#29633);
#26523=PLANE('',#29634);
#26524=PLANE('',#29635);
#26525=PLANE('',#29637);
#26526=PLANE('',#29638);
#26527=PLANE('',#29639);
#26528=PLANE('',#29641);
#26529=PLANE('',#29642);
#26530=PLANE('',#29643);
#26531=PLANE('',#29721);
#26532=PLANE('',#29729);
#26533=PLANE('',#29730);
#26534=PLANE('',#29735);
#26535=PLANE('',#29769);
#26536=PLANE('',#29770);
#26537=PLANE('',#29772);
#26538=PLANE('',#29773);
#26539=PLANE('',#29774);
#26540=PLANE('',#29776);
#26541=PLANE('',#29777);
#26542=PLANE('',#29778);
#26543=PLANE('',#29780);
#26544=PLANE('',#29781);
#26545=PLANE('',#29782);
#26546=PLANE('',#29784);
#26547=PLANE('',#29785);
#26548=PLANE('',#29786);
#26549=PLANE('',#29788);
#26550=PLANE('',#29789);
#26551=PLANE('',#29790);
#26552=PLANE('',#29792);
#26553=PLANE('',#29793);
#26554=PLANE('',#29794);
#26555=PLANE('',#29796);
#26556=PLANE('',#29797);
#26557=PLANE('',#29798);
#26558=PLANE('',#29800);
#26559=PLANE('',#29801);
#26560=PLANE('',#29802);
#26561=PLANE('',#29804);
#26562=PLANE('',#29805);
#26563=PLANE('',#29806);
#26564=PLANE('',#29808);
#26565=PLANE('',#29809);
#26566=PLANE('',#29810);
#26567=PLANE('',#29812);
#26568=PLANE('',#29813);
#26569=PLANE('',#29814);
#26570=PLANE('',#29816);
#26571=PLANE('',#29817);
#26572=PLANE('',#29818);
#26573=PLANE('',#29820);
#26574=PLANE('',#29821);
#26575=PLANE('',#29822);
#26576=PLANE('',#29825);
#26577=PLANE('',#29826);
#26578=PLANE('',#29827);
#26579=PLANE('',#29829);
#26580=PLANE('',#29830);
#26581=PLANE('',#29831);
#26582=PLANE('',#29833);
#26583=PLANE('',#29834);
#26584=PLANE('',#29835);
#26585=PLANE('',#29837);
#26586=PLANE('',#29838);
#26587=PLANE('',#29839);
#26588=PLANE('',#29841);
#26589=PLANE('',#29862);
#26590=PLANE('',#29867);
#26591=PLANE('',#29872);
#26592=PLANE('',#29877);
#26593=PLANE('',#29882);
#26594=PLANE('',#29883);
#26595=PLANE('',#29885);
#26596=PLANE('',#29886);
#26597=PLANE('',#29887);
#26598=PLANE('',#29888);
#26599=PLANE('',#29889);
#26600=PLANE('',#29890);
#26601=PLANE('',#29891);
#26602=PLANE('',#29892);
#26603=PLANE('',#29894);
#26604=PLANE('',#29901);
#26605=PLANE('',#29902);
#26606=PLANE('',#29903);
#26607=PLANE('',#29907);
#26608=PLANE('',#29908);
#26609=PLANE('',#29909);
#26610=PLANE('',#29910);
#26611=PLANE('',#29911);
#26612=PLANE('',#29912);
#26613=PLANE('',#29913);
#26614=PLANE('',#29914);
#26615=PLANE('',#29915);
#26616=PLANE('',#29916);
#26617=PLANE('',#29917);
#26618=PLANE('',#29918);
#26619=PLANE('',#29919);
#26620=PLANE('',#29920);
#26621=PLANE('',#29921);
#26622=PLANE('',#29922);
#26623=PLANE('',#29923);
#26624=PLANE('',#29924);
#26625=PLANE('',#29925);
#26626=PLANE('',#29926);
#26627=PLANE('',#29927);
#26628=PLANE('',#29928);
#26629=PLANE('',#29929);
#26630=PLANE('',#29930);
#26631=PLANE('',#29931);
#26632=PLANE('',#29932);
#26633=PLANE('',#29933);
#26634=PLANE('',#29934);
#26635=PLANE('',#29935);
#26636=PLANE('',#29936);
#26637=PLANE('',#29937);
#26638=PLANE('',#29938);
#26639=PLANE('',#29939);
#26640=PLANE('',#29940);
#26641=PLANE('',#29941);
#26642=PLANE('',#29942);
#26643=PLANE('',#29943);
#26644=PLANE('',#29944);
#26645=PLANE('',#29945);
#26646=PLANE('',#29946);
#26647=PLANE('',#29947);
#26648=PLANE('',#29948);
#26649=PLANE('',#29949);
#26650=PLANE('',#29950);
#26651=PLANE('',#29951);
#26652=PLANE('',#29952);
#26653=PLANE('',#29953);
#26654=PLANE('',#29954);
#26655=PLANE('',#29955);
#26656=PLANE('',#29956);
#26657=PLANE('',#29957);
#26658=PLANE('',#29958);
#26659=PLANE('',#29959);
#26660=PLANE('',#29960);
#26661=PLANE('',#29961);
#26662=PLANE('',#29962);
#26663=PLANE('',#29963);
#26664=PLANE('',#29964);
#26665=PLANE('',#29965);
#26666=PLANE('',#29969);
#26667=PLANE('',#29975);
#26668=PLANE('',#29981);
#26669=PLANE('',#29993);
#26670=PLANE('',#29996);
#26671=PLANE('',#30004);
#26672=PLANE('',#30007);
#26673=PLANE('',#30011);
#26674=PLANE('',#30012);
#26675=PLANE('',#30014);
#26676=PLANE('',#30015);
#26677=PLANE('',#30016);
#26678=PLANE('',#30017);
#26679=PLANE('',#30018);
#26680=PLANE('',#30019);
#26681=PLANE('',#30020);
#26682=PLANE('',#30021);
#26683=PLANE('',#30022);
#26684=PLANE('',#30023);
#26685=PLANE('',#30024);
#26686=PLANE('',#30025);
#26687=PLANE('',#30026);
#26688=PLANE('',#30027);
#26689=PLANE('',#30028);
#26690=PLANE('',#30029);
#26691=PLANE('',#30030);
#26692=PLANE('',#30031);
#26693=PLANE('',#30032);
#26694=PLANE('',#30033);
#26695=PLANE('',#30034);
#26696=PLANE('',#30035);
#26697=PLANE('',#30036);
#26698=PLANE('',#30037);
#26699=PLANE('',#30038);
#26700=PLANE('',#30039);
#26701=PLANE('',#30040);
#26702=PLANE('',#30041);
#26703=PLANE('',#30042);
#26704=PLANE('',#30043);
#26705=PLANE('',#30044);
#26706=PLANE('',#30045);
#26707=PLANE('',#30046);
#26708=PLANE('',#30047);
#26709=PLANE('',#30051);
#26710=PLANE('',#30055);
#26711=PLANE('',#30059);
#26712=PLANE('',#30063);
#26713=PLANE('',#30064);
#26714=PLANE('',#30067);
#26715=PLANE('',#30070);
#26716=PLANE('',#30073);
#26717=PLANE('',#30074);
#26718=PLANE('',#30075);
#26719=PLANE('',#30076);
#26720=PLANE('',#30077);
#26721=PLANE('',#30080);
#26722=PLANE('',#30081);
#26723=PLANE('',#30082);
#26724=PLANE('',#30083);
#26725=PLANE('',#30084);
#26726=PLANE('',#30087);
#26727=PLANE('',#30088);
#26728=PLANE('',#30089);
#26729=PLANE('',#30095);
#26730=PLANE('',#30104);
#26731=PLANE('',#30124);
#26732=PLANE('',#30128);
#26733=PLANE('',#30132);
#26734=PLANE('',#30133);
#26735=PLANE('',#30138);
#26736=PLANE('',#30141);
#26737=PLANE('',#30144);
#26738=PLANE('',#30147);
#26739=PLANE('',#30148);
#26740=PLANE('',#30149);
#26741=PLANE('',#30151);
#26742=PLANE('',#30153);
#26743=PLANE('',#30156);
#26744=PLANE('',#30159);
#26745=PLANE('',#30160);
#26746=PLANE('',#30162);
#26747=PLANE('',#30168);
#26748=PLANE('',#30172);
#26749=PLANE('',#30173);
#26750=PLANE('',#30179);
#26751=PLANE('',#30181);
#26752=PLANE('',#30213);
#26753=PLANE('',#30217);
#26754=PLANE('',#30222);
#26755=PLANE('',#30223);
#26756=PLANE('',#30231);
#26757=PLANE('',#30234);
#26758=PLANE('',#30239);
#26759=PLANE('',#30240);
#26760=PLANE('',#30241);
#26761=PLANE('',#30242);
#26762=PLANE('',#30243);
#26763=PLANE('',#30244);
#26764=PLANE('',#30245);
#26765=PLANE('',#30246);
#26766=PLANE('',#30247);
#26767=PLANE('',#30248);
#26768=PLANE('',#30249);
#26769=PLANE('',#30250);
#26770=PLANE('',#30251);
#26771=PLANE('',#30252);
#26772=PLANE('',#30253);
#26773=PLANE('',#30254);
#26774=PLANE('',#30255);
#26775=PLANE('',#30256);
#26776=PLANE('',#30257);
#26777=PLANE('',#30258);
#26778=PLANE('',#30259);
#26779=PLANE('',#30260);
#26780=PLANE('',#30261);
#26781=PLANE('',#30262);
#26782=PLANE('',#30263);
#26783=PLANE('',#30264);
#26784=PLANE('',#30265);
#26785=PLANE('',#30266);
#26786=PLANE('',#30267);
#26787=PLANE('',#30268);
#26788=PLANE('',#30269);
#26789=PLANE('',#30270);
#26790=PLANE('',#30271);
#26791=PLANE('',#30272);
#26792=PLANE('',#30273);
#26793=PLANE('',#30274);
#26794=PLANE('',#30275);
#26795=PLANE('',#30276);
#26796=PLANE('',#30277);
#26797=PLANE('',#30278);
#26798=PLANE('',#30279);
#26799=PLANE('',#30280);
#26800=PLANE('',#30281);
#26801=PLANE('',#30282);
#26802=PLANE('',#30283);
#26803=PLANE('',#30407);
#26804=PLANE('',#30408);
#26805=PLANE('',#30409);
#26806=PLANE('',#30410);
#26807=PLANE('',#30411);
#26808=PLANE('',#30412);
#26809=PLANE('',#30413);
#26810=PLANE('',#30414);
#26811=PLANE('',#30415);
#26812=PLANE('',#30416);
#26813=PLANE('',#30417);
#26814=PLANE('',#30418);
#26815=PLANE('',#30421);
#26816=PLANE('',#30430);
#26817=PLANE('',#30434);
#26818=PLANE('',#30435);
#26819=PLANE('',#30436);
#26820=PLANE('',#30437);
#26821=PLANE('',#30438);
#26822=PLANE('',#30439);
#26823=PLANE('',#30440);
#26824=PLANE('',#30441);
#26825=PLANE('',#30450);
#26826=PLANE('',#30454);
#26827=PLANE('',#30457);
#26828=PLANE('',#30458);
#26829=PLANE('',#30459);
#26830=PLANE('',#30461);
#26831=PLANE('',#30462);
#26832=PLANE('',#30463);
#26833=PLANE('',#30468);
#26834=PLANE('',#30474);
#26835=PLANE('',#30485);
#26836=PLANE('',#30496);
#26837=PLANE('',#30500);
#26838=PLANE('',#30508);
#26839=PLANE('',#30510);
#26840=PLANE('',#30514);
#26841=PLANE('',#30518);
#26842=PLANE('',#30522);
#26843=PLANE('',#30526);
#26844=PLANE('',#30530);
#26845=PLANE('',#30531);
#26846=PLANE('',#30539);
#26847=PLANE('',#30542);
#26848=PLANE('',#30543);
#26849=PLANE('',#30544);
#26850=PLANE('',#30547);
#26851=PLANE('',#30550);
#26852=PLANE('',#30552);
#26853=PLANE('',#30557);
#26854=PLANE('',#30597);
#26855=PLANE('',#30626);
#26856=PLANE('',#30630);
#26857=PLANE('',#30634);
#26858=PLANE('',#30638);
#26859=PLANE('',#30644);
#26860=PLANE('',#30647);
#26861=PLANE('',#30690);
#26862=PLANE('',#30711);
#26863=PLANE('',#30726);
#26864=PLANE('',#30729);
#26865=PLANE('',#30732);
#26866=PLANE('',#30735);
#26867=PLANE('',#30740);
#26868=PLANE('',#30758);
#26869=PLANE('',#30762);
#26870=PLANE('',#30765);
#26871=PLANE('',#30768);
#26872=PLANE('',#30770);
#26873=PLANE('',#30777);
#26874=PLANE('',#30780);
#26875=PLANE('',#30782);
#26876=PLANE('',#30784);
#26877=PLANE('',#30787);
#26878=PLANE('',#30788);
#26879=ADVANCED_FACE('',(#2971),#26071,.T.);
#26880=ADVANCED_FACE('',(#2972),#26072,.T.);
#26881=ADVANCED_FACE('',(#2973),#26073,.T.);
#26882=ADVANCED_FACE('',(#2974),#26074,.T.);
#26883=ADVANCED_FACE('',(#2975),#26075,.T.);
#26884=ADVANCED_FACE('',(#2976),#26076,.T.);
#26885=ADVANCED_FACE('',(#2977),#26077,.T.);
#26886=ADVANCED_FACE('',(#2978),#26078,.T.);
#26887=ADVANCED_FACE('',(#2979),#26079,.T.);
#26888=ADVANCED_FACE('',(#2980),#26080,.T.);
#26889=ADVANCED_FACE('',(#2981),#26081,.T.);
#26890=ADVANCED_FACE('',(#2982),#26082,.T.);
#26891=ADVANCED_FACE('',(#2983),#26083,.T.);
#26892=ADVANCED_FACE('',(#2984),#26084,.T.);
#26893=ADVANCED_FACE('',(#2985),#2731,.F.);
#26894=ADVANCED_FACE('',(#2986,#1874,#1875,#1876,#1877),#26085,.T.);
#26895=ADVANCED_FACE('',(#2987),#1532,.F.);
#26896=ADVANCED_FACE('',(#2988),#2732,.F.);
#26897=ADVANCED_FACE('',(#2989),#1533,.F.);
#26898=ADVANCED_FACE('',(#2990),#2733,.F.);
#26899=ADVANCED_FACE('',(#2991),#1534,.F.);
#26900=ADVANCED_FACE('',(#2992),#2734,.F.);
#26901=ADVANCED_FACE('',(#2993),#1535,.F.);
#26902=ADVANCED_FACE('',(#2994),#2735,.F.);
#26903=ADVANCED_FACE('',(#2995,#1878,#1879,#1880,#1881),#26086,.T.);
#26904=ADVANCED_FACE('',(#2996),#2736,.F.);
#26905=ADVANCED_FACE('',(#2997),#2737,.F.);
#26906=ADVANCED_FACE('',(#2998),#2738,.F.);
#26907=ADVANCED_FACE('',(#2999),#2739,.F.);
#26908=ADVANCED_FACE('',(#3000,#1882,#1883,#1884,#1885),#26087,.T.);
#26909=ADVANCED_FACE('',(#3001),#1536,.F.);
#26910=ADVANCED_FACE('',(#3002),#2740,.F.);
#26911=ADVANCED_FACE('',(#3003),#1537,.F.);
#26912=ADVANCED_FACE('',(#3004),#2741,.F.);
#26913=ADVANCED_FACE('',(#3005),#1538,.F.);
#26914=ADVANCED_FACE('',(#3006),#2742,.F.);
#26915=ADVANCED_FACE('',(#3007),#1539,.F.);
#26916=ADVANCED_FACE('',(#3008),#2743,.F.);
#26917=ADVANCED_FACE('',(#3009),#1348,.T.);
#26918=ADVANCED_FACE('',(#3010),#1349,.T.);
#26919=ADVANCED_FACE('',(#3011),#1350,.T.);
#26920=ADVANCED_FACE('',(#3012),#1540,.T.);
#26921=ADVANCED_FACE('',(#3013),#1541,.F.);
#26922=ADVANCED_FACE('',(#3014),#2744,.F.);
#26923=ADVANCED_FACE('',(#3015,#1886,#1887,#1888,#1889),#26088,.T.);
#26924=ADVANCED_FACE('',(#3016),#2745,.F.);
#26925=ADVANCED_FACE('',(#3017),#2746,.F.);
#26926=ADVANCED_FACE('',(#3018),#2747,.F.);
#26927=ADVANCED_FACE('',(#3019),#2748,.T.);
#26928=ADVANCED_FACE('',(#3020),#26089,.T.);
#26929=ADVANCED_FACE('',(#3021),#2749,.T.);
#26930=ADVANCED_FACE('',(#3022),#26090,.T.);
#26931=ADVANCED_FACE('',(#3023),#2750,.T.);
#26932=ADVANCED_FACE('',(#3024),#26091,.T.);
#26933=ADVANCED_FACE('',(#3025),#2751,.T.);
#26934=ADVANCED_FACE('',(#3026),#26092,.T.);
#26935=ADVANCED_FACE('',(#3027),#1542,.T.);
#26936=ADVANCED_FACE('',(#3028),#26093,.T.);
#26937=ADVANCED_FACE('',(#3029),#1543,.T.);
#26938=ADVANCED_FACE('',(#3030,#1890),#26094,.T.);
#26939=ADVANCED_FACE('',(#3031),#2752,.T.);
#26940=ADVANCED_FACE('',(#3032),#26095,.T.);
#26941=ADVANCED_FACE('',(#3033),#2753,.T.);
#26942=ADVANCED_FACE('',(#3034),#26096,.T.);
#26943=ADVANCED_FACE('',(#3035),#2754,.T.);
#26944=ADVANCED_FACE('',(#3036),#26097,.T.);
#26945=ADVANCED_FACE('',(#3037),#2755,.T.);
#26946=ADVANCED_FACE('',(#3038),#26098,.T.);
#26947=ADVANCED_FACE('',(#3039),#26099,.T.);
#26948=ADVANCED_FACE('',(#3040,#1891,#1892,#1893,#1894,#1895),#26100,.T.);
#26949=ADVANCED_FACE('',(#3041,#1896),#26101,.F.);
#26950=ADVANCED_FACE('',(#3042),#2756,.F.);
#26951=ADVANCED_FACE('',(#3043),#1351,.T.);
#26952=ADVANCED_FACE('',(#3044),#1352,.T.);
#26953=ADVANCED_FACE('',(#3045),#1353,.T.);
#26954=ADVANCED_FACE('',(#3046),#1544,.F.);
#26955=ADVANCED_FACE('',(#3047),#2757,.F.);
#26956=ADVANCED_FACE('',(#3048),#1354,.T.);
#26957=ADVANCED_FACE('',(#3049),#1355,.T.);
#26958=ADVANCED_FACE('',(#3050),#1356,.T.);
#26959=ADVANCED_FACE('',(#3051),#1545,.F.);
#26960=ADVANCED_FACE('',(#3052),#26102,.T.);
#26961=ADVANCED_FACE('',(#3053),#2758,.F.);
#26962=ADVANCED_FACE('',(#3054),#26103,.T.);
#26963=ADVANCED_FACE('',(#3055),#2759,.F.);
#26964=ADVANCED_FACE('',(#3056),#26104,.T.);
#26965=ADVANCED_FACE('',(#3057),#2760,.F.);
#26966=ADVANCED_FACE('',(#3058),#26105,.T.);
#26967=ADVANCED_FACE('',(#3059),#2761,.F.);
#26968=ADVANCED_FACE('',(#3060),#1546,.F.);
#26969=ADVANCED_FACE('',(#3061),#26106,.T.);
#26970=ADVANCED_FACE('',(#3062),#1547,.F.);
#26971=ADVANCED_FACE('',(#3063),#26107,.T.);
#26972=ADVANCED_FACE('',(#3064),#1357,.T.);
#26973=ADVANCED_FACE('',(#3065),#2762,.F.);
#26974=ADVANCED_FACE('',(#3066),#1358,.T.);
#26975=ADVANCED_FACE('',(#3067),#1359,.T.);
#26976=ADVANCED_FACE('',(#3068),#26108,.T.);
#26977=ADVANCED_FACE('',(#3069),#2763,.F.);
#26978=ADVANCED_FACE('',(#3070),#26109,.T.);
#26979=ADVANCED_FACE('',(#3071),#2764,.F.);
#26980=ADVANCED_FACE('',(#3072),#26110,.T.);
#26981=ADVANCED_FACE('',(#3073),#2765,.F.);
#26982=ADVANCED_FACE('',(#3074),#26111,.T.);
#26983=ADVANCED_FACE('',(#3075),#2766,.F.);
#26984=ADVANCED_FACE('',(#3076),#1548,.F.);
#26985=ADVANCED_FACE('',(#3077),#26112,.T.);
#26986=ADVANCED_FACE('',(#3078),#1549,.F.);
#26987=ADVANCED_FACE('',(#3079),#1360,.T.);
#26988=ADVANCED_FACE('',(#3080),#2767,.F.);
#26989=ADVANCED_FACE('',(#3081),#1361,.T.);
#26990=ADVANCED_FACE('',(#3082),#1362,.T.);
#26991=ADVANCED_FACE('',(#3083),#1363,.T.);
#26992=ADVANCED_FACE('',(#3084),#2768,.F.);
#26993=ADVANCED_FACE('',(#3085),#1364,.T.);
#26994=ADVANCED_FACE('',(#3086),#1365,.T.);
#26995=ADVANCED_FACE('',(#3087),#2769,.F.);
#26996=ADVANCED_FACE('',(#3088),#1366,.T.);
#26997=ADVANCED_FACE('',(#3089),#1367,.T.);
#26998=ADVANCED_FACE('',(#3090),#1368,.T.);
#26999=ADVANCED_FACE('',(#3091),#1550,.F.);
#27000=ADVANCED_FACE('',(#3092),#1369,.T.);
#27001=ADVANCED_FACE('',(#3093),#2770,.F.);
#27002=ADVANCED_FACE('',(#3094),#1370,.T.);
#27003=ADVANCED_FACE('',(#3095),#1371,.T.);
#27004=ADVANCED_FACE('',(#3096),#2771,.T.);
#27005=ADVANCED_FACE('',(#3097),#26113,.T.);
#27006=ADVANCED_FACE('',(#3098),#2772,.T.);
#27007=ADVANCED_FACE('',(#3099),#26114,.T.);
#27008=ADVANCED_FACE('',(#3100),#2773,.T.);
#27009=ADVANCED_FACE('',(#3101),#26115,.T.);
#27010=ADVANCED_FACE('',(#3102),#2774,.T.);
#27011=ADVANCED_FACE('',(#3103),#26116,.T.);
#27012=ADVANCED_FACE('',(#3104),#1551,.T.);
#27013=ADVANCED_FACE('',(#3105),#26117,.T.);
#27014=ADVANCED_FACE('',(#3106),#1552,.T.);
#27015=ADVANCED_FACE('',(#3107,#1897),#26118,.F.);
#27016=ADVANCED_FACE('',(#3108),#2775,.T.);
#27017=ADVANCED_FACE('',(#3109),#26119,.T.);
#27018=ADVANCED_FACE('',(#3110),#2776,.T.);
#27019=ADVANCED_FACE('',(#3111),#26120,.T.);
#27020=ADVANCED_FACE('',(#3112),#2777,.T.);
#27021=ADVANCED_FACE('',(#3113),#26121,.T.);
#27022=ADVANCED_FACE('',(#3114),#2778,.T.);
#27023=ADVANCED_FACE('',(#3115),#26122,.T.);
#27024=ADVANCED_FACE('',(#3116),#26123,.T.);
#27025=ADVANCED_FACE('',(#3117),#1553,.T.);
#27026=ADVANCED_FACE('',(#3118),#26124,.T.);
#27027=ADVANCED_FACE('',(#3119,#1898),#26125,.T.);
#27028=ADVANCED_FACE('',(#3120),#1372,.T.);
#27029=ADVANCED_FACE('',(#3121),#2779,.F.);
#27030=ADVANCED_FACE('',(#3122),#1373,.T.);
#27031=ADVANCED_FACE('',(#3123),#1374,.T.);
#27032=ADVANCED_FACE('',(#3124),#1554,.F.);
#27033=ADVANCED_FACE('',(#3125),#26126,.T.);
#27034=ADVANCED_FACE('',(#3126),#2780,.F.);
#27035=ADVANCED_FACE('',(#3127),#26127,.T.);
#27036=ADVANCED_FACE('',(#3128),#2781,.F.);
#27037=ADVANCED_FACE('',(#3129),#26128,.T.);
#27038=ADVANCED_FACE('',(#3130),#2782,.F.);
#27039=ADVANCED_FACE('',(#3131),#26129,.T.);
#27040=ADVANCED_FACE('',(#3132),#2783,.F.);
#27041=ADVANCED_FACE('',(#3133),#1555,.F.);
#27042=ADVANCED_FACE('',(#3134),#26130,.T.);
#27043=ADVANCED_FACE('',(#3135),#1556,.F.);
#27044=ADVANCED_FACE('',(#3136),#26131,.T.);
#27045=ADVANCED_FACE('',(#3137),#26132,.T.);
#27046=ADVANCED_FACE('',(#3138),#2784,.F.);
#27047=ADVANCED_FACE('',(#3139),#26133,.T.);
#27048=ADVANCED_FACE('',(#3140),#2785,.F.);
#27049=ADVANCED_FACE('',(#3141),#26134,.T.);
#27050=ADVANCED_FACE('',(#3142),#2786,.F.);
#27051=ADVANCED_FACE('',(#3143),#26135,.T.);
#27052=ADVANCED_FACE('',(#3144),#2787,.F.);
#27053=ADVANCED_FACE('',(#3145),#1557,.F.);
#27054=ADVANCED_FACE('',(#3146),#26136,.T.);
#27055=ADVANCED_FACE('',(#3147),#1558,.F.);
#27056=ADVANCED_FACE('',(#3148),#1375,.T.);
#27057=ADVANCED_FACE('',(#3149),#2788,.F.);
#27058=ADVANCED_FACE('',(#3150),#1376,.T.);
#27059=ADVANCED_FACE('',(#3151),#1377,.T.);
#27060=ADVANCED_FACE('',(#3152),#2789,.F.);
#27061=ADVANCED_FACE('',(#3153),#1378,.T.);
#27062=ADVANCED_FACE('',(#3154),#1379,.T.);
#27063=ADVANCED_FACE('',(#3155),#1380,.T.);
#27064=ADVANCED_FACE('',(#3156),#1559,.F.);
#27065=ADVANCED_FACE('',(#3157),#1381,.T.);
#27066=ADVANCED_FACE('',(#3158),#2790,.F.);
#27067=ADVANCED_FACE('',(#3159),#1382,.T.);
#27068=ADVANCED_FACE('',(#3160),#1383,.T.);
#27069=ADVANCED_FACE('',(#3161),#1384,.T.);
#27070=ADVANCED_FACE('',(#3162),#2791,.F.);
#27071=ADVANCED_FACE('',(#3163),#1385,.T.);
#27072=ADVANCED_FACE('',(#3164),#1386,.T.);
#27073=ADVANCED_FACE('',(#3165),#1560,.F.);
#27074=ADVANCED_FACE('',(#3166),#1387,.T.);
#27075=ADVANCED_FACE('',(#3167),#2792,.F.);
#27076=ADVANCED_FACE('',(#3168),#1388,.T.);
#27077=ADVANCED_FACE('',(#3169),#1389,.T.);
#27078=ADVANCED_FACE('',(#3170),#2793,.F.);
#27079=ADVANCED_FACE('',(#3171),#1390,.T.);
#27080=ADVANCED_FACE('',(#3172),#1391,.T.);
#27081=ADVANCED_FACE('',(#3173),#1392,.T.);
#27082=ADVANCED_FACE('',(#3174),#1561,.F.);
#27083=ADVANCED_FACE('',(#3175),#1393,.T.);
#27084=ADVANCED_FACE('',(#3176),#2794,.F.);
#27085=ADVANCED_FACE('',(#3177),#1394,.T.);
#27086=ADVANCED_FACE('',(#3178),#1395,.T.);
#27087=ADVANCED_FACE('',(#3179),#2795,.F.);
#27088=ADVANCED_FACE('',(#3180),#1562,.F.);
#27089=ADVANCED_FACE('',(#3181,#1899,#1900),#26137,.F.);
#27090=ADVANCED_FACE('',(#3182),#2796,.F.);
#27091=ADVANCED_FACE('',(#3183,#1901,#1902),#26138,.T.);
#27092=ADVANCED_FACE('',(#3184),#2797,.F.);
#27093=ADVANCED_FACE('',(#3185),#1563,.F.);
#27094=ADVANCED_FACE('',(#3186),#2798,.F.);
#27095=ADVANCED_FACE('',(#3187),#1396,.F.);
#27096=ADVANCED_FACE('',(#3188),#1397,.F.);
#27097=ADVANCED_FACE('',(#3189),#1398,.F.);
#27098=ADVANCED_FACE('',(#3190),#1399,.F.);
#27099=ADVANCED_FACE('',(#3191),#1400,.F.);
#27100=ADVANCED_FACE('',(#3192),#1401,.F.);
#27101=ADVANCED_FACE('',(#3193),#1402,.F.);
#27102=ADVANCED_FACE('',(#3194),#1403,.F.);
#27103=ADVANCED_FACE('',(#3195),#1404,.F.);
#27104=ADVANCED_FACE('',(#3196),#1405,.F.);
#27105=ADVANCED_FACE('',(#3197),#1406,.F.);
#27106=ADVANCED_FACE('',(#3198),#1407,.F.);
#27107=ADVANCED_FACE('',(#3199),#1408,.F.);
#27108=ADVANCED_FACE('',(#3200),#1409,.F.);
#27109=ADVANCED_FACE('',(#3201),#1410,.F.);
#27110=ADVANCED_FACE('',(#3202),#1411,.F.);
#27111=ADVANCED_FACE('',(#3203),#1412,.F.);
#27112=ADVANCED_FACE('',(#3204),#1413,.F.);
#27113=ADVANCED_FACE('',(#3205,#1903),#26139,.F.);
#27114=ADVANCED_FACE('',(#3206),#26140,.F.);
#27115=ADVANCED_FACE('',(#3207),#26141,.F.);
#27116=ADVANCED_FACE('',(#3208),#26142,.F.);
#27117=ADVANCED_FACE('',(#3209),#26143,.F.);
#27118=ADVANCED_FACE('',(#3210),#26144,.F.);
#27119=ADVANCED_FACE('',(#3211),#26145,.F.);
#27120=ADVANCED_FACE('',(#3212),#26146,.F.);
#27121=ADVANCED_FACE('',(#3213),#26147,.F.);
#27122=ADVANCED_FACE('',(#3214),#26148,.F.);
#27123=ADVANCED_FACE('',(#3215),#1414,.F.);
#27124=ADVANCED_FACE('',(#3216),#1415,.F.);
#27125=ADVANCED_FACE('',(#3217),#1416,.F.);
#27126=ADVANCED_FACE('',(#3218),#1417,.F.);
#27127=ADVANCED_FACE('',(#3219),#1418,.F.);
#27128=ADVANCED_FACE('',(#3220),#1419,.F.);
#27129=ADVANCED_FACE('',(#3221),#1420,.F.);
#27130=ADVANCED_FACE('',(#3222),#1421,.F.);
#27131=ADVANCED_FACE('',(#3223),#1422,.F.);
#27132=ADVANCED_FACE('',(#3224),#1423,.F.);
#27133=ADVANCED_FACE('',(#3225),#1424,.F.);
#27134=ADVANCED_FACE('',(#3226),#1425,.F.);
#27135=ADVANCED_FACE('',(#3227),#1426,.F.);
#27136=ADVANCED_FACE('',(#3228),#1427,.F.);
#27137=ADVANCED_FACE('',(#3229),#1428,.F.);
#27138=ADVANCED_FACE('',(#3230),#1429,.F.);
#27139=ADVANCED_FACE('',(#3231),#1430,.F.);
#27140=ADVANCED_FACE('',(#3232),#1431,.F.);
#27141=ADVANCED_FACE('',(#3233),#1432,.F.);
#27142=ADVANCED_FACE('',(#3234),#1433,.F.);
#27143=ADVANCED_FACE('',(#3235),#1434,.F.);
#27144=ADVANCED_FACE('',(#3236),#1435,.F.);
#27145=ADVANCED_FACE('',(#3237,#1904),#26149,.F.);
#27146=ADVANCED_FACE('',(#3238),#26150,.F.);
#27147=ADVANCED_FACE('',(#3239),#1436,.F.);
#27148=ADVANCED_FACE('',(#3240),#1437,.F.);
#27149=ADVANCED_FACE('',(#3241),#1438,.F.);
#27150=ADVANCED_FACE('',(#3242),#1439,.F.);
#27151=ADVANCED_FACE('',(#3243),#1440,.F.);
#27152=ADVANCED_FACE('',(#3244),#1441,.F.);
#27153=ADVANCED_FACE('',(#3245),#1442,.F.);
#27154=ADVANCED_FACE('',(#3246),#1443,.F.);
#27155=ADVANCED_FACE('',(#3247),#1444,.F.);
#27156=ADVANCED_FACE('',(#3248),#1445,.F.);
#27157=ADVANCED_FACE('',(#3249),#26151,.F.);
#27158=ADVANCED_FACE('',(#3250),#1446,.F.);
#27159=ADVANCED_FACE('',(#3251),#1447,.F.);
#27160=ADVANCED_FACE('',(#3252),#1448,.F.);
#27161=ADVANCED_FACE('',(#3253),#1449,.F.);
#27162=ADVANCED_FACE('',(#3254),#1450,.F.);
#27163=ADVANCED_FACE('',(#3255),#1451,.F.);
#27164=ADVANCED_FACE('',(#3256),#1452,.F.);
#27165=ADVANCED_FACE('',(#3257),#1453,.F.);
#27166=ADVANCED_FACE('',(#3258),#26152,.F.);
#27167=ADVANCED_FACE('',(#3259),#26153,.F.);
#27168=ADVANCED_FACE('',(#3260),#26154,.F.);
#27169=ADVANCED_FACE('',(#3261),#26155,.F.);
#27170=ADVANCED_FACE('',(#3262),#26156,.F.);
#27171=ADVANCED_FACE('',(#3263),#26157,.F.);
#27172=ADVANCED_FACE('',(#3264),#26158,.F.);
#27173=ADVANCED_FACE('',(#3265),#26159,.F.);
#27174=ADVANCED_FACE('',(#3266),#26160,.F.);
#27175=ADVANCED_FACE('',(#3267),#26161,.F.);
#27176=ADVANCED_FACE('',(#3268),#26162,.F.);
#27177=ADVANCED_FACE('',(#3269),#26163,.F.);
#27178=ADVANCED_FACE('',(#3270),#26164,.F.);
#27179=ADVANCED_FACE('',(#3271),#26165,.F.);
#27180=ADVANCED_FACE('',(#3272),#26166,.T.);
#27181=ADVANCED_FACE('',(#3273),#26167,.T.);
#27182=ADVANCED_FACE('',(#3274),#26168,.T.);
#27183=ADVANCED_FACE('',(#3275),#26169,.T.);
#27184=ADVANCED_FACE('',(#3276),#26170,.T.);
#27185=ADVANCED_FACE('',(#3277),#1564,.T.);
#27186=ADVANCED_FACE('',(#3278),#26171,.T.);
#27187=ADVANCED_FACE('',(#3279),#1565,.T.);
#27188=ADVANCED_FACE('',(#3280),#26172,.T.);
#27189=ADVANCED_FACE('',(#3281),#26173,.T.);
#27190=ADVANCED_FACE('',(#3282),#26174,.T.);
#27191=ADVANCED_FACE('',(#3283),#26175,.T.);
#27192=ADVANCED_FACE('',(#3284),#26176,.T.);
#27193=ADVANCED_FACE('',(#3285),#26177,.T.);
#27194=ADVANCED_FACE('',(#3286),#26178,.T.);
#27195=ADVANCED_FACE('',(#3287),#26179,.T.);
#27196=ADVANCED_FACE('',(#3288),#26180,.T.);
#27197=ADVANCED_FACE('',(#3289),#26181,.T.);
#27198=ADVANCED_FACE('',(#3290),#26182,.T.);
#27199=ADVANCED_FACE('',(#3291),#26183,.T.);
#27200=ADVANCED_FACE('',(#3292),#26184,.T.);
#27201=ADVANCED_FACE('',(#3293),#26185,.T.);
#27202=ADVANCED_FACE('',(#3294),#26186,.T.);
#27203=ADVANCED_FACE('',(#3295),#26187,.T.);
#27204=ADVANCED_FACE('',(#3296),#26188,.F.);
#27205=ADVANCED_FACE('',(#3297),#26189,.T.);
#27206=ADVANCED_FACE('',(#3298),#26190,.T.);
#27207=ADVANCED_FACE('',(#3299),#26191,.T.);
#27208=ADVANCED_FACE('',(#3300),#26192,.T.);
#27209=ADVANCED_FACE('',(#3301),#26193,.T.);
#27210=ADVANCED_FACE('',(#3302),#26194,.T.);
#27211=ADVANCED_FACE('',(#3303),#26195,.T.);
#27212=ADVANCED_FACE('',(#3304),#26196,.T.);
#27213=ADVANCED_FACE('',(#3305),#26197,.T.);
#27214=ADVANCED_FACE('',(#3306),#26198,.T.);
#27215=ADVANCED_FACE('',(#3307),#26199,.T.);
#27216=ADVANCED_FACE('',(#3308),#26200,.T.);
#27217=ADVANCED_FACE('',(#3309),#26201,.T.);
#27218=ADVANCED_FACE('',(#3310),#26202,.T.);
#27219=ADVANCED_FACE('',(#3311),#26203,.T.);
#27220=ADVANCED_FACE('',(#3312),#26204,.T.);
#27221=ADVANCED_FACE('',(#3313),#26205,.T.);
#27222=ADVANCED_FACE('',(#3314),#26206,.T.);
#27223=ADVANCED_FACE('',(#3315),#26207,.T.);
#27224=ADVANCED_FACE('',(#3316),#26208,.T.);
#27225=ADVANCED_FACE('',(#3317),#26209,.F.);
#27226=ADVANCED_FACE('',(#3318),#26210,.T.);
#27227=ADVANCED_FACE('',(#3319),#26211,.T.);
#27228=ADVANCED_FACE('',(#3320),#26212,.T.);
#27229=ADVANCED_FACE('',(#3321),#26213,.T.);
#27230=ADVANCED_FACE('',(#3322),#26214,.T.);
#27231=ADVANCED_FACE('',(#3323),#26215,.T.);
#27232=ADVANCED_FACE('',(#3324),#26216,.T.);
#27233=ADVANCED_FACE('',(#3325),#26217,.T.);
#27234=ADVANCED_FACE('',(#3326),#26218,.T.);
#27235=ADVANCED_FACE('',(#3327),#26219,.T.);
#27236=ADVANCED_FACE('',(#3328),#26220,.T.);
#27237=ADVANCED_FACE('',(#3329),#26221,.T.);
#27238=ADVANCED_FACE('',(#3330),#26222,.T.);
#27239=ADVANCED_FACE('',(#3331),#26223,.T.);
#27240=ADVANCED_FACE('',(#3332),#26224,.T.);
#27241=ADVANCED_FACE('',(#3333),#26225,.T.);
#27242=ADVANCED_FACE('',(#3334),#26226,.T.);
#27243=ADVANCED_FACE('',(#3335),#26227,.T.);
#27244=ADVANCED_FACE('',(#3336),#26228,.T.);
#27245=ADVANCED_FACE('',(#3337),#26229,.T.);
#27246=ADVANCED_FACE('',(#3338),#26230,.T.);
#27247=ADVANCED_FACE('',(#3339),#26231,.T.);
#27248=ADVANCED_FACE('',(#3340),#26232,.T.);
#27249=ADVANCED_FACE('',(#3341),#26233,.T.);
#27250=ADVANCED_FACE('',(#3342),#26234,.T.);
#27251=ADVANCED_FACE('',(#3343),#26235,.T.);
#27252=ADVANCED_FACE('',(#3344),#26236,.T.);
#27253=ADVANCED_FACE('',(#3345),#26237,.T.);
#27254=ADVANCED_FACE('',(#3346),#26238,.T.);
#27255=ADVANCED_FACE('',(#3347),#26239,.T.);
#27256=ADVANCED_FACE('',(#3348),#26240,.T.);
#27257=ADVANCED_FACE('',(#3349),#26241,.T.);
#27258=ADVANCED_FACE('',(#3350,#1905,#1906),#26242,.F.);
#27259=ADVANCED_FACE('',(#3351),#26243,.T.);
#27260=ADVANCED_FACE('',(#3352),#26244,.T.);
#27261=ADVANCED_FACE('',(#3353),#26245,.T.);
#27262=ADVANCED_FACE('',(#3354),#26246,.T.);
#27263=ADVANCED_FACE('',(#3355),#26247,.T.);
#27264=ADVANCED_FACE('',(#3356),#26248,.T.);
#27265=ADVANCED_FACE('',(#3357),#26249,.T.);
#27266=ADVANCED_FACE('',(#3358),#26250,.T.);
#27267=ADVANCED_FACE('',(#3359),#26251,.T.);
#27268=ADVANCED_FACE('',(#3360),#26252,.T.);
#27269=ADVANCED_FACE('',(#3361),#26253,.T.);
#27270=ADVANCED_FACE('',(#3362),#26254,.T.);
#27271=ADVANCED_FACE('',(#3363),#26255,.T.);
#27272=ADVANCED_FACE('',(#3364),#26256,.T.);
#27273=ADVANCED_FACE('',(#3365),#26257,.T.);
#27274=ADVANCED_FACE('',(#3366),#26258,.T.);
#27275=ADVANCED_FACE('',(#3367),#26259,.T.);
#27276=ADVANCED_FACE('',(#3368),#26260,.T.);
#27277=ADVANCED_FACE('',(#3369),#26261,.T.);
#27278=ADVANCED_FACE('',(#3370),#26262,.T.);
#27279=ADVANCED_FACE('',(#3371),#26263,.T.);
#27280=ADVANCED_FACE('',(#3372),#26264,.T.);
#27281=ADVANCED_FACE('',(#3373),#26265,.T.);
#27282=ADVANCED_FACE('',(#3374),#26266,.T.);
#27283=ADVANCED_FACE('',(#3375),#26267,.T.);
#27284=ADVANCED_FACE('',(#3376),#26268,.T.);
#27285=ADVANCED_FACE('',(#3377),#26269,.T.);
#27286=ADVANCED_FACE('',(#3378),#26270,.T.);
#27287=ADVANCED_FACE('',(#3379),#2799,.T.);
#27288=ADVANCED_FACE('',(#3380),#2800,.T.);
#27289=ADVANCED_FACE('',(#3381),#1566,.T.);
#27290=ADVANCED_FACE('',(#3382),#2801,.T.);
#27291=ADVANCED_FACE('',(#3383),#26271,.T.);
#27292=ADVANCED_FACE('',(#3384),#2802,.F.);
#27293=ADVANCED_FACE('',(#3385),#1567,.F.);
#27294=ADVANCED_FACE('',(#3386),#2803,.F.);
#27295=ADVANCED_FACE('',(#3387,#1907,#1908),#26272,.T.);
#27296=ADVANCED_FACE('',(#3388),#2804,.F.);
#27297=ADVANCED_FACE('',(#3389),#1568,.F.);
#27298=ADVANCED_FACE('',(#3390),#2805,.F.);
#27299=ADVANCED_FACE('',(#3391),#2806,.T.);
#27300=ADVANCED_FACE('',(#3392),#26273,.T.);
#27301=ADVANCED_FACE('',(#3393),#26274,.T.);
#27302=ADVANCED_FACE('',(#3394,#1909),#26275,.F.);
#27303=ADVANCED_FACE('',(#3395),#26276,.T.);
#27304=ADVANCED_FACE('',(#3396),#26277,.T.);
#27305=ADVANCED_FACE('',(#3397),#26278,.T.);
#27306=ADVANCED_FACE('',(#3398),#26279,.T.);
#27307=ADVANCED_FACE('',(#3399),#26280,.F.);
#27308=ADVANCED_FACE('',(#3400),#26281,.T.);
#27309=ADVANCED_FACE('',(#3401),#26282,.T.);
#27310=ADVANCED_FACE('',(#3402),#26283,.T.);
#27311=ADVANCED_FACE('',(#3403),#26284,.T.);
#27312=ADVANCED_FACE('',(#3404),#26285,.T.);
#27313=ADVANCED_FACE('',(#3405),#26286,.T.);
#27314=ADVANCED_FACE('',(#3406),#26287,.T.);
#27315=ADVANCED_FACE('',(#3407),#26288,.F.);
#27316=ADVANCED_FACE('',(#3408),#26289,.T.);
#27317=ADVANCED_FACE('',(#3409),#26290,.T.);
#27318=ADVANCED_FACE('',(#3410),#26291,.T.);
#27319=ADVANCED_FACE('',(#3411),#26292,.T.);
#27320=ADVANCED_FACE('',(#3412),#26293,.T.);
#27321=ADVANCED_FACE('',(#3413),#26294,.T.);
#27322=ADVANCED_FACE('',(#3414),#26295,.T.);
#27323=ADVANCED_FACE('',(#3415),#26296,.T.);
#27324=ADVANCED_FACE('',(#3416),#26297,.T.);
#27325=ADVANCED_FACE('',(#3417),#26298,.T.);
#27326=ADVANCED_FACE('',(#3418),#26299,.T.);
#27327=ADVANCED_FACE('',(#3419),#26300,.T.);
#27328=ADVANCED_FACE('',(#3420),#26301,.T.);
#27329=ADVANCED_FACE('',(#3421),#26302,.T.);
#27330=ADVANCED_FACE('',(#3422),#26303,.T.);
#27331=ADVANCED_FACE('',(#3423),#26304,.T.);
#27332=ADVANCED_FACE('',(#3424),#26305,.T.);
#27333=ADVANCED_FACE('',(#3425),#26306,.T.);
#27334=ADVANCED_FACE('',(#3426),#26307,.T.);
#27335=ADVANCED_FACE('',(#3427),#26308,.T.);
#27336=ADVANCED_FACE('',(#3428),#26309,.T.);
#27337=ADVANCED_FACE('',(#3429),#26310,.T.);
#27338=ADVANCED_FACE('',(#3430),#26311,.T.);
#27339=ADVANCED_FACE('',(#3431),#26312,.T.);
#27340=ADVANCED_FACE('',(#3432),#26313,.T.);
#27341=ADVANCED_FACE('',(#3433),#26314,.T.);
#27342=ADVANCED_FACE('',(#3434),#26315,.T.);
#27343=ADVANCED_FACE('',(#3435),#26316,.T.);
#27344=ADVANCED_FACE('',(#3436),#26317,.T.);
#27345=ADVANCED_FACE('',(#3437),#26318,.T.);
#27346=ADVANCED_FACE('',(#3438),#26319,.T.);
#27347=ADVANCED_FACE('',(#3439),#26320,.T.);
#27348=ADVANCED_FACE('',(#3440),#26321,.T.);
#27349=ADVANCED_FACE('',(#3441),#26322,.T.);
#27350=ADVANCED_FACE('',(#3442),#26323,.T.);
#27351=ADVANCED_FACE('',(#3443),#26324,.T.);
#27352=ADVANCED_FACE('',(#3444),#26325,.T.);
#27353=ADVANCED_FACE('',(#3445),#26326,.T.);
#27354=ADVANCED_FACE('',(#3446),#26327,.T.);
#27355=ADVANCED_FACE('',(#3447,#1910),#26328,.T.);
#27356=ADVANCED_FACE('',(#3448),#26329,.T.);
#27357=ADVANCED_FACE('',(#3449),#26330,.T.);
#27358=ADVANCED_FACE('',(#3450),#26331,.T.);
#27359=ADVANCED_FACE('',(#3451),#26332,.T.);
#27360=ADVANCED_FACE('',(#3452,#1911),#26333,.T.);
#27361=ADVANCED_FACE('',(#3453),#26334,.T.);
#27362=ADVANCED_FACE('',(#3454),#26335,.T.);
#27363=ADVANCED_FACE('',(#3455),#26336,.T.);
#27364=ADVANCED_FACE('',(#3456),#26337,.T.);
#27365=ADVANCED_FACE('',(#3457),#26338,.F.);
#27366=ADVANCED_FACE('',(#3458),#26339,.T.);
#27367=ADVANCED_FACE('',(#3459),#26340,.T.);
#27368=ADVANCED_FACE('',(#3460),#26341,.T.);
#27369=ADVANCED_FACE('',(#3461),#26342,.T.);
#27370=ADVANCED_FACE('',(#3462),#26343,.T.);
#27371=ADVANCED_FACE('',(#3463),#26344,.T.);
#27372=ADVANCED_FACE('',(#3464),#26345,.T.);
#27373=ADVANCED_FACE('',(#3465),#26346,.T.);
#27374=ADVANCED_FACE('',(#3466),#26347,.T.);
#27375=ADVANCED_FACE('',(#3467),#26348,.T.);
#27376=ADVANCED_FACE('',(#3468),#26349,.T.);
#27377=ADVANCED_FACE('',(#3469),#26350,.T.);
#27378=ADVANCED_FACE('',(#3470),#26351,.T.);
#27379=ADVANCED_FACE('',(#3471),#26352,.T.);
#27380=ADVANCED_FACE('',(#3472,#1912),#26353,.T.);
#27381=ADVANCED_FACE('',(#3473),#26354,.T.);
#27382=ADVANCED_FACE('',(#3474),#26355,.T.);
#27383=ADVANCED_FACE('',(#3475),#26356,.T.);
#27384=ADVANCED_FACE('',(#3476),#26357,.T.);
#27385=ADVANCED_FACE('',(#3477,#1913),#26358,.T.);
#27386=ADVANCED_FACE('',(#3478),#26359,.T.);
#27387=ADVANCED_FACE('',(#3479),#2807,.F.);
#27388=ADVANCED_FACE('',(#3480),#26360,.T.);
#27389=ADVANCED_FACE('',(#3481),#2808,.F.);
#27390=ADVANCED_FACE('',(#3482),#1569,.F.);
#27391=ADVANCED_FACE('',(#3483),#26361,.F.);
#27392=ADVANCED_FACE('',(#3484),#26362,.T.);
#27393=ADVANCED_FACE('',(#3485),#2809,.F.);
#27394=ADVANCED_FACE('',(#3486),#26363,.T.);
#27395=ADVANCED_FACE('',(#3487),#2810,.F.);
#27396=ADVANCED_FACE('',(#3488),#1570,.F.);
#27397=ADVANCED_FACE('',(#3489),#26364,.T.);
#27398=ADVANCED_FACE('',(#3490),#2811,.F.);
#27399=ADVANCED_FACE('',(#3491),#26365,.T.);
#27400=ADVANCED_FACE('',(#3492),#2812,.F.);
#27401=ADVANCED_FACE('',(#3493),#1571,.F.);
#27402=ADVANCED_FACE('',(#3494),#26366,.F.);
#27403=ADVANCED_FACE('',(#3495),#26367,.T.);
#27404=ADVANCED_FACE('',(#3496),#2813,.F.);
#27405=ADVANCED_FACE('',(#3497),#26368,.T.);
#27406=ADVANCED_FACE('',(#3498),#2814,.F.);
#27407=ADVANCED_FACE('',(#3499),#1572,.F.);
#27408=ADVANCED_FACE('',(#3500),#26369,.F.);
#27409=ADVANCED_FACE('',(#3501),#26370,.F.);
#27410=ADVANCED_FACE('',(#3502),#26371,.T.);
#27411=ADVANCED_FACE('',(#3503),#26372,.T.);
#27412=ADVANCED_FACE('',(#3504),#26373,.T.);
#27413=ADVANCED_FACE('',(#3505),#26374,.T.);
#27414=ADVANCED_FACE('',(#3506),#26375,.T.);
#27415=ADVANCED_FACE('',(#3507),#26376,.T.);
#27416=ADVANCED_FACE('',(#3508),#26377,.T.);
#27417=ADVANCED_FACE('',(#3509),#26378,.T.);
#27418=ADVANCED_FACE('',(#3510),#26379,.T.);
#27419=ADVANCED_FACE('',(#3511),#26380,.T.);
#27420=ADVANCED_FACE('',(#3512),#26381,.T.);
#27421=ADVANCED_FACE('',(#3513),#26382,.T.);
#27422=ADVANCED_FACE('',(#3514,#1914,#1915),#26383,.T.);
#27423=ADVANCED_FACE('',(#3515),#26384,.T.);
#27424=ADVANCED_FACE('',(#3516),#26385,.T.);
#27425=ADVANCED_FACE('',(#3517,#1916,#1917),#26386,.T.);
#27426=ADVANCED_FACE('',(#3518),#26387,.T.);
#27427=ADVANCED_FACE('',(#3519),#26388,.T.);
#27428=ADVANCED_FACE('',(#3520),#26389,.T.);
#27429=ADVANCED_FACE('',(#3521),#2815,.F.);
#27430=ADVANCED_FACE('',(#3522),#1573,.F.);
#27431=ADVANCED_FACE('',(#3523),#2816,.F.);
#27432=ADVANCED_FACE('',(#3524),#2817,.F.);
#27433=ADVANCED_FACE('',(#3525),#1574,.F.);
#27434=ADVANCED_FACE('',(#3526),#2818,.F.);
#27435=ADVANCED_FACE('',(#3527),#26390,.T.);
#27436=ADVANCED_FACE('',(#3528),#26391,.T.);
#27437=ADVANCED_FACE('',(#3529),#26392,.T.);
#27438=ADVANCED_FACE('',(#3530),#26393,.T.);
#27439=ADVANCED_FACE('',(#3531),#26394,.T.);
#27440=ADVANCED_FACE('',(#3532),#26395,.T.);
#27441=ADVANCED_FACE('',(#3533),#26396,.T.);
#27442=ADVANCED_FACE('',(#3534),#26397,.T.);
#27443=ADVANCED_FACE('',(#3535),#26398,.F.);
#27444=ADVANCED_FACE('',(#3536),#26399,.T.);
#27445=ADVANCED_FACE('',(#3537),#2819,.T.);
#27446=ADVANCED_FACE('',(#3538),#26400,.T.);
#27447=ADVANCED_FACE('',(#3539),#2820,.T.);
#27448=ADVANCED_FACE('',(#3540),#26401,.T.);
#27449=ADVANCED_FACE('',(#3541),#2821,.T.);
#27450=ADVANCED_FACE('',(#3542),#26402,.T.);
#27451=ADVANCED_FACE('',(#3543),#2822,.T.);
#27452=ADVANCED_FACE('',(#3544),#26403,.T.);
#27453=ADVANCED_FACE('',(#3545),#26404,.T.);
#27454=ADVANCED_FACE('',(#3546),#2823,.T.);
#27455=ADVANCED_FACE('',(#3547),#26405,.T.);
#27456=ADVANCED_FACE('',(#3548),#2824,.T.);
#27457=ADVANCED_FACE('',(#3549,#1918,#1919,#1920),#26406,.T.);
#27458=ADVANCED_FACE('',(#3550),#26407,.T.);
#27459=ADVANCED_FACE('',(#3551),#1575,.F.);
#27460=ADVANCED_FACE('',(#3552),#26408,.T.);
#27461=ADVANCED_FACE('',(#3553),#26409,.T.);
#27462=ADVANCED_FACE('',(#3554),#2825,.T.);
#27463=ADVANCED_FACE('',(#3555),#26410,.T.);
#27464=ADVANCED_FACE('',(#3556),#2826,.T.);
#27465=ADVANCED_FACE('',(#3557),#26411,.T.);
#27466=ADVANCED_FACE('',(#3558),#2827,.T.);
#27467=ADVANCED_FACE('',(#3559),#26412,.T.);
#27468=ADVANCED_FACE('',(#3560),#2828,.T.);
#27469=ADVANCED_FACE('',(#3561),#1576,.T.);
#27470=ADVANCED_FACE('',(#3562),#26413,.T.);
#27471=ADVANCED_FACE('',(#3563),#1577,.T.);
#27472=ADVANCED_FACE('',(#3564,#1921),#26414,.T.);
#27473=ADVANCED_FACE('',(#3565),#2829,.T.);
#27474=ADVANCED_FACE('',(#3566),#26415,.T.);
#27475=ADVANCED_FACE('',(#3567),#26416,.T.);
#27476=ADVANCED_FACE('',(#3568),#2830,.T.);
#27477=ADVANCED_FACE('',(#3569),#26417,.T.);
#27478=ADVANCED_FACE('',(#3570),#2831,.T.);
#27479=ADVANCED_FACE('',(#3571),#26418,.T.);
#27480=ADVANCED_FACE('',(#3572),#26419,.F.);
#27481=ADVANCED_FACE('',(#3573),#26420,.T.);
#27482=ADVANCED_FACE('',(#3574),#26421,.T.);
#27483=ADVANCED_FACE('',(#3575),#2832,.T.);
#27484=ADVANCED_FACE('',(#3576),#26422,.T.);
#27485=ADVANCED_FACE('',(#3577),#2833,.T.);
#27486=ADVANCED_FACE('',(#3578),#26423,.T.);
#27487=ADVANCED_FACE('',(#3579,#1922),#26424,.T.);
#27488=ADVANCED_FACE('',(#3580),#26425,.T.);
#27489=ADVANCED_FACE('',(#3581),#2834,.T.);
#27490=ADVANCED_FACE('',(#3582),#26426,.T.);
#27491=ADVANCED_FACE('',(#3583),#2835,.T.);
#27492=ADVANCED_FACE('',(#3584),#26427,.T.);
#27493=ADVANCED_FACE('',(#3585,#1923),#26428,.T.);
#27494=ADVANCED_FACE('',(#3586),#26429,.T.);
#27495=ADVANCED_FACE('',(#3587),#2836,.T.);
#27496=ADVANCED_FACE('',(#3588),#26430,.T.);
#27497=ADVANCED_FACE('',(#3589),#2837,.T.);
#27498=ADVANCED_FACE('',(#3590),#26431,.T.);
#27499=ADVANCED_FACE('',(#3591),#26432,.T.);
#27500=ADVANCED_FACE('',(#3592),#1578,.T.);
#27501=ADVANCED_FACE('',(#3593),#26433,.T.);
#27502=ADVANCED_FACE('',(#3594),#1579,.T.);
#27503=ADVANCED_FACE('',(#3595),#26434,.T.);
#27504=ADVANCED_FACE('',(#3596),#26435,.F.);
#27505=ADVANCED_FACE('',(#3597),#2838,.T.);
#27506=ADVANCED_FACE('',(#3598,#1924),#26436,.T.);
#27507=ADVANCED_FACE('',(#3599),#1580,.T.);
#27508=ADVANCED_FACE('',(#3600),#2839,.F.);
#27509=ADVANCED_FACE('',(#3601),#1581,.F.);
#27510=ADVANCED_FACE('',(#3602),#2840,.F.);
#27511=ADVANCED_FACE('',(#3603),#1582,.F.);
#27512=ADVANCED_FACE('',(#3604),#2841,.F.);
#27513=ADVANCED_FACE('',(#3605),#2842,.F.);
#27514=ADVANCED_FACE('',(#3606),#1583,.T.);
#27515=ADVANCED_FACE('',(#3607),#1584,.T.);
#27516=ADVANCED_FACE('',(#3608),#26437,.T.);
#27517=ADVANCED_FACE('',(#3609),#1585,.T.);
#27518=ADVANCED_FACE('',(#3610),#26438,.F.);
#27519=ADVANCED_FACE('',(#3611),#26439,.T.);
#27520=ADVANCED_FACE('',(#3612),#26440,.T.);
#27521=ADVANCED_FACE('',(#3613),#26441,.T.);
#27522=ADVANCED_FACE('',(#3614),#26442,.F.);
#27523=ADVANCED_FACE('',(#3615),#26443,.T.);
#27524=ADVANCED_FACE('',(#3616),#26444,.T.);
#27525=ADVANCED_FACE('',(#3617),#26445,.T.);
#27526=ADVANCED_FACE('',(#3618),#2843,.T.);
#27527=ADVANCED_FACE('',(#3619),#1586,.T.);
#27528=ADVANCED_FACE('',(#3620),#2844,.F.);
#27529=ADVANCED_FACE('',(#3621),#1587,.F.);
#27530=ADVANCED_FACE('',(#3622,#1925),#26446,.T.);
#27531=ADVANCED_FACE('',(#3623),#26447,.F.);
#27532=ADVANCED_FACE('',(#3624),#26448,.F.);
#27533=ADVANCED_FACE('',(#3625),#26449,.F.);
#27534=ADVANCED_FACE('',(#3626),#376,.F.);
#27535=ADVANCED_FACE('',(#3627,#1926),#1588,.T.);
#27536=ADVANCED_FACE('',(#3628,#1927),#26450,.T.);
#27537=ADVANCED_FACE('',(#3629),#2845,.T.);
#27538=ADVANCED_FACE('',(#3630),#1589,.T.);
#27539=ADVANCED_FACE('',(#3631),#2846,.T.);
#27540=ADVANCED_FACE('',(#3632),#26451,.T.);
#27541=ADVANCED_FACE('',(#3633),#2847,.T.);
#27542=ADVANCED_FACE('',(#3634),#26452,.T.);
#27543=ADVANCED_FACE('',(#3635),#2848,.T.);
#27544=ADVANCED_FACE('',(#3636),#26453,.T.);
#27545=ADVANCED_FACE('',(#3637),#2849,.T.);
#27546=ADVANCED_FACE('',(#3638),#26454,.T.);
#27547=ADVANCED_FACE('',(#3639),#2850,.T.);
#27548=ADVANCED_FACE('',(#3640),#1590,.T.);
#27549=ADVANCED_FACE('',(#3641),#26455,.F.);
#27550=ADVANCED_FACE('',(#3642),#26456,.T.);
#27551=ADVANCED_FACE('',(#3643),#2851,.T.);
#27552=ADVANCED_FACE('',(#3644),#26457,.T.);
#27553=ADVANCED_FACE('',(#3645),#1591,.T.);
#27554=ADVANCED_FACE('',(#3646),#26458,.T.);
#27555=ADVANCED_FACE('',(#3647),#1592,.T.);
#27556=ADVANCED_FACE('',(#3648),#1593,.T.);
#27557=ADVANCED_FACE('',(#3649),#1594,.T.);
#27558=ADVANCED_FACE('',(#3650),#1595,.T.);
#27559=ADVANCED_FACE('',(#3651),#1596,.T.);
#27560=ADVANCED_FACE('',(#3652),#1597,.T.);
#27561=ADVANCED_FACE('',(#3653),#1598,.T.);
#27562=ADVANCED_FACE('',(#3654),#1599,.T.);
#27563=ADVANCED_FACE('',(#3655),#1600,.T.);
#27564=ADVANCED_FACE('',(#3656),#26459,.F.);
#27565=ADVANCED_FACE('',(#3657),#26460,.F.);
#27566=ADVANCED_FACE('',(#3658),#26461,.F.);
#27567=ADVANCED_FACE('',(#3659),#26462,.F.);
#27568=ADVANCED_FACE('',(#3660),#26463,.F.);
#27569=ADVANCED_FACE('',(#3661),#26464,.F.);
#27570=ADVANCED_FACE('',(#3662),#26465,.F.);
#27571=ADVANCED_FACE('',(#3663),#26466,.F.);
#27572=ADVANCED_FACE('',(#3664),#26467,.F.);
#27573=ADVANCED_FACE('',(#3665),#26468,.F.);
#27574=ADVANCED_FACE('',(#3666),#26469,.F.);
#27575=ADVANCED_FACE('',(#3667),#26470,.F.);
#27576=ADVANCED_FACE('',(#3668),#26471,.F.);
#27577=ADVANCED_FACE('',(#3669),#26472,.F.);
#27578=ADVANCED_FACE('',(#3670),#26473,.F.);
#27579=ADVANCED_FACE('',(#3671),#26474,.F.);
#27580=ADVANCED_FACE('',(#3672),#26475,.F.);
#27581=ADVANCED_FACE('',(#3673),#26476,.F.);
#27582=ADVANCED_FACE('',(#3674),#26477,.F.);
#27583=ADVANCED_FACE('',(#3675),#26478,.F.);
#27584=ADVANCED_FACE('',(#3676),#26479,.F.);
#27585=ADVANCED_FACE('',(#3677),#26480,.F.);
#27586=ADVANCED_FACE('',(#3678),#26481,.F.);
#27587=ADVANCED_FACE('',(#3679),#26482,.F.);
#27588=ADVANCED_FACE('',(#3680),#26483,.F.);
#27589=ADVANCED_FACE('',(#3681),#26484,.F.);
#27590=ADVANCED_FACE('',(#3682),#26485,.F.);
#27591=ADVANCED_FACE('',(#3683),#26486,.F.);
#27592=ADVANCED_FACE('',(#3684),#26487,.F.);
#27593=ADVANCED_FACE('',(#3685),#26488,.F.);
#27594=ADVANCED_FACE('',(#3686),#26489,.F.);
#27595=ADVANCED_FACE('',(#3687),#26490,.F.);
#27596=ADVANCED_FACE('',(#3688),#26491,.F.);
#27597=ADVANCED_FACE('',(#3689),#26492,.F.);
#27598=ADVANCED_FACE('',(#3690),#26493,.F.);
#27599=ADVANCED_FACE('',(#3691),#26494,.F.);
#27600=ADVANCED_FACE('',(#3692),#26495,.F.);
#27601=ADVANCED_FACE('',(#3693),#26496,.F.);
#27602=ADVANCED_FACE('',(#3694),#26497,.F.);
#27603=ADVANCED_FACE('',(#3695),#26498,.F.);
#27604=ADVANCED_FACE('',(#3696),#26499,.F.);
#27605=ADVANCED_FACE('',(#3697),#26500,.F.);
#27606=ADVANCED_FACE('',(#3698),#26501,.F.);
#27607=ADVANCED_FACE('',(#3699),#26502,.F.);
#27608=ADVANCED_FACE('',(#3700),#26503,.F.);
#27609=ADVANCED_FACE('',(#3701),#26504,.F.);
#27610=ADVANCED_FACE('',(#3702),#26505,.F.);
#27611=ADVANCED_FACE('',(#3703),#26506,.F.);
#27612=ADVANCED_FACE('',(#3704),#26507,.F.);
#27613=ADVANCED_FACE('',(#3705),#26508,.F.);
#27614=ADVANCED_FACE('',(#3706),#26509,.F.);
#27615=ADVANCED_FACE('',(#3707),#26510,.F.);
#27616=ADVANCED_FACE('',(#3708),#26511,.F.);
#27617=ADVANCED_FACE('',(#3709),#26512,.F.);
#27618=ADVANCED_FACE('',(#3710),#26513,.F.);
#27619=ADVANCED_FACE('',(#3711),#26514,.F.);
#27620=ADVANCED_FACE('',(#3712),#26515,.F.);
#27621=ADVANCED_FACE('',(#3713),#26516,.F.);
#27622=ADVANCED_FACE('',(#3714),#26517,.F.);
#27623=ADVANCED_FACE('',(#3715),#26518,.F.);
#27624=ADVANCED_FACE('',(#3716),#26519,.F.);
#27625=ADVANCED_FACE('',(#3717),#26520,.F.);
#27626=ADVANCED_FACE('',(#3718),#26521,.F.);
#27627=ADVANCED_FACE('',(#3719),#26522,.F.);
#27628=ADVANCED_FACE('',(#3720),#26523,.F.);
#27629=ADVANCED_FACE('',(#3721),#26524,.F.);
#27630=ADVANCED_FACE('',(#3722),#26525,.F.);
#27631=ADVANCED_FACE('',(#3723),#26526,.F.);
#27632=ADVANCED_FACE('',(#3724),#26527,.F.);
#27633=ADVANCED_FACE('',(#3725),#26528,.F.);
#27634=ADVANCED_FACE('',(#3726),#26529,.F.);
#27635=ADVANCED_FACE('',(#3727),#26530,.F.);
#27636=ADVANCED_FACE('',(#3728),#2852,.T.);
#27637=ADVANCED_FACE('',(#3729),#1601,.T.);
#27638=ADVANCED_FACE('',(#3730),#1602,.T.);
#27639=ADVANCED_FACE('',(#3731),#1603,.T.);
#27640=ADVANCED_FACE('',(#3732),#1604,.T.);
#27641=ADVANCED_FACE('',(#3733),#1605,.T.);
#27642=ADVANCED_FACE('',(#3734),#1606,.T.);
#27643=ADVANCED_FACE('',(#3735),#1607,.T.);
#27644=ADVANCED_FACE('',(#3736),#1608,.T.);
#27645=ADVANCED_FACE('',(#3737),#1609,.T.);
#27646=ADVANCED_FACE('',(#3738),#1610,.T.);
#27647=ADVANCED_FACE('',(#3739),#1611,.T.);
#27648=ADVANCED_FACE('',(#3740),#1612,.T.);
#27649=ADVANCED_FACE('',(#3741),#1613,.T.);
#27650=ADVANCED_FACE('',(#3742),#1614,.T.);
#27651=ADVANCED_FACE('',(#3743),#1615,.T.);
#27652=ADVANCED_FACE('',(#3744),#1616,.T.);
#27653=ADVANCED_FACE('',(#3745),#1617,.T.);
#27654=ADVANCED_FACE('',(#3746),#1618,.T.);
#27655=ADVANCED_FACE('',(#3747),#1619,.T.);
#27656=ADVANCED_FACE('',(#3748),#1620,.T.);
#27657=ADVANCED_FACE('',(#3749),#1621,.T.);
#27658=ADVANCED_FACE('',(#3750),#1622,.T.);
#27659=ADVANCED_FACE('',(#3751),#1623,.T.);
#27660=ADVANCED_FACE('',(#3752),#1454,.F.);
#27661=ADVANCED_FACE('',(#3753),#1624,.T.);
#27662=ADVANCED_FACE('',(#3754),#1455,.F.);
#27663=ADVANCED_FACE('',(#3755),#1625,.T.);
#27664=ADVANCED_FACE('',(#3756),#26531,.T.);
#27665=ADVANCED_FACE('',(#3757),#2853,.T.);
#27666=ADVANCED_FACE('',(#3758),#1626,.T.);
#27667=ADVANCED_FACE('',(#3759),#2854,.T.);
#27668=ADVANCED_FACE('',(#3760,#1928),#26532,.T.);
#27669=ADVANCED_FACE('',(#3761,#1929),#26533,.T.);
#27670=ADVANCED_FACE('',(#3762),#2855,.T.);
#27671=ADVANCED_FACE('',(#3763),#1627,.T.);
#27672=ADVANCED_FACE('',(#3764),#26534,.T.);
#27673=ADVANCED_FACE('',(#3765),#1628,.T.);
#27674=ADVANCED_FACE('',(#3766),#1629,.T.);
#27675=ADVANCED_FACE('',(#3767),#1630,.T.);
#27676=ADVANCED_FACE('',(#3768),#1631,.T.);
#27677=ADVANCED_FACE('',(#3769),#1632,.T.);
#27678=ADVANCED_FACE('',(#3770),#1633,.T.);
#27679=ADVANCED_FACE('',(#3771),#1634,.T.);
#27680=ADVANCED_FACE('',(#3772),#1635,.T.);
#27681=ADVANCED_FACE('',(#3773),#1636,.T.);
#27682=ADVANCED_FACE('',(#3774),#1637,.T.);
#27683=ADVANCED_FACE('',(#3775),#1638,.T.);
#27684=ADVANCED_FACE('',(#3776),#1639,.T.);
#27685=ADVANCED_FACE('',(#3777),#1640,.T.);
#27686=ADVANCED_FACE('',(#3778),#1641,.T.);
#27687=ADVANCED_FACE('',(#3779),#1642,.T.);
#27688=ADVANCED_FACE('',(#3780),#1643,.T.);
#27689=ADVANCED_FACE('',(#3781),#1644,.T.);
#27690=ADVANCED_FACE('',(#3782),#1645,.T.);
#27691=ADVANCED_FACE('',(#3783),#1646,.T.);
#27692=ADVANCED_FACE('',(#3784),#1647,.T.);
#27693=ADVANCED_FACE('',(#3785),#1648,.T.);
#27694=ADVANCED_FACE('',(#3786),#1649,.T.);
#27695=ADVANCED_FACE('',(#3787),#1650,.T.);
#27696=ADVANCED_FACE('',(#3788),#1651,.T.);
#27697=ADVANCED_FACE('',(#3789),#1652,.T.);
#27698=ADVANCED_FACE('',(#3790),#1653,.T.);
#27699=ADVANCED_FACE('',(#3791),#1654,.T.);
#27700=ADVANCED_FACE('',(#3792),#1655,.T.);
#27701=ADVANCED_FACE('',(#3793),#1656,.T.);
#27702=ADVANCED_FACE('',(#3794),#1657,.T.);
#27703=ADVANCED_FACE('',(#3795),#26535,.F.);
#27704=ADVANCED_FACE('',(#3796),#26536,.F.);
#27705=ADVANCED_FACE('',(#3797),#26537,.F.);
#27706=ADVANCED_FACE('',(#3798),#26538,.F.);
#27707=ADVANCED_FACE('',(#3799),#26539,.F.);
#27708=ADVANCED_FACE('',(#3800),#26540,.F.);
#27709=ADVANCED_FACE('',(#3801),#26541,.F.);
#27710=ADVANCED_FACE('',(#3802),#26542,.F.);
#27711=ADVANCED_FACE('',(#3803),#26543,.F.);
#27712=ADVANCED_FACE('',(#3804),#26544,.F.);
#27713=ADVANCED_FACE('',(#3805),#26545,.F.);
#27714=ADVANCED_FACE('',(#3806),#26546,.F.);
#27715=ADVANCED_FACE('',(#3807),#26547,.F.);
#27716=ADVANCED_FACE('',(#3808),#26548,.F.);
#27717=ADVANCED_FACE('',(#3809),#26549,.F.);
#27718=ADVANCED_FACE('',(#3810),#26550,.F.);
#27719=ADVANCED_FACE('',(#3811),#26551,.F.);
#27720=ADVANCED_FACE('',(#3812),#26552,.F.);
#27721=ADVANCED_FACE('',(#3813),#26553,.F.);
#27722=ADVANCED_FACE('',(#3814),#26554,.F.);
#27723=ADVANCED_FACE('',(#3815),#26555,.F.);
#27724=ADVANCED_FACE('',(#3816),#26556,.F.);
#27725=ADVANCED_FACE('',(#3817),#26557,.F.);
#27726=ADVANCED_FACE('',(#3818),#26558,.F.);
#27727=ADVANCED_FACE('',(#3819),#26559,.F.);
#27728=ADVANCED_FACE('',(#3820),#26560,.F.);
#27729=ADVANCED_FACE('',(#3821),#26561,.F.);
#27730=ADVANCED_FACE('',(#3822),#26562,.F.);
#27731=ADVANCED_FACE('',(#3823),#26563,.F.);
#27732=ADVANCED_FACE('',(#3824),#26564,.F.);
#27733=ADVANCED_FACE('',(#3825),#26565,.F.);
#27734=ADVANCED_FACE('',(#3826),#26566,.F.);
#27735=ADVANCED_FACE('',(#3827),#26567,.F.);
#27736=ADVANCED_FACE('',(#3828),#26568,.F.);
#27737=ADVANCED_FACE('',(#3829),#26569,.F.);
#27738=ADVANCED_FACE('',(#3830),#26570,.F.);
#27739=ADVANCED_FACE('',(#3831),#26571,.F.);
#27740=ADVANCED_FACE('',(#3832),#26572,.F.);
#27741=ADVANCED_FACE('',(#3833),#26573,.F.);
#27742=ADVANCED_FACE('',(#3834),#26574,.F.);
#27743=ADVANCED_FACE('',(#3835),#26575,.F.);
#27744=ADVANCED_FACE('',(#3836),#26576,.F.);
#27745=ADVANCED_FACE('',(#3837),#26577,.F.);
#27746=ADVANCED_FACE('',(#3838),#26578,.F.);
#27747=ADVANCED_FACE('',(#3839),#26579,.F.);
#27748=ADVANCED_FACE('',(#3840),#26580,.F.);
#27749=ADVANCED_FACE('',(#3841),#26581,.F.);
#27750=ADVANCED_FACE('',(#3842),#26582,.F.);
#27751=ADVANCED_FACE('',(#3843),#26583,.F.);
#27752=ADVANCED_FACE('',(#3844),#26584,.F.);
#27753=ADVANCED_FACE('',(#3845),#26585,.F.);
#27754=ADVANCED_FACE('',(#3846),#26586,.F.);
#27755=ADVANCED_FACE('',(#3847),#26587,.F.);
#27756=ADVANCED_FACE('',(#3848),#26588,.F.);
#27757=ADVANCED_FACE('',(#3849),#1658,.T.);
#27758=ADVANCED_FACE('',(#3850),#1456,.F.);
#27759=ADVANCED_FACE('',(#3851),#26589,.F.);
#27760=ADVANCED_FACE('',(#3852),#1659,.T.);
#27761=ADVANCED_FACE('',(#3853),#1457,.F.);
#27762=ADVANCED_FACE('',(#3854),#26590,.T.);
#27763=ADVANCED_FACE('',(#3855),#2856,.T.);
#27764=ADVANCED_FACE('',(#3856),#1660,.T.);
#27765=ADVANCED_FACE('',(#3857,#1930),#26591,.T.);
#27766=ADVANCED_FACE('',(#3858),#2857,.T.);
#27767=ADVANCED_FACE('',(#3859),#2858,.T.);
#27768=ADVANCED_FACE('',(#3860),#26592,.T.);
#27769=ADVANCED_FACE('',(#3861),#1661,.T.);
#27770=ADVANCED_FACE('',(#3862),#26593,.F.);
#27771=ADVANCED_FACE('',(#3863,#1931),#26594,.T.);
#27772=ADVANCED_FACE('',(#3864),#26595,.T.);
#27773=ADVANCED_FACE('',(#3865),#26596,.T.);
#27774=ADVANCED_FACE('',(#3866),#26597,.T.);
#27775=ADVANCED_FACE('',(#3867),#26598,.T.);
#27776=ADVANCED_FACE('',(#3868),#26599,.T.);
#27777=ADVANCED_FACE('',(#3869),#26600,.T.);
#27778=ADVANCED_FACE('',(#3870,#1932),#26601,.F.);
#27779=ADVANCED_FACE('',(#3871),#26602,.T.);
#27780=ADVANCED_FACE('',(#3872),#26603,.T.);
#27781=ADVANCED_FACE('',(#3873),#1662,.T.);
#27782=ADVANCED_FACE('',(#3874),#1663,.T.);
#27783=ADVANCED_FACE('',(#3875),#26604,.T.);
#27784=ADVANCED_FACE('',(#3876),#26605,.T.);
#27785=ADVANCED_FACE('',(#3877),#26606,.T.);
#27786=ADVANCED_FACE('',(#3878),#1664,.T.);
#27787=ADVANCED_FACE('',(#3879),#26607,.T.);
#27788=ADVANCED_FACE('',(#3880),#26608,.T.);
#27789=ADVANCED_FACE('',(#3881),#26609,.F.);
#27790=ADVANCED_FACE('',(#3882),#26610,.F.);
#27791=ADVANCED_FACE('',(#3883),#26611,.F.);
#27792=ADVANCED_FACE('',(#3884),#26612,.F.);
#27793=ADVANCED_FACE('',(#3885),#26613,.F.);
#27794=ADVANCED_FACE('',(#3886),#26614,.F.);
#27795=ADVANCED_FACE('',(#3887),#26615,.F.);
#27796=ADVANCED_FACE('',(#3888),#26616,.F.);
#27797=ADVANCED_FACE('',(#3889),#26617,.F.);
#27798=ADVANCED_FACE('',(#3890),#26618,.F.);
#27799=ADVANCED_FACE('',(#3891),#26619,.F.);
#27800=ADVANCED_FACE('',(#3892),#26620,.F.);
#27801=ADVANCED_FACE('',(#3893),#26621,.F.);
#27802=ADVANCED_FACE('',(#3894),#26622,.F.);
#27803=ADVANCED_FACE('',(#3895),#26623,.F.);
#27804=ADVANCED_FACE('',(#3896),#26624,.F.);
#27805=ADVANCED_FACE('',(#3897),#26625,.F.);
#27806=ADVANCED_FACE('',(#3898),#26626,.F.);
#27807=ADVANCED_FACE('',(#3899),#26627,.F.);
#27808=ADVANCED_FACE('',(#3900),#26628,.F.);
#27809=ADVANCED_FACE('',(#3901),#26629,.F.);
#27810=ADVANCED_FACE('',(#3902),#26630,.F.);
#27811=ADVANCED_FACE('',(#3903),#26631,.F.);
#27812=ADVANCED_FACE('',(#3904),#26632,.F.);
#27813=ADVANCED_FACE('',(#3905),#26633,.F.);
#27814=ADVANCED_FACE('',(#3906),#26634,.F.);
#27815=ADVANCED_FACE('',(#3907),#26635,.F.);
#27816=ADVANCED_FACE('',(#3908),#26636,.F.);
#27817=ADVANCED_FACE('',(#3909),#26637,.F.);
#27818=ADVANCED_FACE('',(#3910),#26638,.F.);
#27819=ADVANCED_FACE('',(#3911),#26639,.F.);
#27820=ADVANCED_FACE('',(#3912),#26640,.F.);
#27821=ADVANCED_FACE('',(#3913),#26641,.F.);
#27822=ADVANCED_FACE('',(#3914),#26642,.F.);
#27823=ADVANCED_FACE('',(#3915),#26643,.F.);
#27824=ADVANCED_FACE('',(#3916),#26644,.F.);
#27825=ADVANCED_FACE('',(#3917),#26645,.F.);
#27826=ADVANCED_FACE('',(#3918),#26646,.F.);
#27827=ADVANCED_FACE('',(#3919),#26647,.F.);
#27828=ADVANCED_FACE('',(#3920),#26648,.F.);
#27829=ADVANCED_FACE('',(#3921),#26649,.F.);
#27830=ADVANCED_FACE('',(#3922),#26650,.F.);
#27831=ADVANCED_FACE('',(#3923),#26651,.F.);
#27832=ADVANCED_FACE('',(#3924),#26652,.F.);
#27833=ADVANCED_FACE('',(#3925),#26653,.F.);
#27834=ADVANCED_FACE('',(#3926),#26654,.F.);
#27835=ADVANCED_FACE('',(#3927),#26655,.F.);
#27836=ADVANCED_FACE('',(#3928),#26656,.F.);
#27837=ADVANCED_FACE('',(#3929),#26657,.F.);
#27838=ADVANCED_FACE('',(#3930),#26658,.F.);
#27839=ADVANCED_FACE('',(#3931),#26659,.F.);
#27840=ADVANCED_FACE('',(#3932),#26660,.F.);
#27841=ADVANCED_FACE('',(#3933),#26661,.F.);
#27842=ADVANCED_FACE('',(#3934),#26662,.F.);
#27843=ADVANCED_FACE('',(#3935),#26663,.F.);
#27844=ADVANCED_FACE('',(#3936),#26664,.F.);
#27845=ADVANCED_FACE('',(#3937,#1933,#1934,#1935,#1936,#1937,#1938,#1939,
#1940,#1941,#1942,#1943,#1944),#26665,.F.);
#27846=ADVANCED_FACE('',(#3938),#1665,.F.);
#27847=ADVANCED_FACE('',(#3939),#26666,.T.);
#27848=ADVANCED_FACE('',(#3940),#2859,.T.);
#27849=ADVANCED_FACE('',(#3941,#1945),#1666,.T.);
#27850=ADVANCED_FACE('',(#3942,#1946),#26667,.T.);
#27851=ADVANCED_FACE('',(#3943),#1667,.T.);
#27852=ADVANCED_FACE('',(#3944),#2860,.T.);
#27853=ADVANCED_FACE('',(#3945,#1947),#26668,.T.);
#27854=ADVANCED_FACE('',(#3946),#1458,.T.);
#27855=ADVANCED_FACE('',(#3947),#1668,.F.);
#27856=ADVANCED_FACE('',(#3948,#1948,#1949),#1669,.T.);
#27857=ADVANCED_FACE('',(#3949),#1459,.T.);
#27858=ADVANCED_FACE('',(#3950,#1950),#377,.T.);
#27859=ADVANCED_FACE('',(#3951),#1670,.T.);
#27860=ADVANCED_FACE('',(#3952),#26669,.T.);
#27861=ADVANCED_FACE('',(#3953),#2861,.T.);
#27862=ADVANCED_FACE('',(#3954,#1951),#26670,.T.);
#27863=ADVANCED_FACE('',(#3955),#2862,.T.);
#27864=ADVANCED_FACE('',(#3956),#1671,.T.);
#27865=ADVANCED_FACE('',(#3957),#2863,.T.);
#27866=ADVANCED_FACE('',(#3958,#1952),#26671,.T.);
#27867=ADVANCED_FACE('',(#3959),#2864,.T.);
#27868=ADVANCED_FACE('',(#3960),#26672,.T.);
#27869=ADVANCED_FACE('',(#3961),#1460,.T.);
#27870=ADVANCED_FACE('',(#3962),#26673,.T.);
#27871=ADVANCED_FACE('',(#3963),#26674,.F.);
#27872=ADVANCED_FACE('',(#3964),#26675,.T.);
#27873=ADVANCED_FACE('',(#3965),#26676,.T.);
#27874=ADVANCED_FACE('',(#3966),#26677,.T.);
#27875=ADVANCED_FACE('',(#3967),#26678,.T.);
#27876=ADVANCED_FACE('',(#3968),#26679,.T.);
#27877=ADVANCED_FACE('',(#3969),#26680,.T.);
#27878=ADVANCED_FACE('',(#3970),#26681,.T.);
#27879=ADVANCED_FACE('',(#3971),#26682,.T.);
#27880=ADVANCED_FACE('',(#3972),#26683,.T.);
#27881=ADVANCED_FACE('',(#3973),#26684,.T.);
#27882=ADVANCED_FACE('',(#3974),#26685,.T.);
#27883=ADVANCED_FACE('',(#3975),#26686,.T.);
#27884=ADVANCED_FACE('',(#3976),#26687,.T.);
#27885=ADVANCED_FACE('',(#3977),#26688,.T.);
#27886=ADVANCED_FACE('',(#3978),#26689,.T.);
#27887=ADVANCED_FACE('',(#3979),#26690,.T.);
#27888=ADVANCED_FACE('',(#3980),#26691,.T.);
#27889=ADVANCED_FACE('',(#3981),#26692,.T.);
#27890=ADVANCED_FACE('',(#3982),#26693,.T.);
#27891=ADVANCED_FACE('',(#3983),#26694,.T.);
#27892=ADVANCED_FACE('',(#3984),#26695,.T.);
#27893=ADVANCED_FACE('',(#3985),#26696,.T.);
#27894=ADVANCED_FACE('',(#3986),#26697,.T.);
#27895=ADVANCED_FACE('',(#3987),#26698,.T.);
#27896=ADVANCED_FACE('',(#3988),#26699,.T.);
#27897=ADVANCED_FACE('',(#3989),#26700,.T.);
#27898=ADVANCED_FACE('',(#3990),#26701,.T.);
#27899=ADVANCED_FACE('',(#3991),#26702,.T.);
#27900=ADVANCED_FACE('',(#3992),#26703,.T.);
#27901=ADVANCED_FACE('',(#3993),#26704,.T.);
#27902=ADVANCED_FACE('',(#3994),#26705,.T.);
#27903=ADVANCED_FACE('',(#3995),#26706,.T.);
#27904=ADVANCED_FACE('',(#3996),#26707,.T.);
#27905=ADVANCED_FACE('',(#3997),#26708,.T.);
#27906=ADVANCED_FACE('',(#3998),#2865,.T.);
#27907=ADVANCED_FACE('',(#3999),#26709,.T.);
#27908=ADVANCED_FACE('',(#4000),#2866,.T.);
#27909=ADVANCED_FACE('',(#4001),#26710,.T.);
#27910=ADVANCED_FACE('',(#4002),#2867,.T.);
#27911=ADVANCED_FACE('',(#4003),#26711,.T.);
#27912=ADVANCED_FACE('',(#4004),#2868,.T.);
#27913=ADVANCED_FACE('',(#4005),#26712,.T.);
#27914=ADVANCED_FACE('',(#4006),#26713,.T.);
#27915=ADVANCED_FACE('',(#4007),#1672,.T.);
#27916=ADVANCED_FACE('',(#4008),#26714,.T.);
#27917=ADVANCED_FACE('',(#4009),#1673,.T.);
#27918=ADVANCED_FACE('',(#4010,#1953,#1954),#26715,.F.);
#27919=ADVANCED_FACE('',(#4011),#26716,.T.);
#27920=ADVANCED_FACE('',(#4012),#26717,.T.);
#27921=ADVANCED_FACE('',(#4013),#26718,.T.);
#27922=ADVANCED_FACE('',(#4014),#26719,.T.);
#27923=ADVANCED_FACE('',(#4015,#1955,#1956),#26720,.T.);
#27924=ADVANCED_FACE('',(#4016),#26721,.T.);
#27925=ADVANCED_FACE('',(#4017),#26722,.T.);
#27926=ADVANCED_FACE('',(#4018),#26723,.T.);
#27927=ADVANCED_FACE('',(#4019),#26724,.T.);
#27928=ADVANCED_FACE('',(#4020,#1957,#1958),#26725,.T.);
#27929=ADVANCED_FACE('',(#4021),#26726,.T.);
#27930=ADVANCED_FACE('',(#4022),#26727,.T.);
#27931=ADVANCED_FACE('',(#4023),#26728,.T.);
#27932=ADVANCED_FACE('',(#4024),#2869,.F.);
#27933=ADVANCED_FACE('',(#4025),#1674,.F.);
#27934=ADVANCED_FACE('',(#4026,#1959,#1960),#26729,.T.);
#27935=ADVANCED_FACE('',(#4027),#2870,.F.);
#27936=ADVANCED_FACE('',(#4028),#2871,.F.);
#27937=ADVANCED_FACE('',(#4029),#1675,.F.);
#27938=ADVANCED_FACE('',(#4030),#2872,.F.);
#27939=ADVANCED_FACE('',(#4031,#1961,#1962),#26730,.T.);
#27940=ADVANCED_FACE('',(#4032),#2873,.F.);
#27941=ADVANCED_FACE('',(#4033),#1676,.F.);
#27942=ADVANCED_FACE('',(#4034),#2874,.F.);
#27943=ADVANCED_FACE('',(#4035),#2875,.F.);
#27944=ADVANCED_FACE('',(#4036),#1677,.F.);
#27945=ADVANCED_FACE('',(#4037),#2876,.F.);
#27946=ADVANCED_FACE('',(#4038),#2877,.F.);
#27947=ADVANCED_FACE('',(#4039),#1678,.F.);
#27948=ADVANCED_FACE('',(#4040),#2878,.F.);
#27949=ADVANCED_FACE('',(#4041),#1679,.F.);
#27950=ADVANCED_FACE('',(#4042),#26731,.T.);
#27951=ADVANCED_FACE('',(#4043),#2879,.T.);
#27952=ADVANCED_FACE('',(#4044),#26732,.T.);
#27953=ADVANCED_FACE('',(#4045),#2880,.T.);
#27954=ADVANCED_FACE('',(#4046),#26733,.T.);
#27955=ADVANCED_FACE('',(#4047,#1963,#1964,#1965,#1966),#26734,.T.);
#27956=ADVANCED_FACE('',(#4048),#26735,.T.);
#27957=ADVANCED_FACE('',(#4049),#2881,.T.);
#27958=ADVANCED_FACE('',(#4050),#26736,.T.);
#27959=ADVANCED_FACE('',(#4051),#2882,.T.);
#27960=ADVANCED_FACE('',(#4052),#26737,.T.);
#27961=ADVANCED_FACE('',(#4053),#2883,.F.);
#27962=ADVANCED_FACE('',(#4054),#2884,.F.);
#27963=ADVANCED_FACE('',(#4055),#26738,.T.);
#27964=ADVANCED_FACE('',(#4056),#26739,.T.);
#27965=ADVANCED_FACE('',(#4057),#26740,.T.);
#27966=ADVANCED_FACE('',(#4058),#2885,.T.);
#27967=ADVANCED_FACE('',(#4059),#26741,.T.);
#27968=ADVANCED_FACE('',(#4060),#2886,.T.);
#27969=ADVANCED_FACE('',(#4061),#26742,.T.);
#27970=ADVANCED_FACE('',(#4062),#2887,.T.);
#27971=ADVANCED_FACE('',(#4063),#26743,.T.);
#27972=ADVANCED_FACE('',(#4064),#2888,.T.);
#27973=ADVANCED_FACE('',(#4065),#26744,.T.);
#27974=ADVANCED_FACE('',(#4066),#26745,.T.);
#27975=ADVANCED_FACE('',(#4067),#1680,.T.);
#27976=ADVANCED_FACE('',(#4068),#26746,.T.);
#27977=ADVANCED_FACE('',(#4069),#1681,.T.);
#27978=ADVANCED_FACE('',(#4070,#1967,#1968,#1969),#378,.T.);
#27979=ADVANCED_FACE('',(#4071),#26747,.T.);
#27980=ADVANCED_FACE('',(#4072),#1682,.T.);
#27981=ADVANCED_FACE('',(#4073),#26748,.F.);
#27982=ADVANCED_FACE('',(#4074),#26749,.F.);
#27983=ADVANCED_FACE('',(#4075,#1970,#1971),#379,.T.);
#27984=ADVANCED_FACE('',(#4076),#26750,.T.);
#27985=ADVANCED_FACE('',(#4077),#26751,.F.);
#27986=ADVANCED_FACE('',(#4078),#1683,.T.);
#27987=ADVANCED_FACE('',(#4079,#1972,#1973),#1461,.T.);
#27988=ADVANCED_FACE('',(#4080),#1684,.T.);
#27989=ADVANCED_FACE('',(#4081),#1685,.T.);
#27990=ADVANCED_FACE('',(#4082),#1686,.T.);
#27991=ADVANCED_FACE('',(#4083),#1687,.T.);
#27992=ADVANCED_FACE('',(#4084),#1688,.T.);
#27993=ADVANCED_FACE('',(#4085),#1689,.T.);
#27994=ADVANCED_FACE('',(#4086),#1690,.T.);
#27995=ADVANCED_FACE('',(#4087),#1691,.T.);
#27996=ADVANCED_FACE('',(#4088),#1692,.T.);
#27997=ADVANCED_FACE('',(#4089),#1693,.T.);
#27998=ADVANCED_FACE('',(#4090),#1694,.T.);
#27999=ADVANCED_FACE('',(#4091),#1695,.T.);
#28000=ADVANCED_FACE('',(#4092),#1696,.T.);
#28001=ADVANCED_FACE('',(#4093),#1697,.T.);
#28002=ADVANCED_FACE('',(#4094),#1698,.T.);
#28003=ADVANCED_FACE('',(#4095),#1699,.T.);
#28004=ADVANCED_FACE('',(#4096),#1700,.T.);
#28005=ADVANCED_FACE('',(#4097),#1701,.T.);
#28006=ADVANCED_FACE('',(#4098),#1702,.T.);
#28007=ADVANCED_FACE('',(#4099),#1703,.T.);
#28008=ADVANCED_FACE('',(#4100),#1704,.T.);
#28009=ADVANCED_FACE('',(#4101),#1705,.T.);
#28010=ADVANCED_FACE('',(#4102),#380,.T.);
#28011=ADVANCED_FACE('',(#4103,#1974),#26752,.T.);
#28012=ADVANCED_FACE('',(#4104),#26753,.T.);
#28013=ADVANCED_FACE('',(#4105),#2889,.T.);
#28014=ADVANCED_FACE('',(#4106),#2890,.T.);
#28015=ADVANCED_FACE('',(#4107),#26754,.T.);
#28016=ADVANCED_FACE('',(#4108,#1975),#26755,.T.);
#28017=ADVANCED_FACE('',(#4109),#1706,.T.);
#28018=ADVANCED_FACE('',(#4110),#2891,.T.);
#28019=ADVANCED_FACE('',(#4111),#1462,.F.);
#28020=ADVANCED_FACE('',(#4112),#1707,.T.);
#28021=ADVANCED_FACE('',(#4113),#1463,.F.);
#28022=ADVANCED_FACE('',(#4114),#26756,.T.);
#28023=ADVANCED_FACE('',(#4115),#26757,.T.);
#28024=ADVANCED_FACE('',(#4116),#2892,.T.);
#28025=ADVANCED_FACE('',(#4117),#1708,.T.);
#28026=ADVANCED_FACE('',(#4118),#26758,.T.);
#28027=ADVANCED_FACE('',(#4119),#26759,.T.);
#28028=ADVANCED_FACE('',(#4120),#26760,.T.);
#28029=ADVANCED_FACE('',(#4121),#26761,.T.);
#28030=ADVANCED_FACE('',(#4122),#26762,.T.);
#28031=ADVANCED_FACE('',(#4123),#26763,.T.);
#28032=ADVANCED_FACE('',(#4124),#26764,.T.);
#28033=ADVANCED_FACE('',(#4125),#26765,.T.);
#28034=ADVANCED_FACE('',(#4126),#26766,.T.);
#28035=ADVANCED_FACE('',(#4127),#26767,.T.);
#28036=ADVANCED_FACE('',(#4128),#26768,.T.);
#28037=ADVANCED_FACE('',(#4129),#26769,.T.);
#28038=ADVANCED_FACE('',(#4130),#26770,.T.);
#28039=ADVANCED_FACE('',(#4131),#26771,.T.);
#28040=ADVANCED_FACE('',(#4132),#26772,.T.);
#28041=ADVANCED_FACE('',(#4133),#26773,.T.);
#28042=ADVANCED_FACE('',(#4134),#26774,.T.);
#28043=ADVANCED_FACE('',(#4135),#26775,.T.);
#28044=ADVANCED_FACE('',(#4136),#26776,.T.);
#28045=ADVANCED_FACE('',(#4137),#26777,.T.);
#28046=ADVANCED_FACE('',(#4138),#26778,.T.);
#28047=ADVANCED_FACE('',(#4139),#26779,.T.);
#28048=ADVANCED_FACE('',(#4140),#26780,.T.);
#28049=ADVANCED_FACE('',(#4141),#26781,.T.);
#28050=ADVANCED_FACE('',(#4142),#26782,.T.);
#28051=ADVANCED_FACE('',(#4143),#26783,.T.);
#28052=ADVANCED_FACE('',(#4144),#26784,.T.);
#28053=ADVANCED_FACE('',(#4145),#26785,.T.);
#28054=ADVANCED_FACE('',(#4146),#26786,.T.);
#28055=ADVANCED_FACE('',(#4147),#26787,.T.);
#28056=ADVANCED_FACE('',(#4148),#26788,.T.);
#28057=ADVANCED_FACE('',(#4149),#26789,.T.);
#28058=ADVANCED_FACE('',(#4150),#26790,.T.);
#28059=ADVANCED_FACE('',(#4151),#26791,.T.);
#28060=ADVANCED_FACE('',(#4152),#26792,.T.);
#28061=ADVANCED_FACE('',(#4153),#26793,.T.);
#28062=ADVANCED_FACE('',(#4154),#26794,.T.);
#28063=ADVANCED_FACE('',(#4155),#26795,.T.);
#28064=ADVANCED_FACE('',(#4156),#26796,.T.);
#28065=ADVANCED_FACE('',(#4157),#26797,.F.);
#28066=ADVANCED_FACE('',(#4158),#26798,.F.);
#28067=ADVANCED_FACE('',(#4159),#26799,.F.);
#28068=ADVANCED_FACE('',(#4160),#26800,.T.);
#28069=ADVANCED_FACE('',(#4161),#26801,.T.);
#28070=ADVANCED_FACE('',(#4162),#26802,.T.);
#28071=ADVANCED_FACE('',(#4163),#1709,.T.);
#28072=ADVANCED_FACE('',(#4164),#1710,.T.);
#28073=ADVANCED_FACE('',(#4165),#1711,.T.);
#28074=ADVANCED_FACE('',(#4166),#1712,.T.);
#28075=ADVANCED_FACE('',(#4167),#1713,.T.);
#28076=ADVANCED_FACE('',(#4168),#1714,.T.);
#28077=ADVANCED_FACE('',(#4169),#1715,.T.);
#28078=ADVANCED_FACE('',(#4170),#1716,.T.);
#28079=ADVANCED_FACE('',(#4171),#1717,.T.);
#28080=ADVANCED_FACE('',(#4172),#1718,.T.);
#28081=ADVANCED_FACE('',(#4173),#1719,.T.);
#28082=ADVANCED_FACE('',(#4174),#1720,.T.);
#28083=ADVANCED_FACE('',(#4175),#1721,.T.);
#28084=ADVANCED_FACE('',(#4176),#1722,.T.);
#28085=ADVANCED_FACE('',(#4177),#1723,.T.);
#28086=ADVANCED_FACE('',(#4178),#1724,.T.);
#28087=ADVANCED_FACE('',(#4179),#1725,.T.);
#28088=ADVANCED_FACE('',(#4180),#1726,.T.);
#28089=ADVANCED_FACE('',(#4181),#1727,.T.);
#28090=ADVANCED_FACE('',(#4182),#1728,.T.);
#28091=ADVANCED_FACE('',(#4183),#1729,.T.);
#28092=ADVANCED_FACE('',(#4184),#1730,.T.);
#28093=ADVANCED_FACE('',(#4185),#1731,.T.);
#28094=ADVANCED_FACE('',(#4186),#1732,.T.);
#28095=ADVANCED_FACE('',(#4187),#1733,.T.);
#28096=ADVANCED_FACE('',(#4188),#1734,.T.);
#28097=ADVANCED_FACE('',(#4189),#1735,.T.);
#28098=ADVANCED_FACE('',(#4190),#1736,.T.);
#28099=ADVANCED_FACE('',(#4191),#1737,.T.);
#28100=ADVANCED_FACE('',(#4192),#1738,.T.);
#28101=ADVANCED_FACE('',(#4193),#1739,.T.);
#28102=ADVANCED_FACE('',(#4194),#1740,.T.);
#28103=ADVANCED_FACE('',(#4195),#1741,.T.);
#28104=ADVANCED_FACE('',(#4196),#1742,.T.);
#28105=ADVANCED_FACE('',(#4197),#1743,.T.);
#28106=ADVANCED_FACE('',(#4198),#1744,.T.);
#28107=ADVANCED_FACE('',(#4199),#1745,.T.);
#28108=ADVANCED_FACE('',(#4200),#1746,.T.);
#28109=ADVANCED_FACE('',(#4201),#1747,.T.);
#28110=ADVANCED_FACE('',(#4202),#1748,.T.);
#28111=ADVANCED_FACE('',(#4203),#1749,.T.);
#28112=ADVANCED_FACE('',(#4204),#1750,.T.);
#28113=ADVANCED_FACE('',(#4205),#1751,.T.);
#28114=ADVANCED_FACE('',(#4206),#1752,.T.);
#28115=ADVANCED_FACE('',(#4207),#1753,.T.);
#28116=ADVANCED_FACE('',(#4208),#1754,.T.);
#28117=ADVANCED_FACE('',(#4209),#1755,.T.);
#28118=ADVANCED_FACE('',(#4210),#1756,.T.);
#28119=ADVANCED_FACE('',(#4211),#1757,.T.);
#28120=ADVANCED_FACE('',(#4212),#1758,.T.);
#28121=ADVANCED_FACE('',(#4213),#1759,.T.);
#28122=ADVANCED_FACE('',(#4214),#1760,.T.);
#28123=ADVANCED_FACE('',(#4215),#1761,.T.);
#28124=ADVANCED_FACE('',(#4216),#1762,.T.);
#28125=ADVANCED_FACE('',(#4217),#1763,.T.);
#28126=ADVANCED_FACE('',(#4218),#1764,.T.);
#28127=ADVANCED_FACE('',(#4219),#1765,.T.);
#28128=ADVANCED_FACE('',(#4220),#1766,.T.);
#28129=ADVANCED_FACE('',(#4221),#1767,.T.);
#28130=ADVANCED_FACE('',(#4222),#1768,.T.);
#28131=ADVANCED_FACE('',(#4223),#1769,.T.);
#28132=ADVANCED_FACE('',(#4224),#1770,.T.);
#28133=ADVANCED_FACE('',(#4225),#1771,.T.);
#28134=ADVANCED_FACE('',(#4226),#1772,.T.);
#28135=ADVANCED_FACE('',(#4227),#1773,.T.);
#28136=ADVANCED_FACE('',(#4228),#1774,.T.);
#28137=ADVANCED_FACE('',(#4229),#1775,.T.);
#28138=ADVANCED_FACE('',(#4230),#1776,.T.);
#28139=ADVANCED_FACE('',(#4231),#1777,.T.);
#28140=ADVANCED_FACE('',(#4232),#1778,.T.);
#28141=ADVANCED_FACE('',(#4233),#1779,.T.);
#28142=ADVANCED_FACE('',(#4234),#1780,.T.);
#28143=ADVANCED_FACE('',(#4235),#1781,.T.);
#28144=ADVANCED_FACE('',(#4236),#1782,.T.);
#28145=ADVANCED_FACE('',(#4237),#1783,.T.);
#28146=ADVANCED_FACE('',(#4238),#1784,.T.);
#28147=ADVANCED_FACE('',(#4239),#1785,.T.);
#28148=ADVANCED_FACE('',(#4240),#1786,.T.);
#28149=ADVANCED_FACE('',(#4241),#1787,.T.);
#28150=ADVANCED_FACE('',(#4242),#1788,.T.);
#28151=ADVANCED_FACE('',(#4243),#1789,.T.);
#28152=ADVANCED_FACE('',(#4244),#1790,.T.);
#28153=ADVANCED_FACE('',(#4245),#1791,.T.);
#28154=ADVANCED_FACE('',(#4246),#1792,.T.);
#28155=ADVANCED_FACE('',(#4247),#1793,.T.);
#28156=ADVANCED_FACE('',(#4248),#1794,.T.);
#28157=ADVANCED_FACE('',(#4249),#1795,.T.);
#28158=ADVANCED_FACE('',(#4250),#1796,.T.);
#28159=ADVANCED_FACE('',(#4251),#1797,.T.);
#28160=ADVANCED_FACE('',(#4252),#1798,.T.);
#28161=ADVANCED_FACE('',(#4253),#1799,.T.);
#28162=ADVANCED_FACE('',(#4254),#1800,.T.);
#28163=ADVANCED_FACE('',(#4255),#1801,.T.);
#28164=ADVANCED_FACE('',(#4256),#1802,.T.);
#28165=ADVANCED_FACE('',(#4257),#1803,.T.);
#28166=ADVANCED_FACE('',(#4258),#1804,.T.);
#28167=ADVANCED_FACE('',(#4259),#1805,.T.);
#28168=ADVANCED_FACE('',(#4260),#1806,.T.);
#28169=ADVANCED_FACE('',(#4261),#1807,.T.);
#28170=ADVANCED_FACE('',(#4262),#1808,.T.);
#28171=ADVANCED_FACE('',(#4263),#1809,.T.);
#28172=ADVANCED_FACE('',(#4264),#1810,.T.);
#28173=ADVANCED_FACE('',(#4265),#1811,.T.);
#28174=ADVANCED_FACE('',(#4266),#1812,.T.);
#28175=ADVANCED_FACE('',(#4267),#1813,.T.);
#28176=ADVANCED_FACE('',(#4268),#1814,.T.);
#28177=ADVANCED_FACE('',(#4269),#1815,.T.);
#28178=ADVANCED_FACE('',(#4270),#1816,.T.);
#28179=ADVANCED_FACE('',(#4271),#1817,.T.);
#28180=ADVANCED_FACE('',(#4272),#1818,.T.);
#28181=ADVANCED_FACE('',(#4273),#1819,.T.);
#28182=ADVANCED_FACE('',(#4274),#1820,.T.);
#28183=ADVANCED_FACE('',(#4275),#1821,.T.);
#28184=ADVANCED_FACE('',(#4276),#1822,.T.);
#28185=ADVANCED_FACE('',(#4277),#1823,.T.);
#28186=ADVANCED_FACE('',(#4278),#1824,.T.);
#28187=ADVANCED_FACE('',(#4279),#1825,.T.);
#28188=ADVANCED_FACE('',(#4280),#1826,.T.);
#28189=ADVANCED_FACE('',(#4281),#1827,.T.);
#28190=ADVANCED_FACE('',(#4282),#1464,.F.);
#28191=ADVANCED_FACE('',(#4283),#1465,.F.);
#28192=ADVANCED_FACE('',(#4284),#1466,.F.);
#28193=ADVANCED_FACE('',(#4285),#1467,.F.);
#28194=ADVANCED_FACE('',(#4286),#1468,.F.);
#28195=ADVANCED_FACE('',(#4287),#1469,.F.);
#28196=ADVANCED_FACE('',(#4288),#1470,.F.);
#28197=ADVANCED_FACE('',(#4289),#1471,.F.);
#28198=ADVANCED_FACE('',(#4290),#1472,.F.);
#28199=ADVANCED_FACE('',(#4291),#1473,.F.);
#28200=ADVANCED_FACE('',(#4292),#1474,.F.);
#28201=ADVANCED_FACE('',(#4293),#1475,.F.);
#28202=ADVANCED_FACE('',(#4294),#1476,.F.);
#28203=ADVANCED_FACE('',(#4295),#1477,.F.);
#28204=ADVANCED_FACE('',(#4296),#1478,.F.);
#28205=ADVANCED_FACE('',(#4297),#1479,.F.);
#28206=ADVANCED_FACE('',(#4298),#1480,.F.);
#28207=ADVANCED_FACE('',(#4299),#1481,.F.);
#28208=ADVANCED_FACE('',(#4300),#1482,.F.);
#28209=ADVANCED_FACE('',(#4301),#1483,.F.);
#28210=ADVANCED_FACE('',(#4302),#1484,.F.);
#28211=ADVANCED_FACE('',(#4303),#1485,.F.);
#28212=ADVANCED_FACE('',(#4304),#1486,.F.);
#28213=ADVANCED_FACE('',(#4305),#1487,.F.);
#28214=ADVANCED_FACE('',(#4306),#1488,.F.);
#28215=ADVANCED_FACE('',(#4307),#1489,.F.);
#28216=ADVANCED_FACE('',(#4308),#1490,.F.);
#28217=ADVANCED_FACE('',(#4309),#1491,.F.);
#28218=ADVANCED_FACE('',(#4310),#1492,.F.);
#28219=ADVANCED_FACE('',(#4311),#1493,.F.);
#28220=ADVANCED_FACE('',(#4312),#1494,.F.);
#28221=ADVANCED_FACE('',(#4313),#1495,.F.);
#28222=ADVANCED_FACE('',(#4314),#1496,.F.);
#28223=ADVANCED_FACE('',(#4315,#1976,#1977),#26803,.T.);
#28224=ADVANCED_FACE('',(#4316),#26804,.F.);
#28225=ADVANCED_FACE('',(#4317),#26805,.F.);
#28226=ADVANCED_FACE('',(#4318),#26806,.F.);
#28227=ADVANCED_FACE('',(#4319),#26807,.F.);
#28228=ADVANCED_FACE('',(#4320),#26808,.F.);
#28229=ADVANCED_FACE('',(#4321),#1497,.F.);
#28230=ADVANCED_FACE('',(#4322),#1498,.F.);
#28231=ADVANCED_FACE('',(#4323),#1499,.F.);
#28232=ADVANCED_FACE('',(#4324),#1500,.F.);
#28233=ADVANCED_FACE('',(#4325),#1501,.F.);
#28234=ADVANCED_FACE('',(#4326),#1502,.F.);
#28235=ADVANCED_FACE('',(#4327),#1503,.F.);
#28236=ADVANCED_FACE('',(#4328),#1504,.F.);
#28237=ADVANCED_FACE('',(#4329),#1505,.F.);
#28238=ADVANCED_FACE('',(#4330),#1506,.F.);
#28239=ADVANCED_FACE('',(#4331),#1507,.F.);
#28240=ADVANCED_FACE('',(#4332),#1508,.F.);
#28241=ADVANCED_FACE('',(#4333),#1509,.F.);
#28242=ADVANCED_FACE('',(#4334),#1510,.F.);
#28243=ADVANCED_FACE('',(#4335),#1511,.F.);
#28244=ADVANCED_FACE('',(#4336),#1512,.F.);
#28245=ADVANCED_FACE('',(#4337),#1513,.F.);
#28246=ADVANCED_FACE('',(#4338),#1514,.F.);
#28247=ADVANCED_FACE('',(#4339),#1515,.F.);
#28248=ADVANCED_FACE('',(#4340),#1516,.F.);
#28249=ADVANCED_FACE('',(#4341),#1517,.F.);
#28250=ADVANCED_FACE('',(#4342),#1518,.F.);
#28251=ADVANCED_FACE('',(#4343),#1519,.F.);
#28252=ADVANCED_FACE('',(#4344),#1520,.F.);
#28253=ADVANCED_FACE('',(#4345),#1521,.F.);
#28254=ADVANCED_FACE('',(#4346),#1522,.F.);
#28255=ADVANCED_FACE('',(#4347),#1523,.F.);
#28256=ADVANCED_FACE('',(#4348),#1524,.F.);
#28257=ADVANCED_FACE('',(#4349),#1525,.F.);
#28258=ADVANCED_FACE('',(#4350),#1526,.F.);
#28259=ADVANCED_FACE('',(#4351),#1527,.F.);
#28260=ADVANCED_FACE('',(#4352),#1528,.F.);
#28261=ADVANCED_FACE('',(#4353),#1529,.F.);
#28262=ADVANCED_FACE('',(#4354,#1978,#1979),#26809,.T.);
#28263=ADVANCED_FACE('',(#4355),#26810,.T.);
#28264=ADVANCED_FACE('',(#4356),#26811,.T.);
#28265=ADVANCED_FACE('',(#4357),#26812,.T.);
#28266=ADVANCED_FACE('',(#4358),#26813,.T.);
#28267=ADVANCED_FACE('',(#4359),#26814,.F.);
#28268=ADVANCED_FACE('',(#4360),#1530,.F.);
#28269=ADVANCED_FACE('',(#4361),#26815,.T.);
#28270=ADVANCED_FACE('',(#4362),#1828,.T.);
#28271=ADVANCED_FACE('',(#4363),#1531,.F.);
#28272=ADVANCED_FACE('',(#4364),#381,.F.);
#28273=ADVANCED_FACE('',(#4365,#1980),#26816,.F.);
#28274=ADVANCED_FACE('',(#4366),#1829,.T.);
#28275=ADVANCED_FACE('',(#4367),#2893,.T.);
#28276=ADVANCED_FACE('',(#4368),#26817,.T.);
#28277=ADVANCED_FACE('',(#4369),#26818,.T.);
#28278=ADVANCED_FACE('',(#4370),#26819,.T.);
#28279=ADVANCED_FACE('',(#4371),#26820,.T.);
#28280=ADVANCED_FACE('',(#4372),#26821,.T.);
#28281=ADVANCED_FACE('',(#4373),#26822,.T.);
#28282=ADVANCED_FACE('',(#4374,#1981,#1982,#1983),#26823,.T.);
#28283=ADVANCED_FACE('',(#4375),#26824,.T.);
#28284=ADVANCED_FACE('',(#4376),#2894,.T.);
#28285=ADVANCED_FACE('',(#4377),#2895,.F.);
#28286=ADVANCED_FACE('',(#4378),#1830,.F.);
#28287=ADVANCED_FACE('',(#4379,#1984),#26825,.F.);
#28288=ADVANCED_FACE('',(#4380),#2896,.F.);
#28289=ADVANCED_FACE('',(#4381,#1985),#26826,.T.);
#28290=ADVANCED_FACE('',(#4382),#2897,.T.);
#28291=ADVANCED_FACE('',(#4383),#26827,.T.);
#28292=ADVANCED_FACE('',(#4384),#26828,.T.);
#28293=ADVANCED_FACE('',(#4385),#26829,.T.);
#28294=ADVANCED_FACE('',(#4386),#2898,.T.);
#28295=ADVANCED_FACE('',(#4387),#26830,.T.);
#28296=ADVANCED_FACE('',(#4388),#26831,.T.);
#28297=ADVANCED_FACE('',(#4389),#26832,.T.);
#28298=ADVANCED_FACE('',(#4390),#1831,.F.);
#28299=ADVANCED_FACE('',(#4391,#1986),#26833,.T.);
#28300=ADVANCED_FACE('',(#4392),#1832,.T.);
#28301=ADVANCED_FACE('',(#4393),#2899,.T.);
#28302=ADVANCED_FACE('',(#4394,#1987),#26834,.T.);
#28303=ADVANCED_FACE('',(#4395),#2900,.F.);
#28304=ADVANCED_FACE('',(#4396),#2901,.T.);
#28305=ADVANCED_FACE('',(#4397),#2902,.T.);
#28306=ADVANCED_FACE('',(#4398),#26835,.T.);
#28307=ADVANCED_FACE('',(#4399),#2903,.T.);
#28308=ADVANCED_FACE('',(#4400),#1833,.T.);
#28309=ADVANCED_FACE('',(#4401),#2904,.F.);
#28310=ADVANCED_FACE('',(#4402),#1834,.F.);
#28311=ADVANCED_FACE('',(#4403,#1988),#26836,.T.);
#28312=ADVANCED_FACE('',(#4404),#2905,.F.);
#28313=ADVANCED_FACE('',(#4405,#1989),#26837,.F.);
#28314=ADVANCED_FACE('',(#4406),#2906,.T.);
#28315=ADVANCED_FACE('',(#4407),#1835,.T.);
#28316=ADVANCED_FACE('',(#4408,#1990),#26838,.T.);
#28317=ADVANCED_FACE('',(#4409,#1991),#26839,.F.);
#28318=ADVANCED_FACE('',(#4410),#1836,.T.);
#28319=ADVANCED_FACE('',(#4411,#1992),#26840,.F.);
#28320=ADVANCED_FACE('',(#4412),#1837,.T.);
#28321=ADVANCED_FACE('',(#4413,#1993),#26841,.F.);
#28322=ADVANCED_FACE('',(#4414),#1838,.T.);
#28323=ADVANCED_FACE('',(#4415,#1994),#26842,.F.);
#28324=ADVANCED_FACE('',(#4416),#1839,.T.);
#28325=ADVANCED_FACE('',(#4417,#1995),#26843,.F.);
#28326=ADVANCED_FACE('',(#4418),#1840,.T.);
#28327=ADVANCED_FACE('',(#4419,#1996),#26844,.F.);
#28328=ADVANCED_FACE('',(#4420,#1997),#26845,.T.);
#28329=ADVANCED_FACE('',(#4421),#2907,.T.);
#28330=ADVANCED_FACE('',(#4422),#1841,.T.);
#28331=ADVANCED_FACE('',(#4423),#2908,.T.);
#28332=ADVANCED_FACE('',(#4424,#1998),#26846,.T.);
#28333=ADVANCED_FACE('',(#4425),#1842,.T.);
#28334=ADVANCED_FACE('',(#4426),#26847,.T.);
#28335=ADVANCED_FACE('',(#4427),#26848,.T.);
#28336=ADVANCED_FACE('',(#4428),#26849,.T.);
#28337=ADVANCED_FACE('',(#4429),#2909,.T.);
#28338=ADVANCED_FACE('',(#4430),#26850,.T.);
#28339=ADVANCED_FACE('',(#4431),#1843,.T.);
#28340=ADVANCED_FACE('',(#4432),#26851,.T.);
#28341=ADVANCED_FACE('',(#4433),#2910,.T.);
#28342=ADVANCED_FACE('',(#4434),#26852,.T.);
#28343=ADVANCED_FACE('',(#4435),#2911,.F.);
#28344=ADVANCED_FACE('',(#4436,#1999,#2000,#2001,#2002,#2003,#2004,#2005,
#2006,#2007,#2008,#2009),#26853,.T.);
#28345=ADVANCED_FACE('',(#4437),#1844,.F.);
#28346=ADVANCED_FACE('',(#4438),#2912,.F.);
#28347=ADVANCED_FACE('',(#4439),#1845,.F.);
#28348=ADVANCED_FACE('',(#4440),#2913,.F.);
#28349=ADVANCED_FACE('',(#4441),#1846,.F.);
#28350=ADVANCED_FACE('',(#4442),#2914,.F.);
#28351=ADVANCED_FACE('',(#4443),#1847,.F.);
#28352=ADVANCED_FACE('',(#4444),#2915,.F.);
#28353=ADVANCED_FACE('',(#4445),#1848,.F.);
#28354=ADVANCED_FACE('',(#4446),#2916,.F.);
#28355=ADVANCED_FACE('',(#4447),#1849,.F.);
#28356=ADVANCED_FACE('',(#4448),#2917,.F.);
#28357=ADVANCED_FACE('',(#4449),#1850,.F.);
#28358=ADVANCED_FACE('',(#4450),#2918,.F.);
#28359=ADVANCED_FACE('',(#4451,#2010,#2011,#2012,#2013,#2014,#2015,#2016,
#2017,#2018,#2019,#2020),#26854,.T.);
#28360=ADVANCED_FACE('',(#4452),#1851,.F.);
#28361=ADVANCED_FACE('',(#4453),#2919,.F.);
#28362=ADVANCED_FACE('',(#4454),#1852,.F.);
#28363=ADVANCED_FACE('',(#4455),#2920,.F.);
#28364=ADVANCED_FACE('',(#4456),#1853,.F.);
#28365=ADVANCED_FACE('',(#4457),#2921,.F.);
#28366=ADVANCED_FACE('',(#4458),#1854,.F.);
#28367=ADVANCED_FACE('',(#4459),#2922,.F.);
#28368=ADVANCED_FACE('',(#4460),#1855,.F.);
#28369=ADVANCED_FACE('',(#4461),#26855,.T.);
#28370=ADVANCED_FACE('',(#4462),#2923,.F.);
#28371=ADVANCED_FACE('',(#4463),#26856,.T.);
#28372=ADVANCED_FACE('',(#4464),#2924,.F.);
#28373=ADVANCED_FACE('',(#4465),#26857,.T.);
#28374=ADVANCED_FACE('',(#4466),#2925,.F.);
#28375=ADVANCED_FACE('',(#4467),#26858,.T.);
#28376=ADVANCED_FACE('',(#4468),#2926,.F.);
#28377=ADVANCED_FACE('',(#4469),#1856,.F.);
#28378=ADVANCED_FACE('',(#4470),#26859,.T.);
#28379=ADVANCED_FACE('',(#4471),#1857,.F.);
#28380=ADVANCED_FACE('',(#4472,#2021),#26860,.F.);
#28381=ADVANCED_FACE('',(#4473),#2927,.F.);
#28382=ADVANCED_FACE('',(#4474),#1858,.F.);
#28383=ADVANCED_FACE('',(#4475),#2928,.F.);
#28384=ADVANCED_FACE('',(#4476),#1859,.F.);
#28385=ADVANCED_FACE('',(#4477),#2929,.F.);
#28386=ADVANCED_FACE('',(#4478),#1860,.F.);
#28387=ADVANCED_FACE('',(#4479),#2930,.F.);
#28388=ADVANCED_FACE('',(#4480),#1861,.F.);
#28389=ADVANCED_FACE('',(#4481),#2931,.F.);
#28390=ADVANCED_FACE('',(#4482),#1862,.F.);
#28391=ADVANCED_FACE('',(#4483),#2932,.F.);
#28392=ADVANCED_FACE('',(#4484),#1863,.F.);
#28393=ADVANCED_FACE('',(#4485),#2933,.F.);
#28394=ADVANCED_FACE('',(#4486),#1864,.F.);
#28395=ADVANCED_FACE('',(#4487),#2934,.F.);
#28396=ADVANCED_FACE('',(#4488),#1865,.F.);
#28397=ADVANCED_FACE('',(#4489),#2935,.F.);
#28398=ADVANCED_FACE('',(#4490),#1866,.F.);
#28399=ADVANCED_FACE('',(#4491),#2936,.F.);
#28400=ADVANCED_FACE('',(#4492,#2022,#2023,#2024,#2025,#2026,#2027,#2028,
#2029,#2030,#2031,#2032),#26861,.T.);
#28401=ADVANCED_FACE('',(#4493),#2937,.F.);
#28402=ADVANCED_FACE('',(#4494),#2938,.F.);
#28403=ADVANCED_FACE('',(#4495),#2939,.F.);
#28404=ADVANCED_FACE('',(#4496),#2940,.F.);
#28405=ADVANCED_FACE('',(#4497),#2941,.F.);
#28406=ADVANCED_FACE('',(#4498),#1867,.F.);
#28407=ADVANCED_FACE('',(#4499),#2942,.F.);
#28408=ADVANCED_FACE('',(#4500,#2033,#2034,#2035,#2036,#2037,#2038,#2039,
#2040,#2041,#2042,#2043),#26862,.T.);
#28409=ADVANCED_FACE('',(#4501),#2943,.F.);
#28410=ADVANCED_FACE('',(#4502),#2944,.F.);
#28411=ADVANCED_FACE('',(#4503),#2945,.F.);
#28412=ADVANCED_FACE('',(#4504),#2946,.F.);
#28413=ADVANCED_FACE('',(#4505),#26863,.T.);
#28414=ADVANCED_FACE('',(#4506),#2947,.T.);
#28415=ADVANCED_FACE('',(#4507),#26864,.T.);
#28416=ADVANCED_FACE('',(#4508),#2948,.T.);
#28417=ADVANCED_FACE('',(#4509),#26865,.T.);
#28418=ADVANCED_FACE('',(#4510),#2949,.T.);
#28419=ADVANCED_FACE('',(#4511),#26866,.T.);
#28420=ADVANCED_FACE('',(#4512),#2950,.T.);
#28421=ADVANCED_FACE('',(#4513),#1868,.T.);
#28422=ADVANCED_FACE('',(#4514),#26867,.T.);
#28423=ADVANCED_FACE('',(#4515),#1869,.T.);
#28424=ADVANCED_FACE('',(#4516),#2951,.F.);
#28425=ADVANCED_FACE('',(#4517),#2952,.F.);
#28426=ADVANCED_FACE('',(#4518),#2953,.F.);
#28427=ADVANCED_FACE('',(#4519),#2954,.F.);
#28428=ADVANCED_FACE('',(#4520),#2955,.F.);
#28429=ADVANCED_FACE('',(#4521),#2956,.F.);
#28430=ADVANCED_FACE('',(#4522),#2957,.F.);
#28431=ADVANCED_FACE('',(#4523),#2958,.F.);
#28432=ADVANCED_FACE('',(#4524),#2959,.F.);
#28433=ADVANCED_FACE('',(#4525),#2960,.F.);
#28434=ADVANCED_FACE('',(#4526),#2961,.F.);
#28435=ADVANCED_FACE('',(#4527),#2962,.F.);
#28436=ADVANCED_FACE('',(#4528),#2963,.T.);
#28437=ADVANCED_FACE('',(#4529),#26868,.T.);
#28438=ADVANCED_FACE('',(#4530),#2964,.T.);
#28439=ADVANCED_FACE('',(#4531),#26869,.T.);
#28440=ADVANCED_FACE('',(#4532),#2965,.T.);
#28441=ADVANCED_FACE('',(#4533),#26870,.T.);
#28442=ADVANCED_FACE('',(#4534),#2966,.T.);
#28443=ADVANCED_FACE('',(#4535),#26871,.T.);
#28444=ADVANCED_FACE('',(#4536),#1870,.T.);
#28445=ADVANCED_FACE('',(#4537,#2044),#26872,.T.);
#28446=ADVANCED_FACE('',(#4538),#2967,.F.);
#28447=ADVANCED_FACE('',(#4539),#26873,.T.);
#28448=ADVANCED_FACE('',(#4540),#2968,.F.);
#28449=ADVANCED_FACE('',(#4541),#26874,.T.);
#28450=ADVANCED_FACE('',(#4542),#2969,.F.);
#28451=ADVANCED_FACE('',(#4543),#26875,.T.);
#28452=ADVANCED_FACE('',(#4544),#2970,.F.);
#28453=ADVANCED_FACE('',(#4545),#26876,.T.);
#28454=ADVANCED_FACE('',(#4546),#1871,.F.);
#28455=ADVANCED_FACE('',(#4547),#1872,.F.);
#28456=ADVANCED_FACE('',(#4548),#26877,.T.);
#28457=ADVANCED_FACE('',(#4549),#26878,.T.);
#28458=ADVANCED_FACE('',(#4550),#1873,.T.);
#28459=CLOSED_SHELL('',(#26879,#26880,#26881,#26882,#26883,#26884,#26885,
#26886,#26887,#26888,#26889,#26890,#26891,#26892,#26893,#26894,#26895,#26896,
#26897,#26898,#26899,#26900,#26901,#26902,#26903,#26904,#26905,#26906,#26907,
#26908,#26909,#26910,#26911,#26912,#26913,#26914,#26915,#26916,#26917,#26918,
#26919,#26920,#26921,#26922,#26923,#26924,#26925,#26926,#26927,#26928,#26929,
#26930,#26931,#26932,#26933,#26934,#26935,#26936,#26937,#26938,#26939,#26940,
#26941,#26942,#26943,#26944,#26945,#26946,#26947,#26948,#26949,#26950,#26951,
#26952,#26953,#26954,#26955,#26956,#26957,#26958,#26959,#26960,#26961,#26962,
#26963,#26964,#26965,#26966,#26967,#26968,#26969,#26970,#26971,#26972,#26973,
#26974,#26975,#26976,#26977,#26978,#26979,#26980,#26981,#26982,#26983,#26984,
#26985,#26986,#26987,#26988,#26989,#26990,#26991,#26992,#26993,#26994,#26995,
#26996,#26997,#26998,#26999,#27000,#27001,#27002,#27003,#27004,#27005,#27006,
#27007,#27008,#27009,#27010,#27011,#27012,#27013,#27014,#27015,#27016,#27017,
#27018,#27019,#27020,#27021,#27022,#27023,#27024,#27025,#27026,#27027,#27028,
#27029,#27030,#27031,#27032,#27033,#27034,#27035,#27036,#27037,#27038,#27039,
#27040,#27041,#27042,#27043,#27044,#27045,#27046,#27047,#27048,#27049,#27050,
#27051,#27052,#27053,#27054,#27055,#27056,#27057,#27058,#27059,#27060,#27061,
#27062,#27063,#27064,#27065,#27066,#27067,#27068,#27069,#27070,#27071,#27072,
#27073,#27074,#27075,#27076,#27077,#27078,#27079,#27080,#27081,#27082,#27083,
#27084,#27085,#27086,#27087,#27088,#27089,#27090,#27091,#27092,#27093,#27094,
#27095,#27096,#27097,#27098,#27099,#27100,#27101,#27102,#27103,#27104,#27105,
#27106,#27107,#27108,#27109,#27110,#27111,#27112,#27113,#27114,#27115,#27116,
#27117,#27118,#27119,#27120,#27121,#27122,#27123,#27124,#27125,#27126,#27127,
#27128,#27129,#27130,#27131,#27132,#27133,#27134,#27135,#27136,#27137,#27138,
#27139,#27140,#27141,#27142,#27143,#27144,#27145,#27146,#27147,#27148,#27149,
#27150,#27151,#27152,#27153,#27154,#27155,#27156,#27157,#27158,#27159,#27160,
#27161,#27162,#27163,#27164,#27165,#27166,#27167,#27168,#27169,#27170,#27171,
#27172,#27173,#27174,#27175,#27176,#27177,#27178,#27179,#27180,#27181,#27182,
#27183,#27184,#27185,#27186,#27187));
#28460=CLOSED_SHELL('',(#27188,#27189,#27190,#27191,#27192,#27193,#27194,
#27195,#27196,#27197,#27198,#27199,#27200,#27201,#27202,#27203,#27204,#27205,
#27206,#27207,#27208,#27209,#27210,#27211,#27212,#27213,#27214,#27215,#27216,
#27217,#27218,#27219,#27220,#27221,#27222,#27223,#27224,#27225,#27226,#27227,
#27228,#27229,#27230,#27231,#27232,#27233,#27234,#27235,#27236,#27237,#27238,
#27239,#27240,#27241,#27242,#27243,#27244,#27245,#27246,#27247,#27248,#27249,
#27250,#27251,#27252,#27253,#27254,#27255,#27256,#27257,#27258,#27259,#27260,
#27261,#27262,#27263,#27264,#27265,#27266,#27267,#27268,#27269,#27270,#27271,
#27272,#27273,#27274,#27275,#27276,#27277,#27278,#27279,#27280,#27281,#27282,
#27283,#27284,#27285,#27286,#27287,#27288,#27289,#27290,#27291,#27292,#27293,
#27294,#27295,#27296,#27297,#27298,#27299,#27300,#27301,#27302,#27303,#27304,
#27305));
#28461=CLOSED_SHELL('',(#27306,#27307,#27308,#27309,#27310,#27311,#27312,
#27313,#27314,#27315,#27316,#27317,#27318,#27319,#27320,#27321,#27322,#27323,
#27324,#27325,#27326,#27327,#27328,#27329,#27330,#27331,#27332,#27333,#27334,
#27335,#27336,#27337,#27338,#27339,#27340,#27341,#27342,#27343,#27344,#27345,
#27346,#27347,#27348,#27349,#27350,#27351,#27352,#27353,#27354,#27355,#27356,
#27357,#27358,#27359,#27360,#27361,#27362,#27363,#27364,#27365,#27366,#27367,
#27368,#27369,#27370,#27371,#27372,#27373,#27374,#27375,#27376,#27377,#27378,
#27379,#27380,#27381,#27382,#27383,#27384,#27385,#27386,#27387,#27388,#27389,
#27390,#27391,#27392,#27393,#27394,#27395,#27396,#27397,#27398,#27399,#27400,
#27401,#27402,#27403,#27404,#27405,#27406,#27407,#27408,#27409,#27410,#27411,
#27412,#27413));
#28462=CLOSED_SHELL('',(#27414,#27415,#27416,#27417,#27418,#27419,#27420,
#27421,#27422,#27423,#27424,#27425,#27426,#27427,#27428,#27429,#27430,#27431,
#27432,#27433,#27434,#27435,#27436,#27437,#27438,#27439,#27440,#27441,#27442,
#27443,#27444));
#28463=CLOSED_SHELL('',(#27445,#27446,#27447,#27448,#27449,#27450,#27451,
#27452,#27453,#27454,#27455,#27456,#27457,#27458,#27459,#27460,#27461,#27462,
#27463,#27464,#27465,#27466,#27467,#27468,#27469,#27470,#27471,#27472,#27473,
#27474,#27475,#27476,#27477,#27478,#27479,#27480,#27481,#27482,#27483,#27484,
#27485,#27486,#27487,#27488,#27489,#27490,#27491,#27492,#27493,#27494,#27495,
#27496,#27497,#27498,#27499,#27500,#27501,#27502,#27503,#27504,#27505,#27506,
#27507,#27508,#27509,#27510,#27511,#27512,#27513,#27514,#27515,#27516,#27517,
#27518,#27519,#27520,#27521,#27522,#27523,#27524,#27525,#27526,#27527,#27528,
#27529,#27530,#27531,#27532,#27533,#27534,#27535,#27536,#27537,#27538,#27539,
#27540,#27541,#27542,#27543,#27544,#27545,#27546,#27547,#27548,#27549,#27550,
#27551,#27552,#27553,#27554));
#28464=CLOSED_SHELL('',(#27555,#27556,#27557,#27558,#27559,#27560,#27561,
#27562,#27563,#27564,#27565,#27566,#27567,#27568,#27569,#27570,#27571,#27572,
#27573,#27574,#27575,#27576,#27577,#27578,#27579,#27580,#27581,#27582,#27583,
#27584,#27585,#27586,#27587,#27588,#27589,#27590,#27591,#27592,#27593,#27594,
#27595,#27596,#27597,#27598,#27599,#27600,#27601,#27602,#27603,#27604,#27605,
#27606,#27607,#27608,#27609,#27610,#27611,#27612,#27613,#27614,#27615,#27616,
#27617,#27618,#27619,#27620,#27621,#27622,#27623,#27624,#27625,#27626,#27627,
#27628,#27629,#27630,#27631,#27632,#27633,#27634,#27635,#27636,#27637,#27638,
#27639,#27640,#27641,#27642,#27643,#27644,#27645,#27646,#27647,#27648,#27649,
#27650,#27651,#27652,#27653,#27654,#27655,#27656,#27657,#27658,#27659,#27660,
#27661,#27662,#27663,#27664,#27665,#27666,#27667,#27668,#27669,#27670,#27671,
#27672));
#28465=CLOSED_SHELL('',(#27673,#27674,#27675,#27676,#27677,#27678,#27679,
#27680,#27681,#27682,#27683,#27684,#27685,#27686,#27687,#27688,#27689,#27690,
#27691,#27692,#27693,#27694,#27695,#27696,#27697,#27698,#27699,#27700,#27701,
#27702,#27703,#27704,#27705,#27706,#27707,#27708,#27709,#27710,#27711,#27712,
#27713,#27714,#27715,#27716,#27717,#27718,#27719,#27720,#27721,#27722,#27723,
#27724,#27725,#27726,#27727,#27728,#27729,#27730,#27731,#27732,#27733,#27734,
#27735,#27736,#27737,#27738,#27739,#27740,#27741,#27742,#27743,#27744,#27745,
#27746,#27747,#27748,#27749,#27750,#27751,#27752,#27753,#27754,#27755,#27756,
#27757,#27758,#27759,#27760,#27761,#27762,#27763,#27764,#27765,#27766,#27767,
#27768));
#28466=CLOSED_SHELL('',(#27769,#27770,#27771,#27772,#27773,#27774,#27775,
#27776,#27777,#27778,#27779,#27780,#27781,#27782,#27783,#27784,#27785,#27786,
#27787,#27788,#27789,#27790,#27791,#27792,#27793,#27794,#27795,#27796,#27797,
#27798,#27799,#27800,#27801,#27802,#27803,#27804,#27805,#27806,#27807,#27808,
#27809,#27810,#27811,#27812,#27813,#27814,#27815,#27816,#27817,#27818,#27819,
#27820,#27821,#27822,#27823,#27824,#27825,#27826,#27827,#27828,#27829,#27830,
#27831,#27832,#27833,#27834,#27835,#27836,#27837,#27838,#27839,#27840,#27841,
#27842,#27843,#27844,#27845,#27846,#27847,#27848,#27849,#27850,#27851,#27852,
#27853));
#28467=CLOSED_SHELL('',(#27854,#27855,#27856,#27857,#27858,#27859,#27860,
#27861,#27862,#27863,#27864,#27865,#27866,#27867,#27868));
#28468=CLOSED_SHELL('',(#27869,#27870,#27871));
#28469=CLOSED_SHELL('',(#27872,#27873,#27874,#27875,#27876,#27877,#27878,
#27879,#27880,#27881,#27882,#27883,#27884,#27885,#27886,#27887,#27888,#27889,
#27890,#27891,#27892,#27893,#27894,#27895,#27896,#27897,#27898,#27899,#27900,
#27901,#27902,#27903,#27904,#27905,#27906,#27907,#27908,#27909,#27910,#27911,
#27912,#27913,#27914,#27915,#27916,#27917,#27918,#27919,#27920,#27921,#27922,
#27923,#27924,#27925,#27926,#27927,#27928,#27929,#27930,#27931,#27932,#27933,
#27934,#27935,#27936,#27937,#27938,#27939,#27940,#27941,#27942,#27943,#27944,
#27945,#27946,#27947,#27948,#27949,#27950,#27951,#27952,#27953,#27954,#27955,
#27956,#27957,#27958,#27959,#27960,#27961,#27962,#27963,#27964,#27965,#27966,
#27967,#27968,#27969,#27970,#27971,#27972,#27973,#27974,#27975,#27976,#27977));
#28470=CLOSED_SHELL('',(#27978,#27979,#27980,#27981,#27982,#27983,#27984,
#27985,#27986,#27987));
#28471=CLOSED_SHELL('',(#27988,#27989,#27990,#27991,#27992,#27993,#27994,
#27995,#27996,#27997,#27998,#27999,#28000,#28001,#28002,#28003,#28004,#28005,
#28006,#28007,#28008,#28009,#28010,#28011,#28012,#28013,#28014,#28015,#28016,
#28017,#28018,#28019,#28020,#28021,#28022,#28023,#28024,#28025));
#28472=CLOSED_SHELL('',(#28026,#28027,#28028,#28029,#28030,#28031,#28032,
#28033,#28034,#28035,#28036,#28037,#28038,#28039,#28040,#28041,#28042,#28043,
#28044,#28045,#28046,#28047,#28048,#28049,#28050,#28051,#28052,#28053,#28054,
#28055,#28056,#28057,#28058,#28059,#28060,#28061,#28062,#28063,#28064,#28065,
#28066,#28067,#28068,#28069,#28070));
#28473=CLOSED_SHELL('',(#28071,#28072,#28073,#28074,#28075,#28076,#28077,
#28078,#28079,#28080,#28081,#28082,#28083,#28084,#28085,#28086,#28087,#28088,
#28089,#28090,#28091,#28092,#28093,#28094,#28095,#28096,#28097,#28098,#28099,
#28100,#28101,#28102,#28103,#28104,#28105,#28106,#28107,#28108,#28109,#28110,
#28111,#28112,#28113,#28114,#28115,#28116,#28117,#28118,#28119,#28120,#28121,
#28122,#28123,#28124,#28125,#28126,#28127,#28128,#28129,#28130,#28131,#28132,
#28133,#28134,#28135,#28136,#28137,#28138,#28139,#28140,#28141,#28142,#28143,
#28144,#28145,#28146,#28147,#28148,#28149,#28150,#28151,#28152,#28153,#28154,
#28155,#28156,#28157,#28158,#28159,#28160,#28161,#28162,#28163,#28164,#28165,
#28166,#28167,#28168,#28169,#28170,#28171,#28172,#28173,#28174,#28175,#28176,
#28177,#28178,#28179,#28180,#28181,#28182,#28183,#28184,#28185,#28186,#28187,
#28188,#28189,#28190,#28191,#28192,#28193,#28194,#28195,#28196,#28197,#28198,
#28199,#28200,#28201,#28202,#28203,#28204,#28205,#28206,#28207,#28208,#28209,
#28210,#28211,#28212,#28213,#28214,#28215,#28216,#28217,#28218,#28219,#28220,
#28221,#28222,#28223,#28224,#28225,#28226,#28227,#28228,#28229,#28230,#28231,
#28232,#28233,#28234,#28235,#28236,#28237,#28238,#28239,#28240,#28241,#28242,
#28243,#28244,#28245,#28246,#28247,#28248,#28249,#28250,#28251,#28252,#28253,
#28254,#28255,#28256,#28257,#28258,#28259,#28260,#28261,#28262,#28263,#28264,
#28265,#28266,#28267,#28268,#28269,#28270,#28271,#28272,#28273,#28274,#28275,
#28276,#28277,#28278,#28279,#28280,#28281,#28282,#28283,#28284));
#28474=CLOSED_SHELL('',(#28285,#28286,#28287,#28288,#28289,#28290,#28291,
#28292,#28293,#28294,#28295,#28296,#28297));
#28475=CLOSED_SHELL('',(#28298,#28299,#28300,#28301,#28302,#28303));
#28476=CLOSED_SHELL('',(#28304,#28305,#28306,#28307,#28308,#28309,#28310,
#28311,#28312,#28313,#28314,#28315,#28316,#28317,#28318,#28319,#28320,#28321,
#28322,#28323,#28324,#28325,#28326,#28327,#28328,#28329,#28330,#28331,#28332,
#28333,#28334,#28335,#28336,#28337,#28338,#28339,#28340,#28341,#28342));
#28477=CLOSED_SHELL('',(#28343,#28344,#28345,#28346,#28347,#28348,#28349,
#28350,#28351,#28352,#28353,#28354,#28355,#28356,#28357,#28358,#28359,#28360,
#28361,#28362,#28363,#28364,#28365,#28366,#28367,#28368,#28369,#28370,#28371,
#28372,#28373,#28374,#28375,#28376,#28377,#28378,#28379,#28380,#28381,#28382,
#28383,#28384,#28385,#28386,#28387,#28388,#28389,#28390,#28391,#28392,#28393,
#28394,#28395,#28396,#28397,#28398,#28399,#28400,#28401,#28402,#28403,#28404,
#28405,#28406,#28407,#28408,#28409,#28410,#28411,#28412,#28413,#28414,#28415,
#28416,#28417,#28418,#28419,#28420,#28421,#28422,#28423,#28424,#28425,#28426,
#28427,#28428,#28429,#28430,#28431,#28432,#28433,#28434,#28435,#28436,#28437,
#28438,#28439,#28440,#28441,#28442,#28443,#28444,#28445,#28446,#28447,#28448,
#28449,#28450,#28451,#28452,#28453,#28454,#28455,#28456,#28457,#28458));
#28478=DERIVED_UNIT_ELEMENT(#28516,1.);
#28479=DERIVED_UNIT_ELEMENT(#71494,-3.);
#28480=DERIVED_UNIT_ELEMENT(#28516,1.);
#28481=DERIVED_UNIT_ELEMENT(#71494,-3.);
#28482=DERIVED_UNIT_ELEMENT(#28516,1.);
#28483=DERIVED_UNIT_ELEMENT(#71494,-3.);
#28484=DERIVED_UNIT_ELEMENT(#28516,1.);
#28485=DERIVED_UNIT_ELEMENT(#71494,-3.);
#28486=DERIVED_UNIT_ELEMENT(#28516,1.);
#28487=DERIVED_UNIT_ELEMENT(#71494,-3.);
#28488=DERIVED_UNIT_ELEMENT(#28516,1.);
#28489=DERIVED_UNIT_ELEMENT(#71494,-3.);
#28490=DERIVED_UNIT_ELEMENT(#28516,1.);
#28491=DERIVED_UNIT_ELEMENT(#71494,-3.);
#28492=DERIVED_UNIT_ELEMENT(#28516,1.);
#28493=DERIVED_UNIT_ELEMENT(#71494,-3.);
#28494=DERIVED_UNIT_ELEMENT(#28516,1.);
#28495=DERIVED_UNIT_ELEMENT(#71494,-3.);
#28496=DERIVED_UNIT_ELEMENT(#28516,1.);
#28497=DERIVED_UNIT_ELEMENT(#71494,-3.);
#28498=DERIVED_UNIT_ELEMENT(#28516,1.);
#28499=DERIVED_UNIT_ELEMENT(#71494,-3.);
#28500=DERIVED_UNIT_ELEMENT(#28516,1.);
#28501=DERIVED_UNIT_ELEMENT(#71494,-3.);
#28502=DERIVED_UNIT_ELEMENT(#28516,1.);
#28503=DERIVED_UNIT_ELEMENT(#71494,-3.);
#28504=DERIVED_UNIT_ELEMENT(#28516,1.);
#28505=DERIVED_UNIT_ELEMENT(#71494,-3.);
#28506=DERIVED_UNIT_ELEMENT(#28516,1.);
#28507=DERIVED_UNIT_ELEMENT(#71494,-3.);
#28508=DERIVED_UNIT_ELEMENT(#28516,1.);
#28509=DERIVED_UNIT_ELEMENT(#71494,-3.);
#28510=DERIVED_UNIT_ELEMENT(#28516,1.);
#28511=DERIVED_UNIT_ELEMENT(#71494,-3.);
#28512=DERIVED_UNIT_ELEMENT(#28516,1.);
#28513=DERIVED_UNIT_ELEMENT(#71494,-3.);
#28514=DERIVED_UNIT_ELEMENT(#28516,1.);
#28515=DERIVED_UNIT_ELEMENT(#71494,-3.);
#28516=(
MASS_UNIT()
NAMED_UNIT(*)
SI_UNIT(.KILO.,.GRAM.)
);
#28517=DERIVED_UNIT((#28478,#28479));
#28518=DERIVED_UNIT((#28480,#28481));
#28519=DERIVED_UNIT((#28482,#28483));
#28520=DERIVED_UNIT((#28484,#28485));
#28521=DERIVED_UNIT((#28486,#28487));
#28522=DERIVED_UNIT((#28488,#28489));
#28523=DERIVED_UNIT((#28490,#28491));
#28524=DERIVED_UNIT((#28492,#28493));
#28525=DERIVED_UNIT((#28494,#28495));
#28526=DERIVED_UNIT((#28496,#28497));
#28527=DERIVED_UNIT((#28498,#28499));
#28528=DERIVED_UNIT((#28500,#28501));
#28529=DERIVED_UNIT((#28502,#28503));
#28530=DERIVED_UNIT((#28504,#28505));
#28531=DERIVED_UNIT((#28506,#28507));
#28532=DERIVED_UNIT((#28508,#28509));
#28533=DERIVED_UNIT((#28510,#28511));
#28534=DERIVED_UNIT((#28512,#28513));
#28535=DERIVED_UNIT((#28514,#28515));
#28536=MEASURE_REPRESENTATION_ITEM('density measure',
POSITIVE_RATIO_MEASURE(7850.),#28517);
#28537=MEASURE_REPRESENTATION_ITEM('density measure',
POSITIVE_RATIO_MEASURE(7850.),#28518);
#28538=MEASURE_REPRESENTATION_ITEM('density measure',
POSITIVE_RATIO_MEASURE(7850.),#28519);
#28539=MEASURE_REPRESENTATION_ITEM('density measure',
POSITIVE_RATIO_MEASURE(7850.),#28520);
#28540=MEASURE_REPRESENTATION_ITEM('density measure',
POSITIVE_RATIO_MEASURE(7850.),#28521);
#28541=MEASURE_REPRESENTATION_ITEM('density measure',
POSITIVE_RATIO_MEASURE(7850.),#28522);
#28542=MEASURE_REPRESENTATION_ITEM('density measure',
POSITIVE_RATIO_MEASURE(1060.),#28523);
#28543=MEASURE_REPRESENTATION_ITEM('density measure',
POSITIVE_RATIO_MEASURE(7850.),#28524);
#28544=MEASURE_REPRESENTATION_ITEM('density measure',
POSITIVE_RATIO_MEASURE(7850.),#28525);
#28545=MEASURE_REPRESENTATION_ITEM('density measure',
POSITIVE_RATIO_MEASURE(7850.),#28526);
#28546=MEASURE_REPRESENTATION_ITEM('density measure',
POSITIVE_RATIO_MEASURE(7850.),#28527);
#28547=MEASURE_REPRESENTATION_ITEM('density measure',
POSITIVE_RATIO_MEASURE(7850.),#28528);
#28548=MEASURE_REPRESENTATION_ITEM('density measure',
POSITIVE_RATIO_MEASURE(7850.),#28529);
#28549=MEASURE_REPRESENTATION_ITEM('density measure',
POSITIVE_RATIO_MEASURE(7850.),#28530);
#28550=MEASURE_REPRESENTATION_ITEM('density measure',
POSITIVE_RATIO_MEASURE(7850.),#28531);
#28551=MEASURE_REPRESENTATION_ITEM('density measure',
POSITIVE_RATIO_MEASURE(7850.),#28532);
#28552=MEASURE_REPRESENTATION_ITEM('density measure',
POSITIVE_RATIO_MEASURE(7850.),#28533);
#28553=MEASURE_REPRESENTATION_ITEM('density measure',
POSITIVE_RATIO_MEASURE(7850.),#28534);
#28554=MEASURE_REPRESENTATION_ITEM('density measure',
POSITIVE_RATIO_MEASURE(7850.),#28535);
#28555=PROPERTY_DEFINITION_REPRESENTATION(#28650,#28593);
#28556=PROPERTY_DEFINITION_REPRESENTATION(#28651,#28594);
#28557=PROPERTY_DEFINITION_REPRESENTATION(#28652,#28595);
#28558=PROPERTY_DEFINITION_REPRESENTATION(#28653,#28596);
#28559=PROPERTY_DEFINITION_REPRESENTATION(#28654,#28597);
#28560=PROPERTY_DEFINITION_REPRESENTATION(#28655,#28598);
#28561=PROPERTY_DEFINITION_REPRESENTATION(#28656,#28599);
#28562=PROPERTY_DEFINITION_REPRESENTATION(#28657,#28600);
#28563=PROPERTY_DEFINITION_REPRESENTATION(#28658,#28601);
#28564=PROPERTY_DEFINITION_REPRESENTATION(#28659,#28602);
#28565=PROPERTY_DEFINITION_REPRESENTATION(#28660,#28603);
#28566=PROPERTY_DEFINITION_REPRESENTATION(#28661,#28604);
#28567=PROPERTY_DEFINITION_REPRESENTATION(#28662,#28605);
#28568=PROPERTY_DEFINITION_REPRESENTATION(#28663,#28606);
#28569=PROPERTY_DEFINITION_REPRESENTATION(#28664,#28607);
#28570=PROPERTY_DEFINITION_REPRESENTATION(#28665,#28608);
#28571=PROPERTY_DEFINITION_REPRESENTATION(#28666,#28609);
#28572=PROPERTY_DEFINITION_REPRESENTATION(#28667,#28610);
#28573=PROPERTY_DEFINITION_REPRESENTATION(#28668,#28611);
#28574=PROPERTY_DEFINITION_REPRESENTATION(#28669,#28612);
#28575=PROPERTY_DEFINITION_REPRESENTATION(#28670,#28613);
#28576=PROPERTY_DEFINITION_REPRESENTATION(#28671,#28614);
#28577=PROPERTY_DEFINITION_REPRESENTATION(#28672,#28615);
#28578=PROPERTY_DEFINITION_REPRESENTATION(#28673,#28616);
#28579=PROPERTY_DEFINITION_REPRESENTATION(#28674,#28617);
#28580=PROPERTY_DEFINITION_REPRESENTATION(#28675,#28618);
#28581=PROPERTY_DEFINITION_REPRESENTATION(#28676,#28619);
#28582=PROPERTY_DEFINITION_REPRESENTATION(#28677,#28620);
#28583=PROPERTY_DEFINITION_REPRESENTATION(#28678,#28621);
#28584=PROPERTY_DEFINITION_REPRESENTATION(#28679,#28622);
#28585=PROPERTY_DEFINITION_REPRESENTATION(#28680,#28623);
#28586=PROPERTY_DEFINITION_REPRESENTATION(#28681,#28624);
#28587=PROPERTY_DEFINITION_REPRESENTATION(#28682,#28625);
#28588=PROPERTY_DEFINITION_REPRESENTATION(#28683,#28626);
#28589=PROPERTY_DEFINITION_REPRESENTATION(#28684,#28627);
#28590=PROPERTY_DEFINITION_REPRESENTATION(#28685,#28628);
#28591=PROPERTY_DEFINITION_REPRESENTATION(#28686,#28629);
#28592=PROPERTY_DEFINITION_REPRESENTATION(#28687,#28630);
#28593=REPRESENTATION('material name',(#28631),#71473);
#28594=REPRESENTATION('density',(#28536),#71473);
#28595=REPRESENTATION('material name',(#28632),#71474);
#28596=REPRESENTATION('density',(#28537),#71474);
#28597=REPRESENTATION('material name',(#28633),#71475);
#28598=REPRESENTATION('density',(#28538),#71475);
#28599=REPRESENTATION('material name',(#28634),#71476);
#28600=REPRESENTATION('density',(#28539),#71476);
#28601=REPRESENTATION('material name',(#28635),#71477);
#28602=REPRESENTATION('density',(#28540),#71477);
#28603=REPRESENTATION('material name',(#28636),#71478);
#28604=REPRESENTATION('density',(#28541),#71478);
#28605=REPRESENTATION('material name',(#28637),#71479);
#28606=REPRESENTATION('density',(#28542),#71479);
#28607=REPRESENTATION('material name',(#28638),#71480);
#28608=REPRESENTATION('density',(#28543),#71480);
#28609=REPRESENTATION('material name',(#28639),#71481);
#28610=REPRESENTATION('density',(#28544),#71481);
#28611=REPRESENTATION('material name',(#28640),#71482);
#28612=REPRESENTATION('density',(#28545),#71482);
#28613=REPRESENTATION('material name',(#28641),#71483);
#28614=REPRESENTATION('density',(#28546),#71483);
#28615=REPRESENTATION('material name',(#28642),#71484);
#28616=REPRESENTATION('density',(#28547),#71484);
#28617=REPRESENTATION('material name',(#28643),#71485);
#28618=REPRESENTATION('density',(#28548),#71485);
#28619=REPRESENTATION('material name',(#28644),#71486);
#28620=REPRESENTATION('density',(#28549),#71486);
#28621=REPRESENTATION('material name',(#28645),#71487);
#28622=REPRESENTATION('density',(#28550),#71487);
#28623=REPRESENTATION('material name',(#28646),#71488);
#28624=REPRESENTATION('density',(#28551),#71488);
#28625=REPRESENTATION('material name',(#28647),#71489);
#28626=REPRESENTATION('density',(#28552),#71489);
#28627=REPRESENTATION('material name',(#28648),#71490);
#28628=REPRESENTATION('density',(#28553),#71490);
#28629=REPRESENTATION('material name',(#28649),#71491);
#28630=REPRESENTATION('density',(#28554),#71491);
#28631=DESCRIPTIVE_REPRESENTATION_ITEM('Steel','Steel');
#28632=DESCRIPTIVE_REPRESENTATION_ITEM('Steel','Steel');
#28633=DESCRIPTIVE_REPRESENTATION_ITEM('Steel','Steel');
#28634=DESCRIPTIVE_REPRESENTATION_ITEM('Steel','Steel');
#28635=DESCRIPTIVE_REPRESENTATION_ITEM('Steel','Steel');
#28636=DESCRIPTIVE_REPRESENTATION_ITEM('Steel','Steel');
#28637=DESCRIPTIVE_REPRESENTATION_ITEM('ABS Plastic','ABS Plastic');
#28638=DESCRIPTIVE_REPRESENTATION_ITEM('Steel','Steel');
#28639=DESCRIPTIVE_REPRESENTATION_ITEM('Steel','Steel');
#28640=DESCRIPTIVE_REPRESENTATION_ITEM('Steel','Steel');
#28641=DESCRIPTIVE_REPRESENTATION_ITEM('Steel','Steel');
#28642=DESCRIPTIVE_REPRESENTATION_ITEM('Steel','Steel');
#28643=DESCRIPTIVE_REPRESENTATION_ITEM('Steel','Steel');
#28644=DESCRIPTIVE_REPRESENTATION_ITEM('Steel','Steel');
#28645=DESCRIPTIVE_REPRESENTATION_ITEM('Steel','Steel');
#28646=DESCRIPTIVE_REPRESENTATION_ITEM('Steel','Steel');
#28647=DESCRIPTIVE_REPRESENTATION_ITEM('Steel','Steel');
#28648=DESCRIPTIVE_REPRESENTATION_ITEM('Steel','Steel');
#28649=DESCRIPTIVE_REPRESENTATION_ITEM('Steel','Steel');
#28650=PROPERTY_DEFINITION('material property','material name',#71624);
#28651=PROPERTY_DEFINITION('material property','density of part',#71624);
#28652=PROPERTY_DEFINITION('material property','material name',#71625);
#28653=PROPERTY_DEFINITION('material property','density of part',#71625);
#28654=PROPERTY_DEFINITION('material property','material name',#71626);
#28655=PROPERTY_DEFINITION('material property','density of part',#71626);
#28656=PROPERTY_DEFINITION('material property','material name',#71627);
#28657=PROPERTY_DEFINITION('material property','density of part',#71627);
#28658=PROPERTY_DEFINITION('material property','material name',#71628);
#28659=PROPERTY_DEFINITION('material property','density of part',#71628);
#28660=PROPERTY_DEFINITION('material property','material name',#71629);
#28661=PROPERTY_DEFINITION('material property','density of part',#71629);
#28662=PROPERTY_DEFINITION('material property','material name',#71630);
#28663=PROPERTY_DEFINITION('material property','density of part',#71630);
#28664=PROPERTY_DEFINITION('material property','material name',#71631);
#28665=PROPERTY_DEFINITION('material property','density of part',#71631);
#28666=PROPERTY_DEFINITION('material property','material name',#71632);
#28667=PROPERTY_DEFINITION('material property','density of part',#71632);
#28668=PROPERTY_DEFINITION('material property','material name',#71633);
#28669=PROPERTY_DEFINITION('material property','density of part',#71633);
#28670=PROPERTY_DEFINITION('material property','material name',#71634);
#28671=PROPERTY_DEFINITION('material property','density of part',#71634);
#28672=PROPERTY_DEFINITION('material property','material name',#71635);
#28673=PROPERTY_DEFINITION('material property','density of part',#71635);
#28674=PROPERTY_DEFINITION('material property','material name',#71636);
#28675=PROPERTY_DEFINITION('material property','density of part',#71636);
#28676=PROPERTY_DEFINITION('material property','material name',#71637);
#28677=PROPERTY_DEFINITION('material property','density of part',#71637);
#28678=PROPERTY_DEFINITION('material property','material name',#71638);
#28679=PROPERTY_DEFINITION('material property','density of part',#71638);
#28680=PROPERTY_DEFINITION('material property','material name',#71639);
#28681=PROPERTY_DEFINITION('material property','density of part',#71639);
#28682=PROPERTY_DEFINITION('material property','material name',#71640);
#28683=PROPERTY_DEFINITION('material property','density of part',#71640);
#28684=PROPERTY_DEFINITION('material property','material name',#71641);
#28685=PROPERTY_DEFINITION('material property','density of part',#71641);
#28686=PROPERTY_DEFINITION('material property','material name',#71642);
#28687=PROPERTY_DEFINITION('material property','density of part',#71642);
#28688=AXIS2_PLACEMENT_3D('',#37677,#30855,#30856);
#28689=AXIS2_PLACEMENT_3D('',#37678,#30857,#30858);
#28690=AXIS2_PLACEMENT_3D('',#37679,#30859,#30860);
#28691=AXIS2_PLACEMENT_3D('',#37690,#30866,#30867);
#28692=AXIS2_PLACEMENT_3D('',#37700,#30873,#30874);
#28693=AXIS2_PLACEMENT_3D('',#37704,#30877,#30878);
#28694=AXIS2_PLACEMENT_3D('',#37708,#30881,#30882);
#28695=AXIS2_PLACEMENT_3D('',#37712,#30885,#30886);
#28696=AXIS2_PLACEMENT_3D('',#37720,#30891,#30892);
#28697=AXIS2_PLACEMENT_3D('',#37732,#30899,#30900);
#28698=AXIS2_PLACEMENT_3D('',#37743,#30906,#30907);
#28699=AXIS2_PLACEMENT_3D('',#37749,#30911,#30912);
#28700=AXIS2_PLACEMENT_3D('',#37754,#30916,#30917);
#28701=AXIS2_PLACEMENT_3D('',#37757,#30920,#30921);
#28702=AXIS2_PLACEMENT_3D('',#37760,#30924,#30925);
#28703=AXIS2_PLACEMENT_3D('',#37764,#30928,#30929);
#28704=AXIS2_PLACEMENT_3D('',#37765,#30930,#30931);
#28705=AXIS2_PLACEMENT_3D('',#37767,#30932,#30933);
#28706=AXIS2_PLACEMENT_3D('',#37770,#30935,#30936);
#28707=AXIS2_PLACEMENT_3D('',#37771,#30937,#30938);
#28708=AXIS2_PLACEMENT_3D('',#37781,#30943,#30944);
#28709=AXIS2_PLACEMENT_3D('',#37783,#30945,#30946);
#28710=AXIS2_PLACEMENT_3D('',#37785,#30947,#30948);
#28711=AXIS2_PLACEMENT_3D('',#37786,#30949,#30950);
#28712=AXIS2_PLACEMENT_3D('',#37789,#30952,#30953);
#28713=AXIS2_PLACEMENT_3D('',#37790,#30954,#30955);
#28714=AXIS2_PLACEMENT_3D('',#37793,#30957,#30958);
#28715=AXIS2_PLACEMENT_3D('',#37794,#30959,#30960);
#28716=AXIS2_PLACEMENT_3D('',#37797,#30962,#30963);
#28717=AXIS2_PLACEMENT_3D('',#37798,#30964,#30965);
#28718=AXIS2_PLACEMENT_3D('',#37801,#30967,#30968);
#28719=AXIS2_PLACEMENT_3D('',#37802,#30969,#30970);
#28720=AXIS2_PLACEMENT_3D('',#37805,#30972,#30973);
#28721=AXIS2_PLACEMENT_3D('',#37806,#30974,#30975);
#28722=AXIS2_PLACEMENT_3D('',#37809,#30977,#30978);
#28723=AXIS2_PLACEMENT_3D('',#37810,#30979,#30980);
#28724=AXIS2_PLACEMENT_3D('',#37813,#30982,#30983);
#28725=AXIS2_PLACEMENT_3D('',#37814,#30984,#30985);
#28726=AXIS2_PLACEMENT_3D('',#37816,#30986,#30987);
#28727=AXIS2_PLACEMENT_3D('',#37818,#30989,#30990);
#28728=AXIS2_PLACEMENT_3D('',#37828,#30995,#30996);
#28729=AXIS2_PLACEMENT_3D('',#37830,#30997,#30998);
#28730=AXIS2_PLACEMENT_3D('',#37832,#30999,#31000);
#28731=AXIS2_PLACEMENT_3D('',#37833,#31001,#31002);
#28732=AXIS2_PLACEMENT_3D('',#37835,#31004,#31005);
#28733=AXIS2_PLACEMENT_3D('',#37837,#31007,#31008);
#28734=AXIS2_PLACEMENT_3D('',#37839,#31010,#31011);
#28735=AXIS2_PLACEMENT_3D('',#37841,#31012,#31013);
#28736=AXIS2_PLACEMENT_3D('',#37844,#31015,#31016);
#28737=AXIS2_PLACEMENT_3D('',#37845,#31017,#31018);
#28738=AXIS2_PLACEMENT_3D('',#37855,#31023,#31024);
#28739=AXIS2_PLACEMENT_3D('',#37857,#31025,#31026);
#28740=AXIS2_PLACEMENT_3D('',#37859,#31027,#31028);
#28741=AXIS2_PLACEMENT_3D('',#37860,#31029,#31030);
#28742=AXIS2_PLACEMENT_3D('',#37862,#31031,#31032);
#28743=AXIS2_PLACEMENT_3D('',#37864,#31034,#31035);
#28744=AXIS2_PLACEMENT_3D('',#37867,#31037,#31038);
#28745=AXIS2_PLACEMENT_3D('',#37868,#31039,#31040);
#28746=AXIS2_PLACEMENT_3D('',#37870,#31041,#31042);
#28747=AXIS2_PLACEMENT_3D('',#37872,#31044,#31045);
#28748=AXIS2_PLACEMENT_3D('',#37875,#31047,#31048);
#28749=AXIS2_PLACEMENT_3D('',#37876,#31049,#31050);
#28750=AXIS2_PLACEMENT_3D('',#37878,#31051,#31052);
#28751=AXIS2_PLACEMENT_3D('',#37880,#31054,#31055);
#28752=AXIS2_PLACEMENT_3D('',#37883,#31057,#31058);
#28753=AXIS2_PLACEMENT_3D('',#37884,#31059,#31060);
#28754=AXIS2_PLACEMENT_3D('',#37886,#31061,#31062);
#28755=AXIS2_PLACEMENT_3D('',#37888,#31064,#31065);
#28756=AXIS2_PLACEMENT_3D('',#37893,#31067,#31068);
#28757=AXIS2_PLACEMENT_3D('',#37895,#31069,#31070);
#28758=AXIS2_PLACEMENT_3D('',#37898,#31072,#31073);
#28759=AXIS2_PLACEMENT_3D('',#38007,#31076,#31077);
#28760=AXIS2_PLACEMENT_3D('',#38011,#31079,#31080);
#28761=AXIS2_PLACEMENT_3D('',#38015,#31082,#31083);
#28762=AXIS2_PLACEMENT_3D('',#38040,#31086,#31087);
#28763=AXIS2_PLACEMENT_3D('',#38044,#31089,#31090);
#28764=AXIS2_PLACEMENT_3D('',#38093,#31091,#31092);
#28765=AXIS2_PLACEMENT_3D('',#38094,#31093,#31094);
#28766=AXIS2_PLACEMENT_3D('',#38096,#31095,#31096);
#28767=AXIS2_PLACEMENT_3D('',#38098,#31098,#31099);
#28768=AXIS2_PLACEMENT_3D('',#38108,#31104,#31105);
#28769=AXIS2_PLACEMENT_3D('',#38110,#31106,#31107);
#28770=AXIS2_PLACEMENT_3D('',#38112,#31108,#31109);
#28771=AXIS2_PLACEMENT_3D('',#38113,#31110,#31111);
#28772=AXIS2_PLACEMENT_3D('',#38115,#31113,#31114);
#28773=AXIS2_PLACEMENT_3D('',#38117,#31116,#31117);
#28774=AXIS2_PLACEMENT_3D('',#38119,#31119,#31120);
#28775=AXIS2_PLACEMENT_3D('',#38124,#31122,#31123);
#28776=AXIS2_PLACEMENT_3D('',#38127,#31125,#31126);
#28777=AXIS2_PLACEMENT_3D('',#38128,#31127,#31128);
#28778=AXIS2_PLACEMENT_3D('',#38133,#31132,#31133);
#28779=AXIS2_PLACEMENT_3D('',#38136,#31135,#31136);
#28780=AXIS2_PLACEMENT_3D('',#38137,#31137,#31138);
#28781=AXIS2_PLACEMENT_3D('',#38143,#31142,#31143);
#28782=AXIS2_PLACEMENT_3D('',#38146,#31145,#31146);
#28783=AXIS2_PLACEMENT_3D('',#38147,#31147,#31148);
#28784=AXIS2_PLACEMENT_3D('',#38148,#31149,#31150);
#28785=AXIS2_PLACEMENT_3D('',#38152,#31153,#31154);
#28786=AXIS2_PLACEMENT_3D('',#38156,#31156,#31157);
#28787=AXIS2_PLACEMENT_3D('',#38157,#31158,#31159);
#28788=AXIS2_PLACEMENT_3D('',#38158,#31160,#31161);
#28789=AXIS2_PLACEMENT_3D('',#38161,#31164,#31165);
#28790=AXIS2_PLACEMENT_3D('',#38167,#31169,#31170);
#28791=AXIS2_PLACEMENT_3D('',#38168,#31171,#31172);
#28792=AXIS2_PLACEMENT_3D('',#38170,#31174,#31175);
#28793=AXIS2_PLACEMENT_3D('',#38221,#31179,#31180);
#28794=AXIS2_PLACEMENT_3D('',#38223,#31182,#31183);
#28795=AXIS2_PLACEMENT_3D('',#38228,#31185,#31186);
#28796=AXIS2_PLACEMENT_3D('',#38232,#31188,#31189);
#28797=AXIS2_PLACEMENT_3D('',#38236,#31191,#31192);
#28798=AXIS2_PLACEMENT_3D('',#38239,#31194,#31195);
#28799=AXIS2_PLACEMENT_3D('',#38240,#31196,#31197);
#28800=AXIS2_PLACEMENT_3D('',#38245,#31200,#31201);
#28801=AXIS2_PLACEMENT_3D('',#38246,#31202,#31203);
#28802=AXIS2_PLACEMENT_3D('',#38251,#31207,#31208);
#28803=AXIS2_PLACEMENT_3D('',#38254,#31210,#31211);
#28804=AXIS2_PLACEMENT_3D('',#38255,#31212,#31213);
#28805=AXIS2_PLACEMENT_3D('',#38259,#31216,#31217);
#28806=AXIS2_PLACEMENT_3D('',#38263,#31219,#31220);
#28807=AXIS2_PLACEMENT_3D('',#38264,#31221,#31222);
#28808=AXIS2_PLACEMENT_3D('',#38265,#31223,#31224);
#28809=AXIS2_PLACEMENT_3D('',#38270,#31228,#31229);
#28810=AXIS2_PLACEMENT_3D('',#38273,#31231,#31232);
#28811=AXIS2_PLACEMENT_3D('',#38274,#31233,#31234);
#28812=AXIS2_PLACEMENT_3D('',#38277,#31237,#31238);
#28813=AXIS2_PLACEMENT_3D('',#38279,#31240,#31241);
#28814=AXIS2_PLACEMENT_3D('',#38280,#31242,#31243);
#28815=AXIS2_PLACEMENT_3D('',#38281,#31244,#31245);
#28816=AXIS2_PLACEMENT_3D('',#38282,#31246,#31247);
#28817=AXIS2_PLACEMENT_3D('',#38491,#31270,#31271);
#28818=AXIS2_PLACEMENT_3D('',#38496,#31273,#31274);
#28819=AXIS2_PLACEMENT_3D('',#38500,#31276,#31277);
#28820=AXIS2_PLACEMENT_3D('',#38504,#31279,#31280);
#28821=AXIS2_PLACEMENT_3D('',#38507,#31282,#31283);
#28822=AXIS2_PLACEMENT_3D('',#38508,#31284,#31285);
#28823=AXIS2_PLACEMENT_3D('',#38512,#31287,#31288);
#28824=AXIS2_PLACEMENT_3D('',#38514,#31289,#31290);
#28825=AXIS2_PLACEMENT_3D('',#38615,#31294,#31295);
#28826=AXIS2_PLACEMENT_3D('',#38619,#31297,#31298);
#28827=AXIS2_PLACEMENT_3D('',#38662,#31299,#31300);
#28828=AXIS2_PLACEMENT_3D('',#38663,#31301,#31302);
#28829=AXIS2_PLACEMENT_3D('',#38667,#31304,#31305);
#28830=AXIS2_PLACEMENT_3D('',#38669,#31306,#31307);
#28831=AXIS2_PLACEMENT_3D('',#38765,#31311,#31312);
#28832=AXIS2_PLACEMENT_3D('',#38769,#31314,#31315);
#28833=AXIS2_PLACEMENT_3D('',#38818,#31316,#31317);
#28834=AXIS2_PLACEMENT_3D('',#38819,#31318,#31319);
#28835=AXIS2_PLACEMENT_3D('',#38825,#31323,#31324);
#28836=AXIS2_PLACEMENT_3D('',#38828,#31326,#31327);
#28837=AXIS2_PLACEMENT_3D('',#38829,#31328,#31329);
#28838=AXIS2_PLACEMENT_3D('',#38833,#31332,#31333);
#28839=AXIS2_PLACEMENT_3D('',#38835,#31335,#31336);
#28840=AXIS2_PLACEMENT_3D('',#38836,#31337,#31338);
#28841=AXIS2_PLACEMENT_3D('',#38838,#31340,#31341);
#28842=AXIS2_PLACEMENT_3D('',#38841,#31343,#31344);
#28843=AXIS2_PLACEMENT_3D('',#38842,#31345,#31346);
#28844=AXIS2_PLACEMENT_3D('',#38846,#31349,#31350);
#28845=AXIS2_PLACEMENT_3D('',#38847,#31351,#31352);
#28846=AXIS2_PLACEMENT_3D('',#38848,#31353,#31354);
#28847=AXIS2_PLACEMENT_3D('',#38851,#31356,#31357);
#28848=AXIS2_PLACEMENT_3D('',#38852,#31358,#31359);
#28849=AXIS2_PLACEMENT_3D('',#38856,#31362,#31363);
#28850=AXIS2_PLACEMENT_3D('',#38957,#31367,#31368);
#28851=AXIS2_PLACEMENT_3D('',#38958,#31369,#31370);
#28852=AXIS2_PLACEMENT_3D('',#38962,#31372,#31373);
#28853=AXIS2_PLACEMENT_3D('',#38966,#31375,#31376);
#28854=AXIS2_PLACEMENT_3D('',#38970,#31379,#31380);
#28855=AXIS2_PLACEMENT_3D('',#38971,#31381,#31382);
#28856=AXIS2_PLACEMENT_3D('',#39054,#31385,#31386);
#28857=AXIS2_PLACEMENT_3D('',#39089,#31389,#31390);
#28858=AXIS2_PLACEMENT_3D('',#39092,#31393,#31394);
#28859=AXIS2_PLACEMENT_3D('',#39094,#31395,#31396);
#28860=AXIS2_PLACEMENT_3D('',#39096,#31398,#31399);
#28861=AXIS2_PLACEMENT_3D('',#39100,#31402,#31403);
#28862=AXIS2_PLACEMENT_3D('',#39101,#31404,#31405);
#28863=AXIS2_PLACEMENT_3D('',#39103,#31407,#31408);
#28864=AXIS2_PLACEMENT_3D('',#39105,#31410,#31411);
#28865=AXIS2_PLACEMENT_3D('',#39107,#31413,#31414);
#28866=AXIS2_PLACEMENT_3D('',#39109,#31416,#31417);
#28867=AXIS2_PLACEMENT_3D('',#39110,#31418,#31419);
#28868=AXIS2_PLACEMENT_3D('',#39112,#31421,#31422);
#28869=AXIS2_PLACEMENT_3D('',#39114,#31424,#31425);
#28870=AXIS2_PLACEMENT_3D('',#39300,#31428,#31429);
#28871=AXIS2_PLACEMENT_3D('',#39433,#31434,#31435);
#28872=AXIS2_PLACEMENT_3D('',#39468,#31438,#31439);
#28873=AXIS2_PLACEMENT_3D('',#39472,#31441,#31442);
#28874=AXIS2_PLACEMENT_3D('',#39474,#31443,#31444);
#28875=AXIS2_PLACEMENT_3D('',#39570,#31448,#31449);
#28876=AXIS2_PLACEMENT_3D('',#39574,#31451,#31452);
#28877=AXIS2_PLACEMENT_3D('',#39617,#31453,#31454);
#28878=AXIS2_PLACEMENT_3D('',#39692,#31457,#31458);
#28879=AXIS2_PLACEMENT_3D('',#39727,#31461,#31462);
#28880=AXIS2_PLACEMENT_3D('',#39732,#31464,#31465);
#28881=AXIS2_PLACEMENT_3D('',#39735,#31467,#31468);
#28882=AXIS2_PLACEMENT_3D('',#39736,#31469,#31470);
#28883=AXIS2_PLACEMENT_3D('',#39742,#31474,#31475);
#28884=AXIS2_PLACEMENT_3D('',#39746,#31477,#31478);
#28885=AXIS2_PLACEMENT_3D('',#39747,#31479,#31480);
#28886=AXIS2_PLACEMENT_3D('',#39748,#31481,#31482);
#28887=AXIS2_PLACEMENT_3D('',#39754,#31486,#31487);
#28888=AXIS2_PLACEMENT_3D('',#39757,#31489,#31490);
#28889=AXIS2_PLACEMENT_3D('',#39758,#31491,#31492);
#28890=AXIS2_PLACEMENT_3D('',#39759,#31493,#31494);
#28891=AXIS2_PLACEMENT_3D('',#39763,#31497,#31498);
#28892=AXIS2_PLACEMENT_3D('',#39767,#31500,#31501);
#28893=AXIS2_PLACEMENT_3D('',#39768,#31502,#31503);
#28894=AXIS2_PLACEMENT_3D('',#39769,#31504,#31505);
#28895=AXIS2_PLACEMENT_3D('',#39772,#31508,#31509);
#28896=AXIS2_PLACEMENT_3D('',#39778,#31513,#31514);
#28897=AXIS2_PLACEMENT_3D('',#39779,#31515,#31516);
#28898=AXIS2_PLACEMENT_3D('',#39783,#31519,#31520);
#28899=AXIS2_PLACEMENT_3D('',#39833,#31524,#31525);
#28900=AXIS2_PLACEMENT_3D('',#39836,#31528,#31529);
#28901=AXIS2_PLACEMENT_3D('',#39841,#31531,#31532);
#28902=AXIS2_PLACEMENT_3D('',#39845,#31534,#31535);
#28903=AXIS2_PLACEMENT_3D('',#39849,#31537,#31538);
#28904=AXIS2_PLACEMENT_3D('',#39852,#31540,#31541);
#28905=AXIS2_PLACEMENT_3D('',#39853,#31542,#31543);
#28906=AXIS2_PLACEMENT_3D('',#39858,#31546,#31547);
#28907=AXIS2_PLACEMENT_3D('',#39859,#31548,#31549);
#28908=AXIS2_PLACEMENT_3D('',#39864,#31553,#31554);
#28909=AXIS2_PLACEMENT_3D('',#39867,#31556,#31557);
#28910=AXIS2_PLACEMENT_3D('',#39868,#31558,#31559);
#28911=AXIS2_PLACEMENT_3D('',#39872,#31562,#31563);
#28912=AXIS2_PLACEMENT_3D('',#39876,#31565,#31566);
#28913=AXIS2_PLACEMENT_3D('',#39877,#31567,#31568);
#28914=AXIS2_PLACEMENT_3D('',#39878,#31569,#31570);
#28915=AXIS2_PLACEMENT_3D('',#39884,#31574,#31575);
#28916=AXIS2_PLACEMENT_3D('',#39888,#31577,#31578);
#28917=AXIS2_PLACEMENT_3D('',#39889,#31579,#31580);
#28918=AXIS2_PLACEMENT_3D('',#39890,#31581,#31582);
#28919=AXIS2_PLACEMENT_3D('',#39893,#31585,#31586);
#28920=AXIS2_PLACEMENT_3D('',#39896,#31589,#31590);
#28921=AXIS2_PLACEMENT_3D('',#39945,#31594,#31595);
#28922=AXIS2_PLACEMENT_3D('',#39946,#31596,#31597);
#28923=AXIS2_PLACEMENT_3D('',#39947,#31598,#31599);
#28924=AXIS2_PLACEMENT_3D('',#39948,#31600,#31601);
#28925=AXIS2_PLACEMENT_3D('',#39949,#31602,#31603);
#28926=AXIS2_PLACEMENT_3D('',#39950,#31604,#31605);
#28927=AXIS2_PLACEMENT_3D('',#39955,#31607,#31608);
#28928=AXIS2_PLACEMENT_3D('',#39959,#31610,#31611);
#28929=AXIS2_PLACEMENT_3D('',#39963,#31613,#31614);
#28930=AXIS2_PLACEMENT_3D('',#39966,#31616,#31617);
#28931=AXIS2_PLACEMENT_3D('',#40021,#31620,#31621);
#28932=AXIS2_PLACEMENT_3D('',#40025,#31623,#31624);
#28933=AXIS2_PLACEMENT_3D('',#40027,#31625,#31626);
#28934=AXIS2_PLACEMENT_3D('',#40069,#31628,#31629);
#28935=AXIS2_PLACEMENT_3D('',#40073,#31631,#31632);
#28936=AXIS2_PLACEMENT_3D('',#40119,#31633,#31634);
#28937=AXIS2_PLACEMENT_3D('',#40120,#31635,#31636);
#28938=AXIS2_PLACEMENT_3D('',#40126,#31640,#31641);
#28939=AXIS2_PLACEMENT_3D('',#40128,#31642,#31643);
#28940=AXIS2_PLACEMENT_3D('',#40130,#31645,#31646);
#28941=AXIS2_PLACEMENT_3D('',#40134,#31649,#31650);
#28942=AXIS2_PLACEMENT_3D('',#40135,#31651,#31652);
#28943=AXIS2_PLACEMENT_3D('',#40137,#31654,#31655);
#28944=AXIS2_PLACEMENT_3D('',#40139,#31657,#31658);
#28945=AXIS2_PLACEMENT_3D('',#40141,#31659,#31660);
#28946=AXIS2_PLACEMENT_3D('',#40143,#31662,#31663);
#28947=AXIS2_PLACEMENT_3D('',#40147,#31666,#31667);
#28948=AXIS2_PLACEMENT_3D('',#40148,#31668,#31669);
#28949=AXIS2_PLACEMENT_3D('',#40149,#31670,#31671);
#28950=AXIS2_PLACEMENT_3D('',#40152,#31673,#31674);
#28951=AXIS2_PLACEMENT_3D('',#40153,#31675,#31676);
#28952=AXIS2_PLACEMENT_3D('',#40157,#31679,#31680);
#28953=AXIS2_PLACEMENT_3D('',#40255,#31684,#31685);
#28954=AXIS2_PLACEMENT_3D('',#40256,#31686,#31687);
#28955=AXIS2_PLACEMENT_3D('',#40260,#31689,#31690);
#28956=AXIS2_PLACEMENT_3D('',#40264,#31692,#31693);
#28957=AXIS2_PLACEMENT_3D('',#40268,#31696,#31697);
#28958=AXIS2_PLACEMENT_3D('',#40269,#31698,#31699);
#28959=AXIS2_PLACEMENT_3D('',#40270,#31700,#31701);
#28960=AXIS2_PLACEMENT_3D('',#40273,#31704,#31705);
#28961=AXIS2_PLACEMENT_3D('',#40275,#31707,#31708);
#28962=AXIS2_PLACEMENT_3D('',#40277,#31710,#31711);
#28963=AXIS2_PLACEMENT_3D('',#40279,#31713,#31714);
#28964=AXIS2_PLACEMENT_3D('',#40281,#31716,#31717);
#28965=AXIS2_PLACEMENT_3D('',#40284,#31719,#31720);
#28966=AXIS2_PLACEMENT_3D('',#40285,#31721,#31722);
#28967=AXIS2_PLACEMENT_3D('',#40289,#31725,#31726);
#28968=AXIS2_PLACEMENT_3D('',#40290,#31727,#31728);
#28969=AXIS2_PLACEMENT_3D('',#40291,#31729,#31730);
#28970=AXIS2_PLACEMENT_3D('',#40293,#31732,#31733);
#28971=AXIS2_PLACEMENT_3D('',#40295,#31735,#31736);
#28972=AXIS2_PLACEMENT_3D('',#40468,#31739,#31740);
#28973=AXIS2_PLACEMENT_3D('',#40503,#31743,#31744);
#28974=AXIS2_PLACEMENT_3D('',#40507,#31746,#31747);
#28975=AXIS2_PLACEMENT_3D('',#40509,#31748,#31749);
#28976=AXIS2_PLACEMENT_3D('',#40605,#31753,#31754);
#28977=AXIS2_PLACEMENT_3D('',#40609,#31756,#31757);
#28978=AXIS2_PLACEMENT_3D('',#40652,#31758,#31759);
#28979=AXIS2_PLACEMENT_3D('',#40735,#31762,#31763);
#28980=AXIS2_PLACEMENT_3D('',#40829,#31768,#31769);
#28981=AXIS2_PLACEMENT_3D('',#40833,#31771,#31772);
#28982=AXIS2_PLACEMENT_3D('',#40835,#31773,#31774);
#28983=AXIS2_PLACEMENT_3D('',#40877,#31776,#31777);
#28984=AXIS2_PLACEMENT_3D('',#40881,#31779,#31780);
#28985=AXIS2_PLACEMENT_3D('',#40924,#31781,#31782);
#28986=AXIS2_PLACEMENT_3D('',#41011,#31785,#31786);
#28987=AXIS2_PLACEMENT_3D('',#41046,#31789,#31790);
#28988=AXIS2_PLACEMENT_3D('',#41050,#31792,#31793);
#28989=AXIS2_PLACEMENT_3D('',#41052,#31794,#31795);
#28990=AXIS2_PLACEMENT_3D('',#41148,#31799,#31800);
#28991=AXIS2_PLACEMENT_3D('',#41152,#31802,#31803);
#28992=AXIS2_PLACEMENT_3D('',#41195,#31804,#31805);
#28993=AXIS2_PLACEMENT_3D('',#41278,#31808,#31809);
#28994=AXIS2_PLACEMENT_3D('',#41313,#31812,#31813);
#28995=AXIS2_PLACEMENT_3D('',#41315,#31814,#31815);
#28996=AXIS2_PLACEMENT_3D('',#41318,#31817,#31818);
#28997=AXIS2_PLACEMENT_3D('',#41319,#31819,#31820);
#28998=AXIS2_PLACEMENT_3D('',#41322,#31822,#31823);
#28999=AXIS2_PLACEMENT_3D('',#41323,#31824,#31825);
#29000=AXIS2_PLACEMENT_3D('',#41325,#31826,#31827);
#29001=AXIS2_PLACEMENT_3D('',#41326,#31828,#31829);
#29002=AXIS2_PLACEMENT_3D('',#41328,#31830,#31831);
#29003=AXIS2_PLACEMENT_3D('',#41330,#31833,#31834);
#29004=AXIS2_PLACEMENT_3D('',#41333,#31836,#31837);
#29005=AXIS2_PLACEMENT_3D('',#41334,#31838,#31839);
#29006=AXIS2_PLACEMENT_3D('',#41337,#31841,#31842);
#29007=AXIS2_PLACEMENT_3D('',#41338,#31843,#31844);
#29008=AXIS2_PLACEMENT_3D('',#41341,#31846,#31847);
#29009=AXIS2_PLACEMENT_3D('',#41342,#31848,#31849);
#29010=AXIS2_PLACEMENT_3D('',#41574,#31869,#31870);
#29011=AXIS2_PLACEMENT_3D('',#41575,#31871,#31872);
#29012=AXIS2_PLACEMENT_3D('',#41581,#31876,#31877);
#29013=AXIS2_PLACEMENT_3D('',#41585,#31880,#31881);
#29014=AXIS2_PLACEMENT_3D('',#41589,#31884,#31885);
#29015=AXIS2_PLACEMENT_3D('',#41593,#31888,#31889);
#29016=AXIS2_PLACEMENT_3D('',#41597,#31892,#31893);
#29017=AXIS2_PLACEMENT_3D('',#41601,#31896,#31897);
#29018=AXIS2_PLACEMENT_3D('',#41605,#31900,#31901);
#29019=AXIS2_PLACEMENT_3D('',#41607,#31903,#31904);
#29020=AXIS2_PLACEMENT_3D('',#41886,#31927,#31928);
#29021=AXIS2_PLACEMENT_3D('',#41887,#31929,#31930);
#29022=AXIS2_PLACEMENT_3D('',#42003,#31944,#31945);
#29023=AXIS2_PLACEMENT_3D('',#42095,#31956,#31957);
#29024=AXIS2_PLACEMENT_3D('',#42099,#31960,#31961);
#29025=AXIS2_PLACEMENT_3D('',#42101,#31963,#31964);
#29026=AXIS2_PLACEMENT_3D('',#42102,#31965,#31966);
#29027=AXIS2_PLACEMENT_3D('',#42108,#31970,#31971);
#29028=AXIS2_PLACEMENT_3D('',#42112,#31974,#31975);
#29029=AXIS2_PLACEMENT_3D('',#42116,#31978,#31979);
#29030=AXIS2_PLACEMENT_3D('',#42120,#31982,#31983);
#29031=AXIS2_PLACEMENT_3D('',#42124,#31986,#31987);
#29032=AXIS2_PLACEMENT_3D('',#42128,#31990,#31991);
#29033=AXIS2_PLACEMENT_3D('',#42132,#31994,#31995);
#29034=AXIS2_PLACEMENT_3D('',#42136,#31998,#31999);
#29035=AXIS2_PLACEMENT_3D('',#42140,#32002,#32003);
#29036=AXIS2_PLACEMENT_3D('',#42142,#32005,#32006);
#29037=AXIS2_PLACEMENT_3D('',#42143,#32007,#32008);
#29038=AXIS2_PLACEMENT_3D('',#42144,#32009,#32010);
#29039=AXIS2_PLACEMENT_3D('',#42145,#32011,#32012);
#29040=AXIS2_PLACEMENT_3D('',#42147,#32014,#32015);
#29041=AXIS2_PLACEMENT_3D('',#42149,#32017,#32018);
#29042=AXIS2_PLACEMENT_3D('',#42150,#32019,#32020);
#29043=AXIS2_PLACEMENT_3D('',#42151,#32021,#32022);
#29044=AXIS2_PLACEMENT_3D('',#42152,#32023,#32024);
#29045=AXIS2_PLACEMENT_3D('',#42153,#32025,#32026);
#29046=AXIS2_PLACEMENT_3D('',#42154,#32027,#32028);
#29047=AXIS2_PLACEMENT_3D('',#42163,#32033,#32034);
#29048=AXIS2_PLACEMENT_3D('',#42171,#32039,#32040);
#29049=AXIS2_PLACEMENT_3D('',#42177,#32044,#32045);
#29050=AXIS2_PLACEMENT_3D('',#42181,#32048,#32049);
#29051=AXIS2_PLACEMENT_3D('',#42189,#32054,#32055);
#29052=AXIS2_PLACEMENT_3D('',#42200,#32061,#32062);
#29053=AXIS2_PLACEMENT_3D('',#42206,#32066,#32067);
#29054=AXIS2_PLACEMENT_3D('',#42214,#32072,#32073);
#29055=AXIS2_PLACEMENT_3D('',#42224,#32079,#32080);
#29056=AXIS2_PLACEMENT_3D('',#42228,#32083,#32084);
#29057=AXIS2_PLACEMENT_3D('',#42232,#32087,#32088);
#29058=AXIS2_PLACEMENT_3D('',#42236,#32091,#32092);
#29059=AXIS2_PLACEMENT_3D('',#42244,#32097,#32098);
#29060=AXIS2_PLACEMENT_3D('',#42257,#32105,#32106);
#29061=AXIS2_PLACEMENT_3D('',#42265,#32111,#32112);
#29062=AXIS2_PLACEMENT_3D('',#42273,#32117,#32118);
#29063=AXIS2_PLACEMENT_3D('',#42280,#32123,#32124);
#29064=AXIS2_PLACEMENT_3D('',#42291,#32130,#32131);
#29065=AXIS2_PLACEMENT_3D('',#42299,#32136,#32137);
#29066=AXIS2_PLACEMENT_3D('',#42306,#32142,#32143);
#29067=AXIS2_PLACEMENT_3D('',#42314,#32148,#32149);
#29068=AXIS2_PLACEMENT_3D('',#42322,#32154,#32155);
#29069=AXIS2_PLACEMENT_3D('',#42326,#32158,#32159);
#29070=AXIS2_PLACEMENT_3D('',#42332,#32163,#32164);
#29071=AXIS2_PLACEMENT_3D('',#42338,#32168,#32169);
#29072=AXIS2_PLACEMENT_3D('',#42343,#32173,#32174);
#29073=AXIS2_PLACEMENT_3D('',#42351,#32179,#32180);
#29074=AXIS2_PLACEMENT_3D('',#42363,#32187,#32188);
#29075=AXIS2_PLACEMENT_3D('',#42369,#32192,#32193);
#29076=AXIS2_PLACEMENT_3D('',#42375,#32197,#32198);
#29077=AXIS2_PLACEMENT_3D('',#42379,#32201,#32202);
#29078=AXIS2_PLACEMENT_3D('',#42383,#32205,#32206);
#29079=AXIS2_PLACEMENT_3D('',#42399,#32215,#32216);
#29080=AXIS2_PLACEMENT_3D('',#42405,#32220,#32221);
#29081=AXIS2_PLACEMENT_3D('',#42409,#32224,#32225);
#29082=AXIS2_PLACEMENT_3D('',#42417,#32230,#32231);
#29083=AXIS2_PLACEMENT_3D('',#42423,#32235,#32236);
#29084=AXIS2_PLACEMENT_3D('',#42427,#32239,#32240);
#29085=AXIS2_PLACEMENT_3D('',#42435,#32245,#32246);
#29086=AXIS2_PLACEMENT_3D('',#42438,#32249,#32250);
#29087=AXIS2_PLACEMENT_3D('',#42462,#32263,#32264);
#29088=AXIS2_PLACEMENT_3D('',#42470,#32269,#32270);
#29089=AXIS2_PLACEMENT_3D('',#42480,#32276,#32277);
#29090=AXIS2_PLACEMENT_3D('',#42486,#32281,#32282);
#29091=AXIS2_PLACEMENT_3D('',#42494,#32287,#32288);
#29092=AXIS2_PLACEMENT_3D('',#42500,#32292,#32293);
#29093=AXIS2_PLACEMENT_3D('',#42506,#32297,#32298);
#29094=AXIS2_PLACEMENT_3D('',#42514,#32303,#32304);
#29095=AXIS2_PLACEMENT_3D('',#42520,#32308,#32309);
#29096=AXIS2_PLACEMENT_3D('',#42533,#32317,#32318);
#29097=AXIS2_PLACEMENT_3D('',#42537,#32321,#32322);
#29098=AXIS2_PLACEMENT_3D('',#42540,#32325,#32326);
#29099=AXIS2_PLACEMENT_3D('',#42546,#32330,#32331);
#29100=AXIS2_PLACEMENT_3D('',#42550,#32334,#32335);
#29101=AXIS2_PLACEMENT_3D('',#42552,#32337,#32338);
#29102=AXIS2_PLACEMENT_3D('',#42554,#32340,#32341);
#29103=AXIS2_PLACEMENT_3D('',#42558,#32344,#32345);
#29104=AXIS2_PLACEMENT_3D('',#42559,#32346,#32347);
#29105=AXIS2_PLACEMENT_3D('',#42563,#32350,#32351);
#29106=AXIS2_PLACEMENT_3D('',#42567,#32354,#32355);
#29107=AXIS2_PLACEMENT_3D('',#42577,#32361,#32362);
#29108=AXIS2_PLACEMENT_3D('',#42580,#32365,#32366);
#29109=AXIS2_PLACEMENT_3D('',#42583,#32369,#32370);
#29110=AXIS2_PLACEMENT_3D('',#42585,#32372,#32373);
#29111=AXIS2_PLACEMENT_3D('',#42588,#32376,#32377);
#29112=AXIS2_PLACEMENT_3D('',#42589,#32378,#32379);
#29113=AXIS2_PLACEMENT_3D('',#42593,#32382,#32383);
#29114=AXIS2_PLACEMENT_3D('',#42599,#32387,#32388);
#29115=AXIS2_PLACEMENT_3D('',#42610,#32395,#32396);
#29116=AXIS2_PLACEMENT_3D('',#42616,#32400,#32401);
#29117=AXIS2_PLACEMENT_3D('',#42621,#32404,#32405);
#29118=AXIS2_PLACEMENT_3D('',#42623,#32406,#32407);
#29119=AXIS2_PLACEMENT_3D('',#42624,#32408,#32409);
#29120=AXIS2_PLACEMENT_3D('',#42635,#32415,#32416);
#29121=AXIS2_PLACEMENT_3D('',#42647,#32425,#32426);
#29122=AXIS2_PLACEMENT_3D('',#42653,#32430,#32431);
#29123=AXIS2_PLACEMENT_3D('',#42656,#32434,#32435);
#29124=AXIS2_PLACEMENT_3D('',#42657,#32436,#32437);
#29125=AXIS2_PLACEMENT_3D('',#42658,#32438,#32439);
#29126=AXIS2_PLACEMENT_3D('',#42663,#32443,#32444);
#29127=AXIS2_PLACEMENT_3D('',#42664,#32445,#32446);
#29128=AXIS2_PLACEMENT_3D('',#42668,#32449,#32450);
#29129=AXIS2_PLACEMENT_3D('',#42674,#32454,#32455);
#29130=AXIS2_PLACEMENT_3D('',#42676,#32457,#32458);
#29131=AXIS2_PLACEMENT_3D('',#42680,#32461,#32462);
#29132=AXIS2_PLACEMENT_3D('',#42686,#32466,#32467);
#29133=AXIS2_PLACEMENT_3D('',#42690,#32470,#32471);
#29134=AXIS2_PLACEMENT_3D('',#42692,#32473,#32474);
#29135=AXIS2_PLACEMENT_3D('',#42696,#32477,#32478);
#29136=AXIS2_PLACEMENT_3D('',#42698,#32480,#32481);
#29137=AXIS2_PLACEMENT_3D('',#42702,#32484,#32485);
#29138=AXIS2_PLACEMENT_3D('',#42708,#32489,#32490);
#29139=AXIS2_PLACEMENT_3D('',#42715,#32495,#32496);
#29140=AXIS2_PLACEMENT_3D('',#42716,#32497,#32498);
#29141=AXIS2_PLACEMENT_3D('',#42723,#32503,#32504);
#29142=AXIS2_PLACEMENT_3D('',#42727,#32507,#32508);
#29143=AXIS2_PLACEMENT_3D('',#42731,#32511,#32512);
#29144=AXIS2_PLACEMENT_3D('',#42737,#32516,#32517);
#29145=AXIS2_PLACEMENT_3D('',#42739,#32519,#32520);
#29146=AXIS2_PLACEMENT_3D('',#42741,#32522,#32523);
#29147=AXIS2_PLACEMENT_3D('',#42742,#32524,#32525);
#29148=AXIS2_PLACEMENT_3D('',#42745,#32526,#32527);
#29149=AXIS2_PLACEMENT_3D('',#42746,#32528,#32529);
#29150=AXIS2_PLACEMENT_3D('',#42750,#32531,#32532);
#29151=AXIS2_PLACEMENT_3D('',#42751,#32533,#32534);
#29152=AXIS2_PLACEMENT_3D('',#42752,#32535,#32536);
#29153=AXIS2_PLACEMENT_3D('',#42756,#32538,#32539);
#29154=AXIS2_PLACEMENT_3D('',#42757,#32540,#32541);
#29155=AXIS2_PLACEMENT_3D('',#42758,#32542,#32543);
#29156=AXIS2_PLACEMENT_3D('',#42760,#32544,#32545);
#29157=AXIS2_PLACEMENT_3D('',#42762,#32547,#32548);
#29158=AXIS2_PLACEMENT_3D('',#42765,#32550,#32551);
#29159=AXIS2_PLACEMENT_3D('',#42766,#32552,#32553);
#29160=AXIS2_PLACEMENT_3D('',#42767,#32554,#32555);
#29161=AXIS2_PLACEMENT_3D('',#42770,#32557,#32558);
#29162=AXIS2_PLACEMENT_3D('',#42771,#32559,#32560);
#29163=AXIS2_PLACEMENT_3D('',#42774,#32562,#32563);
#29164=AXIS2_PLACEMENT_3D('',#42775,#32564,#32565);
#29165=AXIS2_PLACEMENT_3D('',#42777,#32566,#32567);
#29166=AXIS2_PLACEMENT_3D('',#42779,#32569,#32570);
#29167=AXIS2_PLACEMENT_3D('',#42781,#32571,#32572);
#29168=AXIS2_PLACEMENT_3D('',#42782,#32573,#32574);
#29169=AXIS2_PLACEMENT_3D('',#42785,#32576,#32577);
#29170=AXIS2_PLACEMENT_3D('',#42786,#32578,#32579);
#29171=AXIS2_PLACEMENT_3D('',#42789,#32581,#32582);
#29172=AXIS2_PLACEMENT_3D('',#42790,#32583,#32584);
#29173=AXIS2_PLACEMENT_3D('',#42792,#32586,#32587);
#29174=AXIS2_PLACEMENT_3D('',#42794,#32588,#32589);
#29175=AXIS2_PLACEMENT_3D('',#42796,#32591,#32592);
#29176=AXIS2_PLACEMENT_3D('',#42797,#32593,#32594);
#29177=AXIS2_PLACEMENT_3D('',#42798,#32595,#32596);
#29178=AXIS2_PLACEMENT_3D('',#42799,#32597,#32598);
#29179=AXIS2_PLACEMENT_3D('',#42800,#32599,#32600);
#29180=AXIS2_PLACEMENT_3D('',#42802,#32602,#32603);
#29181=AXIS2_PLACEMENT_3D('',#42803,#32604,#32605);
#29182=AXIS2_PLACEMENT_3D('',#42804,#32606,#32607);
#29183=AXIS2_PLACEMENT_3D('',#42813,#32612,#32613);
#29184=AXIS2_PLACEMENT_3D('',#42819,#32617,#32618);
#29185=AXIS2_PLACEMENT_3D('',#42832,#32625,#32626);
#29186=AXIS2_PLACEMENT_3D('',#42838,#32630,#32631);
#29187=AXIS2_PLACEMENT_3D('',#42846,#32636,#32637);
#29188=AXIS2_PLACEMENT_3D('',#42854,#32642,#32643);
#29189=AXIS2_PLACEMENT_3D('',#42863,#32648,#32649);
#29190=AXIS2_PLACEMENT_3D('',#42866,#32652,#32653);
#29191=AXIS2_PLACEMENT_3D('',#42875,#32658,#32659);
#29192=AXIS2_PLACEMENT_3D('',#42881,#32663,#32664);
#29193=AXIS2_PLACEMENT_3D('',#42894,#32671,#32672);
#29194=AXIS2_PLACEMENT_3D('',#42904,#32678,#32679);
#29195=AXIS2_PLACEMENT_3D('',#42908,#32682,#32683);
#29196=AXIS2_PLACEMENT_3D('',#42916,#32688,#32689);
#29197=AXIS2_PLACEMENT_3D('',#42922,#32693,#32694);
#29198=AXIS2_PLACEMENT_3D('',#42928,#32698,#32699);
#29199=AXIS2_PLACEMENT_3D('',#42932,#32702,#32703);
#29200=AXIS2_PLACEMENT_3D('',#42938,#32707,#32708);
#29201=AXIS2_PLACEMENT_3D('',#42944,#32712,#32713);
#29202=AXIS2_PLACEMENT_3D('',#42950,#32717,#32718);
#29203=AXIS2_PLACEMENT_3D('',#42954,#32721,#32722);
#29204=AXIS2_PLACEMENT_3D('',#42958,#32725,#32726);
#29205=AXIS2_PLACEMENT_3D('',#42967,#32731,#32732);
#29206=AXIS2_PLACEMENT_3D('',#42970,#32735,#32736);
#29207=AXIS2_PLACEMENT_3D('',#42974,#32739,#32740);
#29208=AXIS2_PLACEMENT_3D('',#42978,#32743,#32744);
#29209=AXIS2_PLACEMENT_3D('',#42985,#32748,#32749);
#29210=AXIS2_PLACEMENT_3D('',#42990,#32753,#32754);
#29211=AXIS2_PLACEMENT_3D('',#42995,#32758,#32759);
#29212=AXIS2_PLACEMENT_3D('',#43000,#32763,#32764);
#29213=AXIS2_PLACEMENT_3D('',#43004,#32767,#32768);
#29214=AXIS2_PLACEMENT_3D('',#43007,#32771,#32772);
#29215=AXIS2_PLACEMENT_3D('',#43012,#32776,#32777);
#29216=AXIS2_PLACEMENT_3D('',#43036,#32790,#32791);
#29217=AXIS2_PLACEMENT_3D('',#43044,#32796,#32797);
#29218=AXIS2_PLACEMENT_3D('',#43049,#32801,#32802);
#29219=AXIS2_PLACEMENT_3D('',#43053,#32805,#32806);
#29220=AXIS2_PLACEMENT_3D('',#43057,#32809,#32810);
#29221=AXIS2_PLACEMENT_3D('',#43061,#32813,#32814);
#29222=AXIS2_PLACEMENT_3D('',#43069,#32819,#32820);
#29223=AXIS2_PLACEMENT_3D('',#43073,#32823,#32824);
#29224=AXIS2_PLACEMENT_3D('',#43079,#32828,#32829);
#29225=AXIS2_PLACEMENT_3D('',#43087,#32834,#32835);
#29226=AXIS2_PLACEMENT_3D('',#43089,#32837,#32838);
#29227=AXIS2_PLACEMENT_3D('',#43095,#32842,#32843);
#29228=AXIS2_PLACEMENT_3D('',#43098,#32846,#32847);
#29229=AXIS2_PLACEMENT_3D('',#43103,#32851,#32852);
#29230=AXIS2_PLACEMENT_3D('',#43109,#32856,#32857);
#29231=AXIS2_PLACEMENT_3D('',#43117,#32862,#32863);
#29232=AXIS2_PLACEMENT_3D('',#43123,#32866,#32867);
#29233=AXIS2_PLACEMENT_3D('',#43126,#32869,#32870);
#29234=AXIS2_PLACEMENT_3D('',#43127,#32871,#32872);
#29235=AXIS2_PLACEMENT_3D('',#43133,#32876,#32877);
#29236=AXIS2_PLACEMENT_3D('',#43141,#32882,#32883);
#29237=AXIS2_PLACEMENT_3D('',#43151,#32889,#32890);
#29238=AXIS2_PLACEMENT_3D('',#43157,#32894,#32895);
#29239=AXIS2_PLACEMENT_3D('',#43164,#32899,#32900);
#29240=AXIS2_PLACEMENT_3D('',#43167,#32902,#32903);
#29241=AXIS2_PLACEMENT_3D('',#43168,#32904,#32905);
#29242=AXIS2_PLACEMENT_3D('',#43170,#32907,#32908);
#29243=AXIS2_PLACEMENT_3D('',#43172,#32910,#32911);
#29244=AXIS2_PLACEMENT_3D('',#43176,#32914,#32915);
#29245=AXIS2_PLACEMENT_3D('',#43178,#32917,#32918);
#29246=AXIS2_PLACEMENT_3D('',#43193,#32927,#32928);
#29247=AXIS2_PLACEMENT_3D('',#43195,#32930,#32931);
#29248=AXIS2_PLACEMENT_3D('',#43196,#32932,#32933);
#29249=AXIS2_PLACEMENT_3D('',#43202,#32937,#32938);
#29250=AXIS2_PLACEMENT_3D('',#43206,#32941,#32942);
#29251=AXIS2_PLACEMENT_3D('',#43212,#32946,#32947);
#29252=AXIS2_PLACEMENT_3D('',#43217,#32951,#32952);
#29253=AXIS2_PLACEMENT_3D('',#43219,#32954,#32955);
#29254=AXIS2_PLACEMENT_3D('',#43225,#32959,#32960);
#29255=AXIS2_PLACEMENT_3D('',#43227,#32962,#32963);
#29256=AXIS2_PLACEMENT_3D('',#43228,#32964,#32965);
#29257=AXIS2_PLACEMENT_3D('',#43236,#32970,#32971);
#29258=AXIS2_PLACEMENT_3D('',#43239,#32974,#32975);
#29259=AXIS2_PLACEMENT_3D('',#43240,#32976,#32977);
#29260=AXIS2_PLACEMENT_3D('',#43244,#32980,#32981);
#29261=AXIS2_PLACEMENT_3D('',#43252,#32985,#32986);
#29262=AXIS2_PLACEMENT_3D('',#43255,#32988,#32989);
#29263=AXIS2_PLACEMENT_3D('',#43256,#32990,#32991);
#29264=AXIS2_PLACEMENT_3D('',#43262,#32995,#32996);
#29265=AXIS2_PLACEMENT_3D('',#43264,#32998,#32999);
#29266=AXIS2_PLACEMENT_3D('',#43268,#33002,#33003);
#29267=AXIS2_PLACEMENT_3D('',#43271,#33006,#33007);
#29268=AXIS2_PLACEMENT_3D('',#43276,#33009,#33010);
#29269=AXIS2_PLACEMENT_3D('',#43279,#33012,#33013);
#29270=AXIS2_PLACEMENT_3D('',#43280,#33014,#33015);
#29271=AXIS2_PLACEMENT_3D('',#43286,#33019,#33020);
#29272=AXIS2_PLACEMENT_3D('',#43289,#33022,#33023);
#29273=AXIS2_PLACEMENT_3D('',#43290,#33024,#33025);
#29274=AXIS2_PLACEMENT_3D('',#43294,#33028,#33029);
#29275=AXIS2_PLACEMENT_3D('',#43295,#33030,#33031);
#29276=AXIS2_PLACEMENT_3D('',#43296,#33032,#33033);
#29277=AXIS2_PLACEMENT_3D('',#43300,#33035,#33036);
#29278=AXIS2_PLACEMENT_3D('',#43302,#33038,#33039);
#29279=AXIS2_PLACEMENT_3D('',#43306,#33042,#33043);
#29280=AXIS2_PLACEMENT_3D('',#43309,#33046,#33047);
#29281=AXIS2_PLACEMENT_3D('',#43312,#33049,#33050);
#29282=AXIS2_PLACEMENT_3D('',#43313,#33051,#33052);
#29283=AXIS2_PLACEMENT_3D('',#43316,#33055,#33056);
#29284=AXIS2_PLACEMENT_3D('',#43317,#33057,#33058);
#29285=AXIS2_PLACEMENT_3D('',#43319,#33060,#33061);
#29286=AXIS2_PLACEMENT_3D('',#43325,#33065,#33066);
#29287=AXIS2_PLACEMENT_3D('',#43328,#33068,#33069);
#29288=AXIS2_PLACEMENT_3D('',#43329,#33070,#33071);
#29289=AXIS2_PLACEMENT_3D('',#43333,#33074,#33075);
#29290=AXIS2_PLACEMENT_3D('',#43334,#33076,#33077);
#29291=AXIS2_PLACEMENT_3D('',#43335,#33078,#33079);
#29292=AXIS2_PLACEMENT_3D('',#43339,#33081,#33082);
#29293=AXIS2_PLACEMENT_3D('',#43341,#33084,#33085);
#29294=AXIS2_PLACEMENT_3D('',#43345,#33088,#33089);
#29295=AXIS2_PLACEMENT_3D('',#43348,#33092,#33093);
#29296=AXIS2_PLACEMENT_3D('',#43351,#33095,#33096);
#29297=AXIS2_PLACEMENT_3D('',#43352,#33097,#33098);
#29298=AXIS2_PLACEMENT_3D('',#43355,#33101,#33102);
#29299=AXIS2_PLACEMENT_3D('',#43356,#33103,#33104);
#29300=AXIS2_PLACEMENT_3D('',#43358,#33106,#33107);
#29301=AXIS2_PLACEMENT_3D('',#43359,#33108,#33109);
#29302=AXIS2_PLACEMENT_3D('',#43360,#33110,#33111);
#29303=AXIS2_PLACEMENT_3D('',#43361,#33112,#33113);
#29304=AXIS2_PLACEMENT_3D('',#43362,#33114,#33115);
#29305=AXIS2_PLACEMENT_3D('',#43363,#33116,#33117);
#29306=AXIS2_PLACEMENT_3D('',#43364,#33118,#33119);
#29307=AXIS2_PLACEMENT_3D('',#43365,#33120,#33121);
#29308=AXIS2_PLACEMENT_3D('',#43378,#33128,#33129);
#29309=AXIS2_PLACEMENT_3D('',#43388,#33135,#33136);
#29310=AXIS2_PLACEMENT_3D('',#43392,#33139,#33140);
#29311=AXIS2_PLACEMENT_3D('',#43400,#33145,#33146);
#29312=AXIS2_PLACEMENT_3D('',#43406,#33150,#33151);
#29313=AXIS2_PLACEMENT_3D('',#43419,#33158,#33159);
#29314=AXIS2_PLACEMENT_3D('',#43429,#33165,#33166);
#29315=AXIS2_PLACEMENT_3D('',#43435,#33170,#33171);
#29316=AXIS2_PLACEMENT_3D('',#43440,#33174,#33175);
#29317=AXIS2_PLACEMENT_3D('',#43442,#33176,#33177);
#29318=AXIS2_PLACEMENT_3D('',#43443,#33178,#33179);
#29319=AXIS2_PLACEMENT_3D('',#43456,#33186,#33187);
#29320=AXIS2_PLACEMENT_3D('',#43463,#33192,#33193);
#29321=AXIS2_PLACEMENT_3D('',#43468,#33196,#33197);
#29322=AXIS2_PLACEMENT_3D('',#43470,#33198,#33199);
#29323=AXIS2_PLACEMENT_3D('',#43471,#33200,#33201);
#29324=AXIS2_PLACEMENT_3D('',#43479,#33206,#33207);
#29325=AXIS2_PLACEMENT_3D('',#43483,#33210,#33211);
#29326=AXIS2_PLACEMENT_3D('',#43488,#33215,#33216);
#29327=AXIS2_PLACEMENT_3D('',#43491,#33218,#33219);
#29328=AXIS2_PLACEMENT_3D('',#43492,#33220,#33221);
#29329=AXIS2_PLACEMENT_3D('',#43494,#33222,#33223);
#29330=AXIS2_PLACEMENT_3D('',#43496,#33225,#33226);
#29331=AXIS2_PLACEMENT_3D('',#43498,#33228,#33229);
#29332=AXIS2_PLACEMENT_3D('',#43501,#33231,#33232);
#29333=AXIS2_PLACEMENT_3D('',#43502,#33233,#33234);
#29334=AXIS2_PLACEMENT_3D('',#43504,#33235,#33236);
#29335=AXIS2_PLACEMENT_3D('',#43506,#33238,#33239);
#29336=AXIS2_PLACEMENT_3D('',#43508,#33241,#33242);
#29337=AXIS2_PLACEMENT_3D('',#43512,#33245,#33246);
#29338=AXIS2_PLACEMENT_3D('',#43515,#33249,#33250);
#29339=AXIS2_PLACEMENT_3D('',#43518,#33253,#33254);
#29340=AXIS2_PLACEMENT_3D('',#43519,#33255,#33256);
#29341=AXIS2_PLACEMENT_3D('',#43520,#33257,#33258);
#29342=AXIS2_PLACEMENT_3D('',#43523,#33261,#33262);
#29343=AXIS2_PLACEMENT_3D('',#43526,#33265,#33266);
#29344=AXIS2_PLACEMENT_3D('',#43527,#33267,#33268);
#29345=AXIS2_PLACEMENT_3D('',#43528,#33269,#33270);
#29346=AXIS2_PLACEMENT_3D('',#43529,#33271,#33272);
#29347=AXIS2_PLACEMENT_3D('',#43530,#33273,#33274);
#29348=AXIS2_PLACEMENT_3D('',#43535,#33276,#33277);
#29349=AXIS2_PLACEMENT_3D('',#43538,#33279,#33280);
#29350=AXIS2_PLACEMENT_3D('',#43539,#33281,#33282);
#29351=AXIS2_PLACEMENT_3D('',#43545,#33286,#33287);
#29352=AXIS2_PLACEMENT_3D('',#43549,#33289,#33290);
#29353=AXIS2_PLACEMENT_3D('',#43550,#33291,#33292);
#29354=AXIS2_PLACEMENT_3D('',#43551,#33293,#33294);
#29355=AXIS2_PLACEMENT_3D('',#43557,#33298,#33299);
#29356=AXIS2_PLACEMENT_3D('',#43561,#33301,#33302);
#29357=AXIS2_PLACEMENT_3D('',#43562,#33303,#33304);
#29358=AXIS2_PLACEMENT_3D('',#43563,#33305,#33306);
#29359=AXIS2_PLACEMENT_3D('',#43569,#33310,#33311);
#29360=AXIS2_PLACEMENT_3D('',#43573,#33313,#33314);
#29361=AXIS2_PLACEMENT_3D('',#43574,#33315,#33316);
#29362=AXIS2_PLACEMENT_3D('',#43575,#33317,#33318);
#29363=AXIS2_PLACEMENT_3D('',#43578,#33321,#33322);
#29364=AXIS2_PLACEMENT_3D('',#43584,#33326,#33327);
#29365=AXIS2_PLACEMENT_3D('',#43587,#33329,#33330);
#29366=AXIS2_PLACEMENT_3D('',#43588,#33331,#33332);
#29367=AXIS2_PLACEMENT_3D('',#43592,#33335,#33336);
#29368=AXIS2_PLACEMENT_3D('',#43595,#33338,#33339);
#29369=AXIS2_PLACEMENT_3D('',#43596,#33340,#33341);
#29370=AXIS2_PLACEMENT_3D('',#43598,#33342,#33343);
#29371=AXIS2_PLACEMENT_3D('',#43600,#33344,#33345);
#29372=AXIS2_PLACEMENT_3D('',#43602,#33346,#33347);
#29373=AXIS2_PLACEMENT_3D('',#43603,#33348,#33349);
#29374=AXIS2_PLACEMENT_3D('',#43612,#33354,#33355);
#29375=AXIS2_PLACEMENT_3D('',#43614,#33356,#33357);
#29376=AXIS2_PLACEMENT_3D('',#43617,#33359,#33360);
#29377=AXIS2_PLACEMENT_3D('',#43618,#33361,#33362);
#29378=AXIS2_PLACEMENT_3D('',#43624,#33366,#33367);
#29379=AXIS2_PLACEMENT_3D('',#43630,#33371,#33372);
#29380=AXIS2_PLACEMENT_3D('',#43633,#33374,#33375);
#29381=AXIS2_PLACEMENT_3D('',#43634,#33376,#33377);
#29382=AXIS2_PLACEMENT_3D('',#43638,#33380,#33381);
#29383=AXIS2_PLACEMENT_3D('',#43642,#33383,#33384);
#29384=AXIS2_PLACEMENT_3D('',#43643,#33385,#33386);
#29385=AXIS2_PLACEMENT_3D('',#43644,#33387,#33388);
#29386=AXIS2_PLACEMENT_3D('',#43650,#33392,#33393);
#29387=AXIS2_PLACEMENT_3D('',#43654,#33395,#33396);
#29388=AXIS2_PLACEMENT_3D('',#43655,#33397,#33398);
#29389=AXIS2_PLACEMENT_3D('',#43656,#33399,#33400);
#29390=AXIS2_PLACEMENT_3D('',#43661,#33404,#33405);
#29391=AXIS2_PLACEMENT_3D('',#43662,#33406,#33407);
#29392=AXIS2_PLACEMENT_3D('',#43663,#33408,#33409);
#29393=AXIS2_PLACEMENT_3D('',#43667,#33411,#33412);
#29394=AXIS2_PLACEMENT_3D('',#43669,#33414,#33415);
#29395=AXIS2_PLACEMENT_3D('',#43673,#33418,#33419);
#29396=AXIS2_PLACEMENT_3D('',#43676,#33421,#33422);
#29397=AXIS2_PLACEMENT_3D('',#43677,#33423,#33424);
#29398=AXIS2_PLACEMENT_3D('',#43682,#33427,#33428);
#29399=AXIS2_PLACEMENT_3D('',#43683,#33429,#33430);
#29400=AXIS2_PLACEMENT_3D('',#43686,#33433,#33434);
#29401=AXIS2_PLACEMENT_3D('',#43687,#33435,#33436);
#29402=AXIS2_PLACEMENT_3D('',#43696,#33441,#33442);
#29403=AXIS2_PLACEMENT_3D('',#43700,#33444,#33445);
#29404=AXIS2_PLACEMENT_3D('',#43701,#33446,#33447);
#29405=AXIS2_PLACEMENT_3D('',#43702,#33448,#33449);
#29406=AXIS2_PLACEMENT_3D('',#43708,#33453,#33454);
#29407=AXIS2_PLACEMENT_3D('',#43712,#33456,#33457);
#29408=AXIS2_PLACEMENT_3D('',#43713,#33458,#33459);
#29409=AXIS2_PLACEMENT_3D('',#43714,#33460,#33461);
#29410=AXIS2_PLACEMENT_3D('',#43720,#33465,#33466);
#29411=AXIS2_PLACEMENT_3D('',#43724,#33468,#33469);
#29412=AXIS2_PLACEMENT_3D('',#43726,#33471,#33472);
#29413=AXIS2_PLACEMENT_3D('',#43730,#33475,#33476);
#29414=AXIS2_PLACEMENT_3D('',#43739,#33481,#33482);
#29415=AXIS2_PLACEMENT_3D('',#43743,#33484,#33485);
#29416=AXIS2_PLACEMENT_3D('',#43744,#33486,#33487);
#29417=AXIS2_PLACEMENT_3D('',#43745,#33488,#33489);
#29418=AXIS2_PLACEMENT_3D('',#43751,#33493,#33494);
#29419=AXIS2_PLACEMENT_3D('',#43755,#33496,#33497);
#29420=AXIS2_PLACEMENT_3D('',#43756,#33498,#33499);
#29421=AXIS2_PLACEMENT_3D('',#43757,#33500,#33501);
#29422=AXIS2_PLACEMENT_3D('',#43763,#33505,#33506);
#29423=AXIS2_PLACEMENT_3D('',#43766,#33508,#33509);
#29424=AXIS2_PLACEMENT_3D('',#43767,#33510,#33511);
#29425=AXIS2_PLACEMENT_3D('',#43776,#33516,#33517);
#29426=AXIS2_PLACEMENT_3D('',#43780,#33519,#33520);
#29427=AXIS2_PLACEMENT_3D('',#43781,#33521,#33522);
#29428=AXIS2_PLACEMENT_3D('',#43782,#33523,#33524);
#29429=AXIS2_PLACEMENT_3D('',#43788,#33528,#33529);
#29430=AXIS2_PLACEMENT_3D('',#43792,#33531,#33532);
#29431=AXIS2_PLACEMENT_3D('',#43793,#33533,#33534);
#29432=AXIS2_PLACEMENT_3D('',#43794,#33535,#33536);
#29433=AXIS2_PLACEMENT_3D('',#43800,#33540,#33541);
#29434=AXIS2_PLACEMENT_3D('',#43803,#33543,#33544);
#29435=AXIS2_PLACEMENT_3D('',#43804,#33545,#33546);
#29436=AXIS2_PLACEMENT_3D('',#43813,#33551,#33552);
#29437=AXIS2_PLACEMENT_3D('',#43817,#33554,#33555);
#29438=AXIS2_PLACEMENT_3D('',#43818,#33556,#33557);
#29439=AXIS2_PLACEMENT_3D('',#43819,#33558,#33559);
#29440=AXIS2_PLACEMENT_3D('',#43825,#33563,#33564);
#29441=AXIS2_PLACEMENT_3D('',#43829,#33566,#33567);
#29442=AXIS2_PLACEMENT_3D('',#43830,#33568,#33569);
#29443=AXIS2_PLACEMENT_3D('',#43831,#33570,#33571);
#29444=AXIS2_PLACEMENT_3D('',#43837,#33575,#33576);
#29445=AXIS2_PLACEMENT_3D('',#43842,#33580,#33581);
#29446=AXIS2_PLACEMENT_3D('',#43844,#33583,#33584);
#29447=AXIS2_PLACEMENT_3D('',#43846,#33586,#33587);
#29448=AXIS2_PLACEMENT_3D('',#43848,#33589,#33590);
#29449=AXIS2_PLACEMENT_3D('',#43852,#33593,#33594);
#29450=AXIS2_PLACEMENT_3D('',#43855,#33596,#33597);
#29451=AXIS2_PLACEMENT_3D('',#43856,#33598,#33599);
#29452=AXIS2_PLACEMENT_3D('',#43858,#33600,#33601);
#29453=AXIS2_PLACEMENT_3D('',#43861,#33603,#33604);
#29454=AXIS2_PLACEMENT_3D('',#43862,#33605,#33606);
#29455=AXIS2_PLACEMENT_3D('',#43864,#33607,#33608);
#29456=AXIS2_PLACEMENT_3D('',#43865,#33609,#33610);
#29457=AXIS2_PLACEMENT_3D('',#43867,#33612,#33613);
#29458=AXIS2_PLACEMENT_3D('',#43870,#33615,#33616);
#29459=AXIS2_PLACEMENT_3D('',#43871,#33617,#33618);
#29460=AXIS2_PLACEMENT_3D('',#43873,#33619,#33620);
#29461=AXIS2_PLACEMENT_3D('',#43875,#33622,#33623);
#29462=AXIS2_PLACEMENT_3D('',#43878,#33625,#33626);
#29463=AXIS2_PLACEMENT_3D('',#43879,#33627,#33628);
#29464=AXIS2_PLACEMENT_3D('',#43882,#33630,#33631);
#29465=AXIS2_PLACEMENT_3D('',#43883,#33632,#33633);
#29466=AXIS2_PLACEMENT_3D('',#43886,#33635,#33636);
#29467=AXIS2_PLACEMENT_3D('',#43889,#33638,#33639);
#29468=AXIS2_PLACEMENT_3D('',#43891,#33641,#33642);
#29469=AXIS2_PLACEMENT_3D('',#43894,#33645,#33646);
#29470=AXIS2_PLACEMENT_3D('',#43896,#33648,#33649);
#29471=AXIS2_PLACEMENT_3D('',#43898,#33651,#33652);
#29472=AXIS2_PLACEMENT_3D('',#43901,#33654,#33655);
#29473=AXIS2_PLACEMENT_3D('',#43902,#33656,#33657);
#29474=AXIS2_PLACEMENT_3D('',#43904,#33659,#33660);
#29475=AXIS2_PLACEMENT_3D('',#43906,#33662,#33663);
#29476=AXIS2_PLACEMENT_3D('',#43907,#33664,#33665);
#29477=AXIS2_PLACEMENT_3D('',#43908,#33666,#33667);
#29478=AXIS2_PLACEMENT_3D('',#43910,#33668,#33669);
#29479=AXIS2_PLACEMENT_3D('',#43912,#33671,#33672);
#29480=AXIS2_PLACEMENT_3D('',#43914,#33674,#33675);
#29481=AXIS2_PLACEMENT_3D('',#43915,#33676,#33677);
#29482=AXIS2_PLACEMENT_3D('',#43916,#33678,#33679);
#29483=AXIS2_PLACEMENT_3D('',#43918,#33680,#33681);
#29484=AXIS2_PLACEMENT_3D('',#43919,#33682,#33683);
#29485=AXIS2_PLACEMENT_3D('',#43920,#33684,#33685);
#29486=AXIS2_PLACEMENT_3D('',#43921,#33686,#33687);
#29487=AXIS2_PLACEMENT_3D('',#43924,#33689,#33690);
#29488=AXIS2_PLACEMENT_3D('',#43925,#33691,#33692);
#29489=AXIS2_PLACEMENT_3D('',#43927,#33694,#33695);
#29490=AXIS2_PLACEMENT_3D('',#43929,#33696,#33697);
#29491=AXIS2_PLACEMENT_3D('',#43932,#33699,#33700);
#29492=AXIS2_PLACEMENT_3D('',#43933,#33701,#33702);
#29493=AXIS2_PLACEMENT_3D('',#43935,#33703,#33704);
#29494=AXIS2_PLACEMENT_3D('',#43937,#33706,#33707);
#29495=AXIS2_PLACEMENT_3D('',#43939,#33708,#33709);
#29496=AXIS2_PLACEMENT_3D('',#43940,#33710,#33711);
#29497=AXIS2_PLACEMENT_3D('',#43941,#33712,#33713);
#29498=AXIS2_PLACEMENT_3D('',#43942,#33714,#33715);
#29499=AXIS2_PLACEMENT_3D('',#43943,#33716,#33717);
#29500=AXIS2_PLACEMENT_3D('',#43944,#33718,#33719);
#29501=AXIS2_PLACEMENT_3D('',#43945,#33720,#33721);
#29502=AXIS2_PLACEMENT_3D('',#43948,#33722,#33723);
#29503=AXIS2_PLACEMENT_3D('',#43949,#33724,#33725);
#29504=AXIS2_PLACEMENT_3D('',#43950,#33726,#33727);
#29505=AXIS2_PLACEMENT_3D('',#43951,#33728,#33729);
#29506=AXIS2_PLACEMENT_3D('',#43953,#33730,#33731);
#29507=AXIS2_PLACEMENT_3D('',#43955,#33733,#33734);
#29508=AXIS2_PLACEMENT_3D('',#43957,#33735,#33736);
#29509=AXIS2_PLACEMENT_3D('',#43958,#33737,#33738);
#29510=AXIS2_PLACEMENT_3D('',#43960,#33739,#33740);
#29511=AXIS2_PLACEMENT_3D('',#43962,#33742,#33743);
#29512=AXIS2_PLACEMENT_3D('',#43964,#33744,#33745);
#29513=AXIS2_PLACEMENT_3D('',#43966,#33747,#33748);
#29514=AXIS2_PLACEMENT_3D('',#43968,#33750,#33751);
#29515=AXIS2_PLACEMENT_3D('',#43974,#33755,#33756);
#29516=AXIS2_PLACEMENT_3D('',#43977,#33758,#33759);
#29517=AXIS2_PLACEMENT_3D('',#43978,#33760,#33761);
#29518=AXIS2_PLACEMENT_3D('',#43984,#33765,#33766);
#29519=AXIS2_PLACEMENT_3D('',#43988,#33768,#33769);
#29520=AXIS2_PLACEMENT_3D('',#43989,#33770,#33771);
#29521=AXIS2_PLACEMENT_3D('',#43990,#33772,#33773);
#29522=AXIS2_PLACEMENT_3D('',#43996,#33777,#33778);
#29523=AXIS2_PLACEMENT_3D('',#43999,#33780,#33781);
#29524=AXIS2_PLACEMENT_3D('',#44000,#33782,#33783);
#29525=AXIS2_PLACEMENT_3D('',#44001,#33784,#33785);
#29526=AXIS2_PLACEMENT_3D('',#44005,#33788,#33789);
#29527=AXIS2_PLACEMENT_3D('',#44006,#33790,#33791);
#29528=AXIS2_PLACEMENT_3D('',#44007,#33792,#33793);
#29529=AXIS2_PLACEMENT_3D('',#44009,#33795,#33796);
#29530=AXIS2_PLACEMENT_3D('',#44010,#33797,#33798);
#29531=AXIS2_PLACEMENT_3D('',#44012,#33800,#33801);
#29532=AXIS2_PLACEMENT_3D('',#44013,#33802,#33803);
#29533=AXIS2_PLACEMENT_3D('',#44015,#33805,#33806);
#29534=AXIS2_PLACEMENT_3D('',#44017,#33808,#33809);
#29535=AXIS2_PLACEMENT_3D('',#44018,#33810,#33811);
#29536=AXIS2_PLACEMENT_3D('',#44019,#33812,#33813);
#29537=AXIS2_PLACEMENT_3D('',#44041,#33815,#33816);
#29538=AXIS2_PLACEMENT_3D('',#44052,#33817,#33818);
#29539=AXIS2_PLACEMENT_3D('',#44142,#33820,#33821);
#29540=AXIS2_PLACEMENT_3D('',#44232,#33823,#33824);
#29541=AXIS2_PLACEMENT_3D('',#44322,#33826,#33827);
#29542=AXIS2_PLACEMENT_3D('',#44327,#33829,#33830);
#29543=AXIS2_PLACEMENT_3D('',#44411,#33831,#33832);
#29544=AXIS2_PLACEMENT_3D('',#44429,#33834,#33835);
#29545=AXIS2_PLACEMENT_3D('',#44439,#33836,#33837);
#29546=AXIS2_PLACEMENT_3D('',#44477,#33839,#33840);
#29547=AXIS2_PLACEMENT_3D('',#44515,#33842,#33843);
#29548=AXIS2_PLACEMENT_3D('',#44553,#33845,#33846);
#29549=AXIS2_PLACEMENT_3D('',#44564,#33850,#33851);
#29550=AXIS2_PLACEMENT_3D('',#44572,#33854,#33855);
#29551=AXIS2_PLACEMENT_3D('',#44573,#33856,#33857);
#29552=AXIS2_PLACEMENT_3D('',#44574,#33858,#33859);
#29553=AXIS2_PLACEMENT_3D('',#44585,#33863,#33864);
#29554=AXIS2_PLACEMENT_3D('',#44593,#33867,#33868);
#29555=AXIS2_PLACEMENT_3D('',#44594,#33869,#33870);
#29556=AXIS2_PLACEMENT_3D('',#44595,#33871,#33872);
#29557=AXIS2_PLACEMENT_3D('',#44606,#33876,#33877);
#29558=AXIS2_PLACEMENT_3D('',#44614,#33880,#33881);
#29559=AXIS2_PLACEMENT_3D('',#44615,#33882,#33883);
#29560=AXIS2_PLACEMENT_3D('',#44616,#33884,#33885);
#29561=AXIS2_PLACEMENT_3D('',#44627,#33889,#33890);
#29562=AXIS2_PLACEMENT_3D('',#44635,#33893,#33894);
#29563=AXIS2_PLACEMENT_3D('',#44636,#33895,#33896);
#29564=AXIS2_PLACEMENT_3D('',#44637,#33897,#33898);
#29565=AXIS2_PLACEMENT_3D('',#44648,#33902,#33903);
#29566=AXIS2_PLACEMENT_3D('',#44656,#33906,#33907);
#29567=AXIS2_PLACEMENT_3D('',#44657,#33908,#33909);
#29568=AXIS2_PLACEMENT_3D('',#44658,#33910,#33911);
#29569=AXIS2_PLACEMENT_3D('',#44669,#33915,#33916);
#29570=AXIS2_PLACEMENT_3D('',#44677,#33919,#33920);
#29571=AXIS2_PLACEMENT_3D('',#44679,#33921,#33922);
#29572=AXIS2_PLACEMENT_3D('',#44680,#33923,#33924);
#29573=AXIS2_PLACEMENT_3D('',#44681,#33925,#33926);
#29574=AXIS2_PLACEMENT_3D('',#44692,#33930,#33931);
#29575=AXIS2_PLACEMENT_3D('',#44700,#33934,#33935);
#29576=AXIS2_PLACEMENT_3D('',#44701,#33936,#33937);
#29577=AXIS2_PLACEMENT_3D('',#44702,#33938,#33939);
#29578=AXIS2_PLACEMENT_3D('',#44713,#33943,#33944);
#29579=AXIS2_PLACEMENT_3D('',#44721,#33947,#33948);
#29580=AXIS2_PLACEMENT_3D('',#44722,#33949,#33950);
#29581=AXIS2_PLACEMENT_3D('',#44723,#33951,#33952);
#29582=AXIS2_PLACEMENT_3D('',#44734,#33956,#33957);
#29583=AXIS2_PLACEMENT_3D('',#44742,#33960,#33961);
#29584=AXIS2_PLACEMENT_3D('',#44743,#33962,#33963);
#29585=AXIS2_PLACEMENT_3D('',#44744,#33964,#33965);
#29586=AXIS2_PLACEMENT_3D('',#44755,#33969,#33970);
#29587=AXIS2_PLACEMENT_3D('',#44763,#33973,#33974);
#29588=AXIS2_PLACEMENT_3D('',#44764,#33975,#33976);
#29589=AXIS2_PLACEMENT_3D('',#44765,#33977,#33978);
#29590=AXIS2_PLACEMENT_3D('',#44776,#33982,#33983);
#29591=AXIS2_PLACEMENT_3D('',#44784,#33986,#33987);
#29592=AXIS2_PLACEMENT_3D('',#44785,#33988,#33989);
#29593=AXIS2_PLACEMENT_3D('',#44786,#33990,#33991);
#29594=AXIS2_PLACEMENT_3D('',#44797,#33995,#33996);
#29595=AXIS2_PLACEMENT_3D('',#44805,#33999,#34000);
#29596=AXIS2_PLACEMENT_3D('',#44806,#34001,#34002);
#29597=AXIS2_PLACEMENT_3D('',#44807,#34003,#34004);
#29598=AXIS2_PLACEMENT_3D('',#44818,#34008,#34009);
#29599=AXIS2_PLACEMENT_3D('',#44826,#34012,#34013);
#29600=AXIS2_PLACEMENT_3D('',#44827,#34014,#34015);
#29601=AXIS2_PLACEMENT_3D('',#44828,#34016,#34017);
#29602=AXIS2_PLACEMENT_3D('',#44839,#34021,#34022);
#29603=AXIS2_PLACEMENT_3D('',#44847,#34025,#34026);
#29604=AXIS2_PLACEMENT_3D('',#44848,#34027,#34028);
#29605=AXIS2_PLACEMENT_3D('',#44849,#34029,#34030);
#29606=AXIS2_PLACEMENT_3D('',#44860,#34034,#34035);
#29607=AXIS2_PLACEMENT_3D('',#44868,#34038,#34039);
#29608=AXIS2_PLACEMENT_3D('',#44869,#34040,#34041);
#29609=AXIS2_PLACEMENT_3D('',#44870,#34042,#34043);
#29610=AXIS2_PLACEMENT_3D('',#44881,#34047,#34048);
#29611=AXIS2_PLACEMENT_3D('',#44889,#34051,#34052);
#29612=AXIS2_PLACEMENT_3D('',#44890,#34053,#34054);
#29613=AXIS2_PLACEMENT_3D('',#44891,#34055,#34056);
#29614=AXIS2_PLACEMENT_3D('',#44902,#34060,#34061);
#29615=AXIS2_PLACEMENT_3D('',#44910,#34064,#34065);
#29616=AXIS2_PLACEMENT_3D('',#44911,#34066,#34067);
#29617=AXIS2_PLACEMENT_3D('',#44912,#34068,#34069);
#29618=AXIS2_PLACEMENT_3D('',#44923,#34073,#34074);
#29619=AXIS2_PLACEMENT_3D('',#44931,#34077,#34078);
#29620=AXIS2_PLACEMENT_3D('',#44932,#34079,#34080);
#29621=AXIS2_PLACEMENT_3D('',#44933,#34081,#34082);
#29622=AXIS2_PLACEMENT_3D('',#44944,#34086,#34087);
#29623=AXIS2_PLACEMENT_3D('',#44952,#34090,#34091);
#29624=AXIS2_PLACEMENT_3D('',#44953,#34092,#34093);
#29625=AXIS2_PLACEMENT_3D('',#44954,#34094,#34095);
#29626=AXIS2_PLACEMENT_3D('',#44965,#34099,#34100);
#29627=AXIS2_PLACEMENT_3D('',#44973,#34103,#34104);
#29628=AXIS2_PLACEMENT_3D('',#44974,#34105,#34106);
#29629=AXIS2_PLACEMENT_3D('',#44975,#34107,#34108);
#29630=AXIS2_PLACEMENT_3D('',#44986,#34112,#34113);
#29631=AXIS2_PLACEMENT_3D('',#44994,#34116,#34117);
#29632=AXIS2_PLACEMENT_3D('',#44995,#34118,#34119);
#29633=AXIS2_PLACEMENT_3D('',#44996,#34120,#34121);
#29634=AXIS2_PLACEMENT_3D('',#45007,#34125,#34126);
#29635=AXIS2_PLACEMENT_3D('',#45015,#34129,#34130);
#29636=AXIS2_PLACEMENT_3D('',#45016,#34131,#34132);
#29637=AXIS2_PLACEMENT_3D('',#45017,#34133,#34134);
#29638=AXIS2_PLACEMENT_3D('',#45028,#34138,#34139);
#29639=AXIS2_PLACEMENT_3D('',#45036,#34142,#34143);
#29640=AXIS2_PLACEMENT_3D('',#45037,#34144,#34145);
#29641=AXIS2_PLACEMENT_3D('',#45038,#34146,#34147);
#29642=AXIS2_PLACEMENT_3D('',#45049,#34151,#34152);
#29643=AXIS2_PLACEMENT_3D('',#45057,#34155,#34156);
#29644=AXIS2_PLACEMENT_3D('',#45058,#34157,#34158);
#29645=AXIS2_PLACEMENT_3D('',#45059,#34159,#34160);
#29646=AXIS2_PLACEMENT_3D('',#45061,#34161,#34162);
#29647=AXIS2_PLACEMENT_3D('',#45063,#34164,#34165);
#29648=AXIS2_PLACEMENT_3D('',#45064,#34166,#34167);
#29649=AXIS2_PLACEMENT_3D('',#45065,#34168,#34169);
#29650=AXIS2_PLACEMENT_3D('',#45066,#34170,#34171);
#29651=AXIS2_PLACEMENT_3D('',#45067,#34172,#34173);
#29652=AXIS2_PLACEMENT_3D('',#45068,#34174,#34175);
#29653=AXIS2_PLACEMENT_3D('',#45069,#34176,#34177);
#29654=AXIS2_PLACEMENT_3D('',#45070,#34178,#34179);
#29655=AXIS2_PLACEMENT_3D('',#45071,#34180,#34181);
#29656=AXIS2_PLACEMENT_3D('',#45072,#34182,#34183);
#29657=AXIS2_PLACEMENT_3D('',#45073,#34184,#34185);
#29658=AXIS2_PLACEMENT_3D('',#45074,#34186,#34187);
#29659=AXIS2_PLACEMENT_3D('',#45075,#34188,#34189);
#29660=AXIS2_PLACEMENT_3D('',#45076,#34190,#34191);
#29661=AXIS2_PLACEMENT_3D('',#45077,#34192,#34193);
#29662=AXIS2_PLACEMENT_3D('',#45078,#34194,#34195);
#29663=AXIS2_PLACEMENT_3D('',#45079,#34196,#34197);
#29664=AXIS2_PLACEMENT_3D('',#45080,#34198,#34199);
#29665=AXIS2_PLACEMENT_3D('',#45081,#34200,#34201);
#29666=AXIS2_PLACEMENT_3D('',#45082,#34202,#34203);
#29667=AXIS2_PLACEMENT_3D('',#45083,#34204,#34205);
#29668=AXIS2_PLACEMENT_3D('',#45084,#34206,#34207);
#29669=AXIS2_PLACEMENT_3D('',#45085,#34208,#34209);
#29670=AXIS2_PLACEMENT_3D('',#45086,#34210,#34211);
#29671=AXIS2_PLACEMENT_3D('',#45087,#34212,#34213);
#29672=AXIS2_PLACEMENT_3D('',#45088,#34214,#34215);
#29673=AXIS2_PLACEMENT_3D('',#45089,#34216,#34217);
#29674=AXIS2_PLACEMENT_3D('',#45090,#34218,#34219);
#29675=AXIS2_PLACEMENT_3D('',#45091,#34220,#34221);
#29676=AXIS2_PLACEMENT_3D('',#45092,#34222,#34223);
#29677=AXIS2_PLACEMENT_3D('',#45093,#34224,#34225);
#29678=AXIS2_PLACEMENT_3D('',#45094,#34226,#34227);
#29679=AXIS2_PLACEMENT_3D('',#45095,#34228,#34229);
#29680=AXIS2_PLACEMENT_3D('',#45096,#34230,#34231);
#29681=AXIS2_PLACEMENT_3D('',#45097,#34232,#34233);
#29682=AXIS2_PLACEMENT_3D('',#45098,#34234,#34235);
#29683=AXIS2_PLACEMENT_3D('',#45099,#34236,#34237);
#29684=AXIS2_PLACEMENT_3D('',#45100,#34238,#34239);
#29685=AXIS2_PLACEMENT_3D('',#45101,#34240,#34241);
#29686=AXIS2_PLACEMENT_3D('',#45102,#34242,#34243);
#29687=AXIS2_PLACEMENT_3D('',#45103,#34244,#34245);
#29688=AXIS2_PLACEMENT_3D('',#45104,#34246,#34247);
#29689=AXIS2_PLACEMENT_3D('',#45105,#34248,#34249);
#29690=AXIS2_PLACEMENT_3D('',#45106,#34250,#34251);
#29691=AXIS2_PLACEMENT_3D('',#45107,#34252,#34253);
#29692=AXIS2_PLACEMENT_3D('',#45108,#34254,#34255);
#29693=AXIS2_PLACEMENT_3D('',#45109,#34256,#34257);
#29694=AXIS2_PLACEMENT_3D('',#45110,#34258,#34259);
#29695=AXIS2_PLACEMENT_3D('',#45111,#34260,#34261);
#29696=AXIS2_PLACEMENT_3D('',#45112,#34262,#34263);
#29697=AXIS2_PLACEMENT_3D('',#45113,#34264,#34265);
#29698=AXIS2_PLACEMENT_3D('',#45114,#34266,#34267);
#29699=AXIS2_PLACEMENT_3D('',#45115,#34268,#34269);
#29700=AXIS2_PLACEMENT_3D('',#45116,#34270,#34271);
#29701=AXIS2_PLACEMENT_3D('',#45117,#34272,#34273);
#29702=AXIS2_PLACEMENT_3D('',#45118,#34274,#34275);
#29703=AXIS2_PLACEMENT_3D('',#45119,#34276,#34277);
#29704=AXIS2_PLACEMENT_3D('',#45120,#34278,#34279);
#29705=AXIS2_PLACEMENT_3D('',#45121,#34280,#34281);
#29706=AXIS2_PLACEMENT_3D('',#45122,#34282,#34283);
#29707=AXIS2_PLACEMENT_3D('',#45123,#34284,#34285);
#29708=AXIS2_PLACEMENT_3D('',#45124,#34286,#34287);
#29709=AXIS2_PLACEMENT_3D('',#45125,#34288,#34289);
#29710=AXIS2_PLACEMENT_3D('',#45126,#34290,#34291);
#29711=AXIS2_PLACEMENT_3D('',#45127,#34292,#34293);
#29712=AXIS2_PLACEMENT_3D('',#45128,#34294,#34295);
#29713=AXIS2_PLACEMENT_3D('',#45129,#34296,#34297);
#29714=AXIS2_PLACEMENT_3D('',#45130,#34298,#34299);
#29715=AXIS2_PLACEMENT_3D('',#45131,#34300,#34301);
#29716=AXIS2_PLACEMENT_3D('',#45132,#34302,#34303);
#29717=AXIS2_PLACEMENT_3D('',#45591,#34304,#34305);
#29718=AXIS2_PLACEMENT_3D('',#45593,#34306,#34307);
#29719=AXIS2_PLACEMENT_3D('',#46040,#34308,#34309);
#29720=AXIS2_PLACEMENT_3D('',#46041,#34310,#34311);
#29721=AXIS2_PLACEMENT_3D('',#46042,#34312,#34313);
#29722=AXIS2_PLACEMENT_3D('',#46044,#34314,#34315);
#29723=AXIS2_PLACEMENT_3D('',#46045,#34316,#34317);
#29724=AXIS2_PLACEMENT_3D('',#46047,#34318,#34319);
#29725=AXIS2_PLACEMENT_3D('',#46049,#34321,#34322);
#29726=AXIS2_PLACEMENT_3D('',#46051,#34323,#34324);
#29727=AXIS2_PLACEMENT_3D('',#46053,#34326,#34327);
#29728=AXIS2_PLACEMENT_3D('',#46055,#34328,#34329);
#29729=AXIS2_PLACEMENT_3D('',#46057,#34331,#34332);
#29730=AXIS2_PLACEMENT_3D('',#46058,#34333,#34334);
#29731=AXIS2_PLACEMENT_3D('',#46060,#34335,#34336);
#29732=AXIS2_PLACEMENT_3D('',#46061,#34337,#34338);
#29733=AXIS2_PLACEMENT_3D('',#46062,#34339,#34340);
#29734=AXIS2_PLACEMENT_3D('',#46064,#34342,#34343);
#29735=AXIS2_PLACEMENT_3D('',#46065,#34344,#34345);
#29736=AXIS2_PLACEMENT_3D('',#46066,#34346,#34347);
#29737=AXIS2_PLACEMENT_3D('',#46067,#34348,#34349);
#29738=AXIS2_PLACEMENT_3D('',#46083,#34351,#34352);
#29739=AXIS2_PLACEMENT_3D('',#46094,#34353,#34354);
#29740=AXIS2_PLACEMENT_3D('',#46142,#34356,#34357);
#29741=AXIS2_PLACEMENT_3D('',#46190,#34359,#34360);
#29742=AXIS2_PLACEMENT_3D('',#46244,#34362,#34363);
#29743=AXIS2_PLACEMENT_3D('',#46292,#34365,#34366);
#29744=AXIS2_PLACEMENT_3D('',#46340,#34368,#34369);
#29745=AXIS2_PLACEMENT_3D('',#46394,#34371,#34372);
#29746=AXIS2_PLACEMENT_3D('',#46442,#34374,#34375);
#29747=AXIS2_PLACEMENT_3D('',#46490,#34377,#34378);
#29748=AXIS2_PLACEMENT_3D('',#46544,#34380,#34381);
#29749=AXIS2_PLACEMENT_3D('',#46592,#34383,#34384);
#29750=AXIS2_PLACEMENT_3D('',#46640,#34386,#34387);
#29751=AXIS2_PLACEMENT_3D('',#46688,#34389,#34390);
#29752=AXIS2_PLACEMENT_3D('',#46736,#34392,#34393);
#29753=AXIS2_PLACEMENT_3D('',#46784,#34395,#34396);
#29754=AXIS2_PLACEMENT_3D('',#46795,#34398,#34399);
#29755=AXIS2_PLACEMENT_3D('',#46800,#34400,#34401);
#29756=AXIS2_PLACEMENT_3D('',#46825,#34403,#34404);
#29757=AXIS2_PLACEMENT_3D('',#46849,#34406,#34407);
#29758=AXIS2_PLACEMENT_3D('',#46875,#34409,#34410);
#29759=AXIS2_PLACEMENT_3D('',#46899,#34412,#34413);
#29760=AXIS2_PLACEMENT_3D('',#46923,#34415,#34416);
#29761=AXIS2_PLACEMENT_3D('',#46948,#34418,#34419);
#29762=AXIS2_PLACEMENT_3D('',#46973,#34421,#34422);
#29763=AXIS2_PLACEMENT_3D('',#46997,#34424,#34425);
#29764=AXIS2_PLACEMENT_3D('',#47022,#34427,#34428);
#29765=AXIS2_PLACEMENT_3D('',#47047,#34430,#34431);
#29766=AXIS2_PLACEMENT_3D('',#47071,#34433,#34434);
#29767=AXIS2_PLACEMENT_3D('',#47096,#34436,#34437);
#29768=AXIS2_PLACEMENT_3D('',#47121,#34439,#34440);
#29769=AXIS2_PLACEMENT_3D('',#47145,#34442,#34443);
#29770=AXIS2_PLACEMENT_3D('',#47156,#34447,#34448);
#29771=AXIS2_PLACEMENT_3D('',#47158,#34449,#34450);
#29772=AXIS2_PLACEMENT_3D('',#47160,#34452,#34453);
#29773=AXIS2_PLACEMENT_3D('',#47166,#34455,#34456);
#29774=AXIS2_PLACEMENT_3D('',#47177,#34460,#34461);
#29775=AXIS2_PLACEMENT_3D('',#47179,#34462,#34463);
#29776=AXIS2_PLACEMENT_3D('',#47181,#34465,#34466);
#29777=AXIS2_PLACEMENT_3D('',#47187,#34468,#34469);
#29778=AXIS2_PLACEMENT_3D('',#47198,#34473,#34474);
#29779=AXIS2_PLACEMENT_3D('',#47200,#34475,#34476);
#29780=AXIS2_PLACEMENT_3D('',#47202,#34478,#34479);
#29781=AXIS2_PLACEMENT_3D('',#47208,#34481,#34482);
#29782=AXIS2_PLACEMENT_3D('',#47219,#34486,#34487);
#29783=AXIS2_PLACEMENT_3D('',#47221,#34488,#34489);
#29784=AXIS2_PLACEMENT_3D('',#47223,#34491,#34492);
#29785=AXIS2_PLACEMENT_3D('',#47229,#34494,#34495);
#29786=AXIS2_PLACEMENT_3D('',#47240,#34499,#34500);
#29787=AXIS2_PLACEMENT_3D('',#47242,#34501,#34502);
#29788=AXIS2_PLACEMENT_3D('',#47244,#34504,#34505);
#29789=AXIS2_PLACEMENT_3D('',#47250,#34507,#34508);
#29790=AXIS2_PLACEMENT_3D('',#47261,#34512,#34513);
#29791=AXIS2_PLACEMENT_3D('',#47263,#34514,#34515);
#29792=AXIS2_PLACEMENT_3D('',#47265,#34517,#34518);
#29793=AXIS2_PLACEMENT_3D('',#47271,#34520,#34521);
#29794=AXIS2_PLACEMENT_3D('',#47282,#34525,#34526);
#29795=AXIS2_PLACEMENT_3D('',#47284,#34527,#34528);
#29796=AXIS2_PLACEMENT_3D('',#47286,#34530,#34531);
#29797=AXIS2_PLACEMENT_3D('',#47292,#34533,#34534);
#29798=AXIS2_PLACEMENT_3D('',#47303,#34538,#34539);
#29799=AXIS2_PLACEMENT_3D('',#47305,#34540,#34541);
#29800=AXIS2_PLACEMENT_3D('',#47307,#34543,#34544);
#29801=AXIS2_PLACEMENT_3D('',#47313,#34546,#34547);
#29802=AXIS2_PLACEMENT_3D('',#47324,#34551,#34552);
#29803=AXIS2_PLACEMENT_3D('',#47326,#34553,#34554);
#29804=AXIS2_PLACEMENT_3D('',#47328,#34556,#34557);
#29805=AXIS2_PLACEMENT_3D('',#47334,#34559,#34560);
#29806=AXIS2_PLACEMENT_3D('',#47345,#34564,#34565);
#29807=AXIS2_PLACEMENT_3D('',#47347,#34566,#34567);
#29808=AXIS2_PLACEMENT_3D('',#47349,#34569,#34570);
#29809=AXIS2_PLACEMENT_3D('',#47355,#34572,#34573);
#29810=AXIS2_PLACEMENT_3D('',#47366,#34577,#34578);
#29811=AXIS2_PLACEMENT_3D('',#47368,#34579,#34580);
#29812=AXIS2_PLACEMENT_3D('',#47370,#34582,#34583);
#29813=AXIS2_PLACEMENT_3D('',#47376,#34585,#34586);
#29814=AXIS2_PLACEMENT_3D('',#47387,#34590,#34591);
#29815=AXIS2_PLACEMENT_3D('',#47389,#34592,#34593);
#29816=AXIS2_PLACEMENT_3D('',#47391,#34595,#34596);
#29817=AXIS2_PLACEMENT_3D('',#47397,#34598,#34599);
#29818=AXIS2_PLACEMENT_3D('',#47408,#34603,#34604);
#29819=AXIS2_PLACEMENT_3D('',#47410,#34605,#34606);
#29820=AXIS2_PLACEMENT_3D('',#47412,#34608,#34609);
#29821=AXIS2_PLACEMENT_3D('',#47418,#34611,#34612);
#29822=AXIS2_PLACEMENT_3D('',#47429,#34616,#34617);
#29823=AXIS2_PLACEMENT_3D('',#47431,#34618,#34619);
#29824=AXIS2_PLACEMENT_3D('',#47434,#34621,#34622);
#29825=AXIS2_PLACEMENT_3D('',#47435,#34623,#34624);
#29826=AXIS2_PLACEMENT_3D('',#47441,#34626,#34627);
#29827=AXIS2_PLACEMENT_3D('',#47452,#34631,#34632);
#29828=AXIS2_PLACEMENT_3D('',#47454,#34633,#34634);
#29829=AXIS2_PLACEMENT_3D('',#47456,#34636,#34637);
#29830=AXIS2_PLACEMENT_3D('',#47462,#34639,#34640);
#29831=AXIS2_PLACEMENT_3D('',#47473,#34644,#34645);
#29832=AXIS2_PLACEMENT_3D('',#47475,#34646,#34647);
#29833=AXIS2_PLACEMENT_3D('',#47477,#34649,#34650);
#29834=AXIS2_PLACEMENT_3D('',#47483,#34652,#34653);
#29835=AXIS2_PLACEMENT_3D('',#47494,#34657,#34658);
#29836=AXIS2_PLACEMENT_3D('',#47496,#34659,#34660);
#29837=AXIS2_PLACEMENT_3D('',#47498,#34662,#34663);
#29838=AXIS2_PLACEMENT_3D('',#47504,#34665,#34666);
#29839=AXIS2_PLACEMENT_3D('',#47515,#34670,#34671);
#29840=AXIS2_PLACEMENT_3D('',#47517,#34672,#34673);
#29841=AXIS2_PLACEMENT_3D('',#47519,#34675,#34676);
#29842=AXIS2_PLACEMENT_3D('',#47525,#34678,#34679);
#29843=AXIS2_PLACEMENT_3D('',#47526,#34680,#34681);
#29844=AXIS2_PLACEMENT_3D('',#47527,#34682,#34683);
#29845=AXIS2_PLACEMENT_3D('',#47528,#34684,#34685);
#29846=AXIS2_PLACEMENT_3D('',#47529,#34686,#34687);
#29847=AXIS2_PLACEMENT_3D('',#47530,#34688,#34689);
#29848=AXIS2_PLACEMENT_3D('',#47531,#34690,#34691);
#29849=AXIS2_PLACEMENT_3D('',#47532,#34692,#34693);
#29850=AXIS2_PLACEMENT_3D('',#47535,#34695,#34696);
#29851=AXIS2_PLACEMENT_3D('',#47536,#34697,#34698);
#29852=AXIS2_PLACEMENT_3D('',#47537,#34699,#34700);
#29853=AXIS2_PLACEMENT_3D('',#47538,#34701,#34702);
#29854=AXIS2_PLACEMENT_3D('',#47539,#34703,#34704);
#29855=AXIS2_PLACEMENT_3D('',#47540,#34705,#34706);
#29856=AXIS2_PLACEMENT_3D('',#47541,#34707,#34708);
#29857=AXIS2_PLACEMENT_3D('',#47542,#34709,#34710);
#29858=AXIS2_PLACEMENT_3D('',#47543,#34711,#34712);
#29859=AXIS2_PLACEMENT_3D('',#47544,#34713,#34714);
#29860=AXIS2_PLACEMENT_3D('',#47545,#34715,#34716);
#29861=AXIS2_PLACEMENT_3D('',#47546,#34717,#34718);
#29862=AXIS2_PLACEMENT_3D('',#48106,#34719,#34720);
#29863=AXIS2_PLACEMENT_3D('',#48108,#34721,#34722);
#29864=AXIS2_PLACEMENT_3D('',#48109,#34723,#34724);
#29865=AXIS2_PLACEMENT_3D('',#48175,#34725,#34726);
#29866=AXIS2_PLACEMENT_3D('',#48176,#34727,#34728);
#29867=AXIS2_PLACEMENT_3D('',#48671,#34729,#34730);
#29868=AXIS2_PLACEMENT_3D('',#48673,#34731,#34732);
#29869=AXIS2_PLACEMENT_3D('',#48674,#34733,#34734);
#29870=AXIS2_PLACEMENT_3D('',#48676,#34736,#34737);
#29871=AXIS2_PLACEMENT_3D('',#48677,#34738,#34739);
#29872=AXIS2_PLACEMENT_3D('',#48678,#34740,#34741);
#29873=AXIS2_PLACEMENT_3D('',#48680,#34742,#34743);
#29874=AXIS2_PLACEMENT_3D('',#48681,#34744,#34745);
#29875=AXIS2_PLACEMENT_3D('',#48683,#34747,#34748);
#29876=AXIS2_PLACEMENT_3D('',#48685,#34749,#34750);
#29877=AXIS2_PLACEMENT_3D('',#48687,#34752,#34753);
#29878=AXIS2_PLACEMENT_3D('',#48688,#34754,#34755);
#29879=AXIS2_PLACEMENT_3D('',#48689,#34756,#34757);
#29880=AXIS2_PLACEMENT_3D('',#48691,#34758,#34759);
#29881=AXIS2_PLACEMENT_3D('',#48694,#34761,#34762);
#29882=AXIS2_PLACEMENT_3D('',#48695,#34763,#34764);
#29883=AXIS2_PLACEMENT_3D('',#48696,#34765,#34766);
#29884=AXIS2_PLACEMENT_3D('',#48710,#34773,#34774);
#29885=AXIS2_PLACEMENT_3D('',#48711,#34775,#34776);
#29886=AXIS2_PLACEMENT_3D('',#48717,#34780,#34781);
#29887=AXIS2_PLACEMENT_3D('',#48721,#34784,#34785);
#29888=AXIS2_PLACEMENT_3D('',#48725,#34788,#34789);
#29889=AXIS2_PLACEMENT_3D('',#48729,#34792,#34793);
#29890=AXIS2_PLACEMENT_3D('',#48733,#34796,#34797);
#29891=AXIS2_PLACEMENT_3D('',#48735,#34799,#34800);
#29892=AXIS2_PLACEMENT_3D('',#48736,#34801,#34802);
#29893=AXIS2_PLACEMENT_3D('',#48740,#34804,#34805);
#29894=AXIS2_PLACEMENT_3D('',#48741,#34806,#34807);
#29895=AXIS2_PLACEMENT_3D('',#48746,#34809,#34810);
#29896=AXIS2_PLACEMENT_3D('',#48747,#34811,#34812);
#29897=AXIS2_PLACEMENT_3D('',#48748,#34813,#34814);
#29898=AXIS2_PLACEMENT_3D('',#48786,#34816,#34817);
#29899=AXIS2_PLACEMENT_3D('',#48789,#34818,#34819);
#29900=AXIS2_PLACEMENT_3D('',#48793,#34821,#34822);
#29901=AXIS2_PLACEMENT_3D('',#48795,#34824,#34825);
#29902=AXIS2_PLACEMENT_3D('',#48801,#34829,#34830);
#29903=AXIS2_PLACEMENT_3D('',#48807,#34834,#34835);
#29904=AXIS2_PLACEMENT_3D('',#48813,#34839,#34840);
#29905=AXIS2_PLACEMENT_3D('',#48815,#34841,#34842);
#29906=AXIS2_PLACEMENT_3D('',#48817,#34843,#34844);
#29907=AXIS2_PLACEMENT_3D('',#48819,#34846,#34847);
#29908=AXIS2_PLACEMENT_3D('',#48825,#34851,#34852);
#29909=AXIS2_PLACEMENT_3D('',#48828,#34855,#34856);
#29910=AXIS2_PLACEMENT_3D('',#48829,#34857,#34858);
#29911=AXIS2_PLACEMENT_3D('',#48838,#34863,#34864);
#29912=AXIS2_PLACEMENT_3D('',#48844,#34868,#34869);
#29913=AXIS2_PLACEMENT_3D('',#48850,#34873,#34874);
#29914=AXIS2_PLACEMENT_3D('',#48853,#34877,#34878);
#29915=AXIS2_PLACEMENT_3D('',#48854,#34879,#34880);
#29916=AXIS2_PLACEMENT_3D('',#48863,#34885,#34886);
#29917=AXIS2_PLACEMENT_3D('',#48869,#34890,#34891);
#29918=AXIS2_PLACEMENT_3D('',#48875,#34895,#34896);
#29919=AXIS2_PLACEMENT_3D('',#48878,#34899,#34900);
#29920=AXIS2_PLACEMENT_3D('',#48879,#34901,#34902);
#29921=AXIS2_PLACEMENT_3D('',#48888,#34907,#34908);
#29922=AXIS2_PLACEMENT_3D('',#48894,#34912,#34913);
#29923=AXIS2_PLACEMENT_3D('',#48900,#34917,#34918);
#29924=AXIS2_PLACEMENT_3D('',#48903,#34921,#34922);
#29925=AXIS2_PLACEMENT_3D('',#48904,#34923,#34924);
#29926=AXIS2_PLACEMENT_3D('',#48913,#34929,#34930);
#29927=AXIS2_PLACEMENT_3D('',#48919,#34934,#34935);
#29928=AXIS2_PLACEMENT_3D('',#48925,#34939,#34940);
#29929=AXIS2_PLACEMENT_3D('',#48928,#34943,#34944);
#29930=AXIS2_PLACEMENT_3D('',#48929,#34945,#34946);
#29931=AXIS2_PLACEMENT_3D('',#48938,#34951,#34952);
#29932=AXIS2_PLACEMENT_3D('',#48944,#34956,#34957);
#29933=AXIS2_PLACEMENT_3D('',#48950,#34961,#34962);
#29934=AXIS2_PLACEMENT_3D('',#48953,#34965,#34966);
#29935=AXIS2_PLACEMENT_3D('',#48954,#34967,#34968);
#29936=AXIS2_PLACEMENT_3D('',#48963,#34973,#34974);
#29937=AXIS2_PLACEMENT_3D('',#48969,#34978,#34979);
#29938=AXIS2_PLACEMENT_3D('',#48975,#34983,#34984);
#29939=AXIS2_PLACEMENT_3D('',#48978,#34987,#34988);
#29940=AXIS2_PLACEMENT_3D('',#48979,#34989,#34990);
#29941=AXIS2_PLACEMENT_3D('',#48988,#34995,#34996);
#29942=AXIS2_PLACEMENT_3D('',#48994,#35000,#35001);
#29943=AXIS2_PLACEMENT_3D('',#49000,#35005,#35006);
#29944=AXIS2_PLACEMENT_3D('',#49003,#35009,#35010);
#29945=AXIS2_PLACEMENT_3D('',#49004,#35011,#35012);
#29946=AXIS2_PLACEMENT_3D('',#49013,#35017,#35018);
#29947=AXIS2_PLACEMENT_3D('',#49019,#35022,#35023);
#29948=AXIS2_PLACEMENT_3D('',#49025,#35027,#35028);
#29949=AXIS2_PLACEMENT_3D('',#49028,#35031,#35032);
#29950=AXIS2_PLACEMENT_3D('',#49029,#35033,#35034);
#29951=AXIS2_PLACEMENT_3D('',#49038,#35039,#35040);
#29952=AXIS2_PLACEMENT_3D('',#49044,#35044,#35045);
#29953=AXIS2_PLACEMENT_3D('',#49050,#35049,#35050);
#29954=AXIS2_PLACEMENT_3D('',#49053,#35053,#35054);
#29955=AXIS2_PLACEMENT_3D('',#49054,#35055,#35056);
#29956=AXIS2_PLACEMENT_3D('',#49063,#35061,#35062);
#29957=AXIS2_PLACEMENT_3D('',#49069,#35066,#35067);
#29958=AXIS2_PLACEMENT_3D('',#49075,#35071,#35072);
#29959=AXIS2_PLACEMENT_3D('',#49078,#35075,#35076);
#29960=AXIS2_PLACEMENT_3D('',#49079,#35077,#35078);
#29961=AXIS2_PLACEMENT_3D('',#49088,#35083,#35084);
#29962=AXIS2_PLACEMENT_3D('',#49094,#35088,#35089);
#29963=AXIS2_PLACEMENT_3D('',#49100,#35093,#35094);
#29964=AXIS2_PLACEMENT_3D('',#49103,#35097,#35098);
#29965=AXIS2_PLACEMENT_3D('',#49104,#35099,#35100);
#29966=AXIS2_PLACEMENT_3D('',#49106,#35101,#35102);
#29967=AXIS2_PLACEMENT_3D('',#49107,#35103,#35104);
#29968=AXIS2_PLACEMENT_3D('',#49110,#35106,#35107);
#29969=AXIS2_PLACEMENT_3D('',#49111,#35108,#35109);
#29970=AXIS2_PLACEMENT_3D('',#49113,#35110,#35111);
#29971=AXIS2_PLACEMENT_3D('',#49114,#35112,#35113);
#29972=AXIS2_PLACEMENT_3D('',#49116,#35114,#35115);
#29973=AXIS2_PLACEMENT_3D('',#49118,#35117,#35118);
#29974=AXIS2_PLACEMENT_3D('',#49120,#35119,#35120);
#29975=AXIS2_PLACEMENT_3D('',#49122,#35122,#35123);
#29976=AXIS2_PLACEMENT_3D('',#49124,#35124,#35125);
#29977=AXIS2_PLACEMENT_3D('',#49125,#35126,#35127);
#29978=AXIS2_PLACEMENT_3D('',#49127,#35128,#35129);
#29979=AXIS2_PLACEMENT_3D('',#49129,#35131,#35132);
#29980=AXIS2_PLACEMENT_3D('',#49131,#35133,#35134);
#29981=AXIS2_PLACEMENT_3D('',#49133,#35136,#35137);
#29982=AXIS2_PLACEMENT_3D('',#49134,#35138,#35139);
#29983=AXIS2_PLACEMENT_3D('',#49328,#35141,#35142);
#29984=AXIS2_PLACEMENT_3D('',#49366,#35144,#35145);
#29985=AXIS2_PLACEMENT_3D('',#49368,#35146,#35147);
#29986=AXIS2_PLACEMENT_3D('',#49371,#35149,#35150);
#29987=AXIS2_PLACEMENT_3D('',#49529,#35152,#35153);
#29988=AXIS2_PLACEMENT_3D('',#49531,#35154,#35155);
#29989=AXIS2_PLACEMENT_3D('',#49532,#35156,#35157);
#29990=AXIS2_PLACEMENT_3D('',#49602,#35158,#35159);
#29991=AXIS2_PLACEMENT_3D('',#49604,#35160,#35161);
#29992=AXIS2_PLACEMENT_3D('',#49608,#35164,#35165);
#29993=AXIS2_PLACEMENT_3D('',#49609,#35166,#35167);
#29994=AXIS2_PLACEMENT_3D('',#49611,#35168,#35169);
#29995=AXIS2_PLACEMENT_3D('',#49612,#35170,#35171);
#29996=AXIS2_PLACEMENT_3D('',#49614,#35173,#35174);
#29997=AXIS2_PLACEMENT_3D('',#49616,#35175,#35176);
#29998=AXIS2_PLACEMENT_3D('',#49617,#35177,#35178);
#29999=AXIS2_PLACEMENT_3D('',#49619,#35179,#35180);
#30000=AXIS2_PLACEMENT_3D('',#49621,#35182,#35183);
#30001=AXIS2_PLACEMENT_3D('',#49623,#35184,#35185);
#30002=AXIS2_PLACEMENT_3D('',#49625,#35187,#35188);
#30003=AXIS2_PLACEMENT_3D('',#49627,#35189,#35190);
#30004=AXIS2_PLACEMENT_3D('',#49629,#35192,#35193);
#30005=AXIS2_PLACEMENT_3D('',#49630,#35194,#35195);
#30006=AXIS2_PLACEMENT_3D('',#49632,#35196,#35197);
#30007=AXIS2_PLACEMENT_3D('',#49634,#35199,#35200);
#30008=AXIS2_PLACEMENT_3D('',#49635,#35201,#35202);
#30009=AXIS2_PLACEMENT_3D('',#49967,#35203,#35204);
#30010=AXIS2_PLACEMENT_3D('',#49999,#35205,#35206);
#30011=AXIS2_PLACEMENT_3D('',#50000,#35207,#35208);
#30012=AXIS2_PLACEMENT_3D('',#50001,#35209,#35210);
#30013=AXIS2_PLACEMENT_3D('',#50002,#35211,#35212);
#30014=AXIS2_PLACEMENT_3D('',#50003,#35213,#35214);
#30015=AXIS2_PLACEMENT_3D('',#50012,#35219,#35220);
#30016=AXIS2_PLACEMENT_3D('',#50018,#35224,#35225);
#30017=AXIS2_PLACEMENT_3D('',#50024,#35229,#35230);
#30018=AXIS2_PLACEMENT_3D('',#50033,#35235,#35236);
#30019=AXIS2_PLACEMENT_3D('',#50039,#35240,#35241);
#30020=AXIS2_PLACEMENT_3D('',#50045,#35245,#35246);
#30021=AXIS2_PLACEMENT_3D('',#50056,#35252,#35253);
#30022=AXIS2_PLACEMENT_3D('',#50070,#35261,#35262);
#30023=AXIS2_PLACEMENT_3D('',#50074,#35265,#35266);
#30024=AXIS2_PLACEMENT_3D('',#50082,#35271,#35272);
#30025=AXIS2_PLACEMENT_3D('',#50086,#35275,#35276);
#30026=AXIS2_PLACEMENT_3D('',#50095,#35282,#35283);
#30027=AXIS2_PLACEMENT_3D('',#50105,#35289,#35290);
#30028=AXIS2_PLACEMENT_3D('',#50115,#35296,#35297);
#30029=AXIS2_PLACEMENT_3D('',#50123,#35302,#35303);
#30030=AXIS2_PLACEMENT_3D('',#50129,#35307,#35308);
#30031=AXIS2_PLACEMENT_3D('',#50137,#35313,#35314);
#30032=AXIS2_PLACEMENT_3D('',#50141,#35317,#35318);
#30033=AXIS2_PLACEMENT_3D('',#50147,#35322,#35323);
#30034=AXIS2_PLACEMENT_3D('',#50158,#35329,#35330);
#30035=AXIS2_PLACEMENT_3D('',#50172,#35338,#35339);
#30036=AXIS2_PLACEMENT_3D('',#50176,#35342,#35343);
#30037=AXIS2_PLACEMENT_3D('',#50185,#35349,#35350);
#30038=AXIS2_PLACEMENT_3D('',#50191,#35354,#35355);
#30039=AXIS2_PLACEMENT_3D('',#50195,#35358,#35359);
#30040=AXIS2_PLACEMENT_3D('',#50202,#35364,#35365);
#30041=AXIS2_PLACEMENT_3D('',#50206,#35368,#35369);
#30042=AXIS2_PLACEMENT_3D('',#50210,#35372,#35373);
#30043=AXIS2_PLACEMENT_3D('',#50220,#35379,#35380);
#30044=AXIS2_PLACEMENT_3D('',#50230,#35386,#35387);
#30045=AXIS2_PLACEMENT_3D('',#50238,#35392,#35393);
#30046=AXIS2_PLACEMENT_3D('',#50244,#35397,#35398);
#30047=AXIS2_PLACEMENT_3D('',#50252,#35403,#35404);
#30048=AXIS2_PLACEMENT_3D('',#50258,#35408,#35409);
#30049=AXIS2_PLACEMENT_3D('',#50263,#35411,#35412);
#30050=AXIS2_PLACEMENT_3D('',#50266,#35414,#35415);
#30051=AXIS2_PLACEMENT_3D('',#50267,#35416,#35417);
#30052=AXIS2_PLACEMENT_3D('',#50273,#35421,#35422);
#30053=AXIS2_PLACEMENT_3D('',#50277,#35424,#35425);
#30054=AXIS2_PLACEMENT_3D('',#50278,#35426,#35427);
#30055=AXIS2_PLACEMENT_3D('',#50279,#35428,#35429);
#30056=AXIS2_PLACEMENT_3D('',#50285,#35433,#35434);
#30057=AXIS2_PLACEMENT_3D('',#50289,#35436,#35437);
#30058=AXIS2_PLACEMENT_3D('',#50290,#35438,#35439);
#30059=AXIS2_PLACEMENT_3D('',#50291,#35440,#35441);
#30060=AXIS2_PLACEMENT_3D('',#50297,#35445,#35446);
#30061=AXIS2_PLACEMENT_3D('',#50301,#35448,#35449);
#30062=AXIS2_PLACEMENT_3D('',#50302,#35450,#35451);
#30063=AXIS2_PLACEMENT_3D('',#50303,#35452,#35453);
#30064=AXIS2_PLACEMENT_3D('',#50306,#35456,#35457);
#30065=AXIS2_PLACEMENT_3D('',#50312,#35461,#35462);
#30066=AXIS2_PLACEMENT_3D('',#50315,#35464,#35465);
#30067=AXIS2_PLACEMENT_3D('',#50316,#35466,#35467);
#30068=AXIS2_PLACEMENT_3D('',#50320,#35470,#35471);
#30069=AXIS2_PLACEMENT_3D('',#50323,#35473,#35474);
#30070=AXIS2_PLACEMENT_3D('',#50324,#35475,#35476);
#30071=AXIS2_PLACEMENT_3D('',#50326,#35477,#35478);
#30072=AXIS2_PLACEMENT_3D('',#50328,#35479,#35480);
#30073=AXIS2_PLACEMENT_3D('',#50329,#35481,#35482);
#30074=AXIS2_PLACEMENT_3D('',#50333,#35485,#35486);
#30075=AXIS2_PLACEMENT_3D('',#50337,#35489,#35490);
#30076=AXIS2_PLACEMENT_3D('',#50343,#35494,#35495);
#30077=AXIS2_PLACEMENT_3D('',#50345,#35497,#35498);
#30078=AXIS2_PLACEMENT_3D('',#50352,#35502,#35503);
#30079=AXIS2_PLACEMENT_3D('',#50354,#35504,#35505);
#30080=AXIS2_PLACEMENT_3D('',#50355,#35506,#35507);
#30081=AXIS2_PLACEMENT_3D('',#50358,#35510,#35511);
#30082=AXIS2_PLACEMENT_3D('',#50359,#35512,#35513);
#30083=AXIS2_PLACEMENT_3D('',#50367,#35518,#35519);
#30084=AXIS2_PLACEMENT_3D('',#50369,#35521,#35522);
#30085=AXIS2_PLACEMENT_3D('',#50373,#35525,#35526);
#30086=AXIS2_PLACEMENT_3D('',#50375,#35527,#35528);
#30087=AXIS2_PLACEMENT_3D('',#50376,#35529,#35530);
#30088=AXIS2_PLACEMENT_3D('',#50380,#35533,#35534);
#30089=AXIS2_PLACEMENT_3D('',#50384,#35537,#35538);
#30090=AXIS2_PLACEMENT_3D('',#50386,#35540,#35541);
#30091=AXIS2_PLACEMENT_3D('',#50388,#35542,#35543);
#30092=AXIS2_PLACEMENT_3D('',#50391,#35545,#35546);
#30093=AXIS2_PLACEMENT_3D('',#50392,#35547,#35548);
#30094=AXIS2_PLACEMENT_3D('',#50394,#35549,#35550);
#30095=AXIS2_PLACEMENT_3D('',#50396,#35552,#35553);
#30096=AXIS2_PLACEMENT_3D('',#50399,#35555,#35556);
#30097=AXIS2_PLACEMENT_3D('',#50400,#35557,#35558);
#30098=AXIS2_PLACEMENT_3D('',#50402,#35560,#35561);
#30099=AXIS2_PLACEMENT_3D('',#50405,#35563,#35564);
#30100=AXIS2_PLACEMENT_3D('',#50406,#35565,#35566);
#30101=AXIS2_PLACEMENT_3D('',#50408,#35567,#35568);
#30102=AXIS2_PLACEMENT_3D('',#50410,#35570,#35571);
#30103=AXIS2_PLACEMENT_3D('',#50412,#35572,#35573);
#30104=AXIS2_PLACEMENT_3D('',#50414,#35575,#35576);
#30105=AXIS2_PLACEMENT_3D('',#50417,#35578,#35579);
#30106=AXIS2_PLACEMENT_3D('',#50418,#35580,#35581);
#30107=AXIS2_PLACEMENT_3D('',#50421,#35583,#35584);
#30108=AXIS2_PLACEMENT_3D('',#50422,#35585,#35586);
#30109=AXIS2_PLACEMENT_3D('',#50424,#35587,#35588);
#30110=AXIS2_PLACEMENT_3D('',#50426,#35590,#35591);
#30111=AXIS2_PLACEMENT_3D('',#50428,#35593,#35594);
#30112=AXIS2_PLACEMENT_3D('',#50431,#35596,#35597);
#30113=AXIS2_PLACEMENT_3D('',#50432,#35598,#35599);
#30114=AXIS2_PLACEMENT_3D('',#50434,#35600,#35601);
#30115=AXIS2_PLACEMENT_3D('',#50436,#35603,#35604);
#30116=AXIS2_PLACEMENT_3D('',#50438,#35606,#35607);
#30117=AXIS2_PLACEMENT_3D('',#50441,#35609,#35610);
#30118=AXIS2_PLACEMENT_3D('',#50442,#35611,#35612);
#30119=AXIS2_PLACEMENT_3D('',#50445,#35614,#35615);
#30120=AXIS2_PLACEMENT_3D('',#50446,#35616,#35617);
#30121=AXIS2_PLACEMENT_3D('',#50449,#35619,#35620);
#30122=AXIS2_PLACEMENT_3D('',#50450,#35621,#35622);
#30123=AXIS2_PLACEMENT_3D('',#50453,#35624,#35625);
#30124=AXIS2_PLACEMENT_3D('',#50454,#35626,#35627);
#30125=AXIS2_PLACEMENT_3D('',#50460,#35631,#35632);
#30126=AXIS2_PLACEMENT_3D('',#50464,#35634,#35635);
#30127=AXIS2_PLACEMENT_3D('',#50465,#35636,#35637);
#30128=AXIS2_PLACEMENT_3D('',#50466,#35638,#35639);
#30129=AXIS2_PLACEMENT_3D('',#50472,#35643,#35644);
#30130=AXIS2_PLACEMENT_3D('',#50476,#35646,#35647);
#30131=AXIS2_PLACEMENT_3D('',#50477,#35648,#35649);
#30132=AXIS2_PLACEMENT_3D('',#50478,#35650,#35651);
#30133=AXIS2_PLACEMENT_3D('',#50481,#35654,#35655);
#30134=AXIS2_PLACEMENT_3D('',#50487,#35658,#35659);
#30135=AXIS2_PLACEMENT_3D('',#50491,#35661,#35662);
#30136=AXIS2_PLACEMENT_3D('',#50494,#35664,#35665);
#30137=AXIS2_PLACEMENT_3D('',#50496,#35666,#35667);
#30138=AXIS2_PLACEMENT_3D('',#50497,#35668,#35669);
#30139=AXIS2_PLACEMENT_3D('',#50501,#35672,#35673);
#30140=AXIS2_PLACEMENT_3D('',#50504,#35675,#35676);
#30141=AXIS2_PLACEMENT_3D('',#50505,#35677,#35678);
#30142=AXIS2_PLACEMENT_3D('',#50509,#35681,#35682);
#30143=AXIS2_PLACEMENT_3D('',#50512,#35684,#35685);
#30144=AXIS2_PLACEMENT_3D('',#50513,#35686,#35687);
#30145=AXIS2_PLACEMENT_3D('',#50517,#35690,#35691);
#30146=AXIS2_PLACEMENT_3D('',#50519,#35693,#35694);
#30147=AXIS2_PLACEMENT_3D('',#50521,#35696,#35697);
#30148=AXIS2_PLACEMENT_3D('',#50523,#35699,#35700);
#30149=AXIS2_PLACEMENT_3D('',#50527,#35703,#35704);
#30150=AXIS2_PLACEMENT_3D('',#50529,#35706,#35707);
#30151=AXIS2_PLACEMENT_3D('',#50532,#35710,#35711);
#30152=AXIS2_PLACEMENT_3D('',#50534,#35713,#35714);
#30153=AXIS2_PLACEMENT_3D('',#50536,#35716,#35717);
#30154=AXIS2_PLACEMENT_3D('',#50538,#35719,#35720);
#30155=AXIS2_PLACEMENT_3D('',#50541,#35722,#35723);
#30156=AXIS2_PLACEMENT_3D('',#50542,#35724,#35725);
#30157=AXIS2_PLACEMENT_3D('',#50546,#35728,#35729);
#30158=AXIS2_PLACEMENT_3D('',#50549,#35731,#35732);
#30159=AXIS2_PLACEMENT_3D('',#50550,#35733,#35734);
#30160=AXIS2_PLACEMENT_3D('',#50552,#35736,#35737);
#30161=AXIS2_PLACEMENT_3D('',#50555,#35740,#35741);
#30162=AXIS2_PLACEMENT_3D('',#50557,#35743,#35744);
#30163=AXIS2_PLACEMENT_3D('',#50558,#35745,#35746);
#30164=AXIS2_PLACEMENT_3D('',#50559,#35747,#35748);
#30165=AXIS2_PLACEMENT_3D('',#50560,#35749,#35750);
#30166=AXIS2_PLACEMENT_3D('',#50562,#35751,#35752);
#30167=AXIS2_PLACEMENT_3D('',#50563,#35753,#35754);
#30168=AXIS2_PLACEMENT_3D('',#50772,#35755,#35756);
#30169=AXIS2_PLACEMENT_3D('',#50773,#35757,#35758);
#30170=AXIS2_PLACEMENT_3D('',#50774,#35759,#35760);
#30171=AXIS2_PLACEMENT_3D('',#50775,#35761,#35762);
#30172=AXIS2_PLACEMENT_3D('',#50776,#35763,#35764);
#30173=AXIS2_PLACEMENT_3D('',#50777,#35765,#35766);
#30174=AXIS2_PLACEMENT_3D('',#50778,#35767,#35768);
#30175=AXIS2_PLACEMENT_3D('',#50779,#35769,#35770);
#30176=AXIS2_PLACEMENT_3D('',#50781,#35771,#35772);
#30177=AXIS2_PLACEMENT_3D('',#50782,#35773,#35774);
#30178=AXIS2_PLACEMENT_3D('',#50785,#35775,#35776);
#30179=AXIS2_PLACEMENT_3D('',#50943,#35777,#35778);
#30180=AXIS2_PLACEMENT_3D('',#50946,#35780,#35781);
#30181=AXIS2_PLACEMENT_3D('',#50947,#35782,#35783);
#30182=AXIS2_PLACEMENT_3D('',#50948,#35784,#35785);
#30183=AXIS2_PLACEMENT_3D('',#50949,#35786,#35787);
#30184=AXIS2_PLACEMENT_3D('',#56990,#35788,#35789);
#30185=AXIS2_PLACEMENT_3D('',#56991,#35790,#35791);
#30186=AXIS2_PLACEMENT_3D('',#57007,#35793,#35794);
#30187=AXIS2_PLACEMENT_3D('',#57018,#35795,#35796);
#30188=AXIS2_PLACEMENT_3D('',#57066,#35798,#35799);
#30189=AXIS2_PLACEMENT_3D('',#57114,#35801,#35802);
#30190=AXIS2_PLACEMENT_3D('',#57168,#35804,#35805);
#30191=AXIS2_PLACEMENT_3D('',#57216,#35807,#35808);
#30192=AXIS2_PLACEMENT_3D('',#57264,#35810,#35811);
#30193=AXIS2_PLACEMENT_3D('',#57318,#35813,#35814);
#30194=AXIS2_PLACEMENT_3D('',#57366,#35816,#35817);
#30195=AXIS2_PLACEMENT_3D('',#57414,#35819,#35820);
#30196=AXIS2_PLACEMENT_3D('',#57468,#35822,#35823);
#30197=AXIS2_PLACEMENT_3D('',#57516,#35825,#35826);
#30198=AXIS2_PLACEMENT_3D('',#57527,#35828,#35829);
#30199=AXIS2_PLACEMENT_3D('',#57532,#35830,#35831);
#30200=AXIS2_PLACEMENT_3D('',#57557,#35833,#35834);
#30201=AXIS2_PLACEMENT_3D('',#57582,#35836,#35837);
#30202=AXIS2_PLACEMENT_3D('',#57607,#35839,#35840);
#30203=AXIS2_PLACEMENT_3D('',#57631,#35842,#35843);
#30204=AXIS2_PLACEMENT_3D('',#57656,#35845,#35846);
#30205=AXIS2_PLACEMENT_3D('',#57681,#35848,#35849);
#30206=AXIS2_PLACEMENT_3D('',#57705,#35851,#35852);
#30207=AXIS2_PLACEMENT_3D('',#57730,#35854,#35855);
#30208=AXIS2_PLACEMENT_3D('',#57755,#35857,#35858);
#30209=AXIS2_PLACEMENT_3D('',#57779,#35860,#35861);
#30210=AXIS2_PLACEMENT_3D('',#57782,#35862,#35863);
#30211=AXIS2_PLACEMENT_3D('',#57838,#35864,#35865);
#30212=AXIS2_PLACEMENT_3D('',#57839,#35866,#35867);
#30213=AXIS2_PLACEMENT_3D('',#57894,#35868,#35869);
#30214=AXIS2_PLACEMENT_3D('',#57896,#35870,#35871);
#30215=AXIS2_PLACEMENT_3D('',#57897,#35872,#35873);
#30216=AXIS2_PLACEMENT_3D('',#57898,#35874,#35875);
#30217=AXIS2_PLACEMENT_3D('',#57899,#35876,#35877);
#30218=AXIS2_PLACEMENT_3D('',#57900,#35878,#35879);
#30219=AXIS2_PLACEMENT_3D('',#57901,#35880,#35881);
#30220=AXIS2_PLACEMENT_3D('',#57902,#35882,#35883);
#30221=AXIS2_PLACEMENT_3D('',#57903,#35884,#35885);
#30222=AXIS2_PLACEMENT_3D('',#57904,#35886,#35887);
#30223=AXIS2_PLACEMENT_3D('',#57905,#35888,#35889);
#30224=AXIS2_PLACEMENT_3D('',#57907,#35890,#35891);
#30225=AXIS2_PLACEMENT_3D('',#58044,#35892,#35893);
#30226=AXIS2_PLACEMENT_3D('',#58045,#35894,#35895);
#30227=AXIS2_PLACEMENT_3D('',#58047,#35896,#35897);
#30228=AXIS2_PLACEMENT_3D('',#58049,#35899,#35900);
#30229=AXIS2_PLACEMENT_3D('',#58448,#35902,#35903);
#30230=AXIS2_PLACEMENT_3D('',#58459,#35904,#35905);
#30231=AXIS2_PLACEMENT_3D('',#58844,#35906,#35907);
#30232=AXIS2_PLACEMENT_3D('',#58846,#35908,#35909);
#30233=AXIS2_PLACEMENT_3D('',#58847,#35910,#35911);
#30234=AXIS2_PLACEMENT_3D('',#58848,#35912,#35913);
#30235=AXIS2_PLACEMENT_3D('',#58850,#35914,#35915);
#30236=AXIS2_PLACEMENT_3D('',#58851,#35916,#35917);
#30237=AXIS2_PLACEMENT_3D('',#58853,#35919,#35920);
#30238=AXIS2_PLACEMENT_3D('',#58854,#35921,#35922);
#30239=AXIS2_PLACEMENT_3D('',#58855,#35923,#35924);
#30240=AXIS2_PLACEMENT_3D('',#58868,#35931,#35932);
#30241=AXIS2_PLACEMENT_3D('',#58874,#35936,#35937);
#30242=AXIS2_PLACEMENT_3D('',#58882,#35942,#35943);
#30243=AXIS2_PLACEMENT_3D('',#58890,#35948,#35949);
#30244=AXIS2_PLACEMENT_3D('',#58906,#35958,#35959);
#30245=AXIS2_PLACEMENT_3D('',#58910,#35962,#35963);
#30246=AXIS2_PLACEMENT_3D('',#58918,#35968,#35969);
#30247=AXIS2_PLACEMENT_3D('',#58924,#35973,#35974);
#30248=AXIS2_PLACEMENT_3D('',#58930,#35978,#35979);
#30249=AXIS2_PLACEMENT_3D('',#58943,#35986,#35987);
#30250=AXIS2_PLACEMENT_3D('',#58949,#35991,#35992);
#30251=AXIS2_PLACEMENT_3D('',#58954,#35996,#35997);
#30252=AXIS2_PLACEMENT_3D('',#58956,#35999,#36000);
#30253=AXIS2_PLACEMENT_3D('',#58960,#36003,#36004);
#30254=AXIS2_PLACEMENT_3D('',#58968,#36009,#36010);
#30255=AXIS2_PLACEMENT_3D('',#58974,#36014,#36015);
#30256=AXIS2_PLACEMENT_3D('',#58978,#36018,#36019);
#30257=AXIS2_PLACEMENT_3D('',#58982,#36022,#36023);
#30258=AXIS2_PLACEMENT_3D('',#58985,#36026,#36027);
#30259=AXIS2_PLACEMENT_3D('',#58993,#36032,#36033);
#30260=AXIS2_PLACEMENT_3D('',#58999,#36037,#36038);
#30261=AXIS2_PLACEMENT_3D('',#59000,#36039,#36040);
#30262=AXIS2_PLACEMENT_3D('',#59005,#36044,#36045);
#30263=AXIS2_PLACEMENT_3D('',#59011,#36049,#36050);
#30264=AXIS2_PLACEMENT_3D('',#59017,#36054,#36055);
#30265=AXIS2_PLACEMENT_3D('',#59023,#36059,#36060);
#30266=AXIS2_PLACEMENT_3D('',#59029,#36064,#36065);
#30267=AXIS2_PLACEMENT_3D('',#59031,#36067,#36068);
#30268=AXIS2_PLACEMENT_3D('',#59035,#36071,#36072);
#30269=AXIS2_PLACEMENT_3D('',#59038,#36075,#36076);
#30270=AXIS2_PLACEMENT_3D('',#59044,#36080,#36081);
#30271=AXIS2_PLACEMENT_3D('',#59048,#36084,#36085);
#30272=AXIS2_PLACEMENT_3D('',#59050,#36087,#36088);
#30273=AXIS2_PLACEMENT_3D('',#59054,#36091,#36092);
#30274=AXIS2_PLACEMENT_3D('',#59060,#36096,#36097);
#30275=AXIS2_PLACEMENT_3D('',#59063,#36100,#36101);
#30276=AXIS2_PLACEMENT_3D('',#59066,#36104,#36105);
#30277=AXIS2_PLACEMENT_3D('',#59068,#36107,#36108);
#30278=AXIS2_PLACEMENT_3D('',#59069,#36109,#36110);
#30279=AXIS2_PLACEMENT_3D('',#59070,#36111,#36112);
#30280=AXIS2_PLACEMENT_3D('',#59072,#36114,#36115);
#30281=AXIS2_PLACEMENT_3D('',#59073,#36116,#36117);
#30282=AXIS2_PLACEMENT_3D('',#59074,#36118,#36119);
#30283=AXIS2_PLACEMENT_3D('',#59076,#36121,#36122);
#30284=AXIS2_PLACEMENT_3D('',#59077,#36123,#36124);
#30285=AXIS2_PLACEMENT_3D('',#59078,#36125,#36126);
#30286=AXIS2_PLACEMENT_3D('',#59094,#36128,#36129);
#30287=AXIS2_PLACEMENT_3D('',#59105,#36130,#36131);
#30288=AXIS2_PLACEMENT_3D('',#59171,#36133,#36134);
#30289=AXIS2_PLACEMENT_3D('',#59231,#36136,#36137);
#30290=AXIS2_PLACEMENT_3D('',#59291,#36139,#36140);
#30291=AXIS2_PLACEMENT_3D('',#59354,#36142,#36143);
#30292=AXIS2_PLACEMENT_3D('',#59414,#36145,#36146);
#30293=AXIS2_PLACEMENT_3D('',#59474,#36148,#36149);
#30294=AXIS2_PLACEMENT_3D('',#59537,#36151,#36152);
#30295=AXIS2_PLACEMENT_3D('',#59597,#36154,#36155);
#30296=AXIS2_PLACEMENT_3D('',#59663,#36157,#36158);
#30297=AXIS2_PLACEMENT_3D('',#59732,#36160,#36161);
#30298=AXIS2_PLACEMENT_3D('',#59798,#36163,#36164);
#30299=AXIS2_PLACEMENT_3D('',#59858,#36166,#36167);
#30300=AXIS2_PLACEMENT_3D('',#59921,#36169,#36170);
#30301=AXIS2_PLACEMENT_3D('',#59987,#36172,#36173);
#30302=AXIS2_PLACEMENT_3D('',#60047,#36175,#36176);
#30303=AXIS2_PLACEMENT_3D('',#60101,#36178,#36179);
#30304=AXIS2_PLACEMENT_3D('',#60155,#36181,#36182);
#30305=AXIS2_PLACEMENT_3D('',#60215,#36184,#36185);
#30306=AXIS2_PLACEMENT_3D('',#60281,#36187,#36188);
#30307=AXIS2_PLACEMENT_3D('',#60347,#36190,#36191);
#30308=AXIS2_PLACEMENT_3D('',#60416,#36193,#36194);
#30309=AXIS2_PLACEMENT_3D('',#60476,#36196,#36197);
#30310=AXIS2_PLACEMENT_3D('',#60539,#36199,#36200);
#30311=AXIS2_PLACEMENT_3D('',#60605,#36202,#36203);
#30312=AXIS2_PLACEMENT_3D('',#60671,#36205,#36206);
#30313=AXIS2_PLACEMENT_3D('',#60725,#36208,#36209);
#30314=AXIS2_PLACEMENT_3D('',#60779,#36211,#36212);
#30315=AXIS2_PLACEMENT_3D('',#60842,#36214,#36215);
#30316=AXIS2_PLACEMENT_3D('',#60908,#36217,#36218);
#30317=AXIS2_PLACEMENT_3D('',#60959,#36220,#36221);
#30318=AXIS2_PLACEMENT_3D('',#61022,#36223,#36224);
#30319=AXIS2_PLACEMENT_3D('',#61076,#36226,#36227);
#30320=AXIS2_PLACEMENT_3D('',#61139,#36229,#36230);
#30321=AXIS2_PLACEMENT_3D('',#61208,#36232,#36233);
#30322=AXIS2_PLACEMENT_3D('',#61271,#36235,#36236);
#30323=AXIS2_PLACEMENT_3D('',#61325,#36238,#36239);
#30324=AXIS2_PLACEMENT_3D('',#61385,#36241,#36242);
#30325=AXIS2_PLACEMENT_3D('',#61445,#36244,#36245);
#30326=AXIS2_PLACEMENT_3D('',#61505,#36247,#36248);
#30327=AXIS2_PLACEMENT_3D('',#61568,#36250,#36251);
#30328=AXIS2_PLACEMENT_3D('',#61622,#36253,#36254);
#30329=AXIS2_PLACEMENT_3D('',#61676,#36256,#36257);
#30330=AXIS2_PLACEMENT_3D('',#61742,#36259,#36260);
#30331=AXIS2_PLACEMENT_3D('',#61811,#36262,#36263);
#30332=AXIS2_PLACEMENT_3D('',#61874,#36265,#36266);
#30333=AXIS2_PLACEMENT_3D('',#61928,#36268,#36269);
#30334=AXIS2_PLACEMENT_3D('',#61994,#36271,#36272);
#30335=AXIS2_PLACEMENT_3D('',#62060,#36274,#36275);
#30336=AXIS2_PLACEMENT_3D('',#62120,#36277,#36278);
#30337=AXIS2_PLACEMENT_3D('',#62180,#36280,#36281);
#30338=AXIS2_PLACEMENT_3D('',#62234,#36283,#36284);
#30339=AXIS2_PLACEMENT_3D('',#62291,#36286,#36287);
#30340=AXIS2_PLACEMENT_3D('',#62357,#36289,#36290);
#30341=AXIS2_PLACEMENT_3D('',#62426,#36292,#36293);
#30342=AXIS2_PLACEMENT_3D('',#62489,#36295,#36296);
#30343=AXIS2_PLACEMENT_3D('',#62543,#36298,#36299);
#30344=AXIS2_PLACEMENT_3D('',#62609,#36301,#36302);
#30345=AXIS2_PLACEMENT_3D('',#62675,#36304,#36305);
#30346=AXIS2_PLACEMENT_3D('',#62680,#36307,#36308);
#30347=AXIS2_PLACEMENT_3D('',#62734,#36309,#36310);
#30348=AXIS2_PLACEMENT_3D('',#62756,#36312,#36313);
#30349=AXIS2_PLACEMENT_3D('',#62765,#36314,#36315);
#30350=AXIS2_PLACEMENT_3D('',#62795,#36317,#36318);
#30351=AXIS2_PLACEMENT_3D('',#62825,#36320,#36321);
#30352=AXIS2_PLACEMENT_3D('',#62870,#36323,#36324);
#30353=AXIS2_PLACEMENT_3D('',#62915,#36326,#36327);
#30354=AXIS2_PLACEMENT_3D('',#62945,#36329,#36330);
#30355=AXIS2_PLACEMENT_3D('',#62975,#36332,#36333);
#30356=AXIS2_PLACEMENT_3D('',#63004,#36335,#36336);
#30357=AXIS2_PLACEMENT_3D('',#63046,#36338,#36339);
#30358=AXIS2_PLACEMENT_3D('',#63076,#36341,#36342);
#30359=AXIS2_PLACEMENT_3D('',#63118,#36344,#36345);
#30360=AXIS2_PLACEMENT_3D('',#63148,#36347,#36348);
#30361=AXIS2_PLACEMENT_3D('',#63178,#36350,#36351);
#30362=AXIS2_PLACEMENT_3D('',#63220,#36353,#36354);
#30363=AXIS2_PLACEMENT_3D('',#63262,#36356,#36357);
#30364=AXIS2_PLACEMENT_3D('',#63292,#36359,#36360);
#30365=AXIS2_PLACEMENT_3D('',#63322,#36362,#36363);
#30366=AXIS2_PLACEMENT_3D('',#63364,#36365,#36366);
#30367=AXIS2_PLACEMENT_3D('',#63418,#36368,#36369);
#30368=AXIS2_PLACEMENT_3D('',#63448,#36371,#36372);
#30369=AXIS2_PLACEMENT_3D('',#63490,#36374,#36375);
#30370=AXIS2_PLACEMENT_3D('',#63519,#36377,#36378);
#30371=AXIS2_PLACEMENT_3D('',#63549,#36380,#36381);
#30372=AXIS2_PLACEMENT_3D('',#63592,#36383,#36384);
#30373=AXIS2_PLACEMENT_3D('',#63634,#36386,#36387);
#30374=AXIS2_PLACEMENT_3D('',#63664,#36389,#36390);
#30375=AXIS2_PLACEMENT_3D('',#63693,#36392,#36393);
#30376=AXIS2_PLACEMENT_3D('',#63735,#36395,#36396);
#30377=AXIS2_PLACEMENT_3D('',#63792,#36398,#36399);
#30378=AXIS2_PLACEMENT_3D('',#63821,#36401,#36402);
#30379=AXIS2_PLACEMENT_3D('',#63848,#36404,#36405);
#30380=AXIS2_PLACEMENT_3D('',#63877,#36407,#36408);
#30381=AXIS2_PLACEMENT_3D('',#63922,#36410,#36411);
#30382=AXIS2_PLACEMENT_3D('',#63965,#36413,#36414);
#30383=AXIS2_PLACEMENT_3D('',#64010,#36416,#36417);
#30384=AXIS2_PLACEMENT_3D('',#64040,#36419,#36420);
#30385=AXIS2_PLACEMENT_3D('',#64070,#36422,#36423);
#30386=AXIS2_PLACEMENT_3D('',#64099,#36425,#36426);
#30387=AXIS2_PLACEMENT_3D('',#64145,#36428,#36429);
#30388=AXIS2_PLACEMENT_3D('',#64175,#36431,#36432);
#30389=AXIS2_PLACEMENT_3D('',#64205,#36434,#36435);
#30390=AXIS2_PLACEMENT_3D('',#64234,#36437,#36438);
#30391=AXIS2_PLACEMENT_3D('',#64276,#36440,#36441);
#30392=AXIS2_PLACEMENT_3D('',#64319,#36443,#36444);
#30393=AXIS2_PLACEMENT_3D('',#64361,#36446,#36447);
#30394=AXIS2_PLACEMENT_3D('',#64391,#36449,#36450);
#30395=AXIS2_PLACEMENT_3D('',#64421,#36452,#36453);
#30396=AXIS2_PLACEMENT_3D('',#64450,#36455,#36456);
#30397=AXIS2_PLACEMENT_3D('',#64492,#36458,#36459);
#30398=AXIS2_PLACEMENT_3D('',#64523,#36461,#36462);
#30399=AXIS2_PLACEMENT_3D('',#64553,#36464,#36465);
#30400=AXIS2_PLACEMENT_3D('',#64595,#36467,#36468);
#30401=AXIS2_PLACEMENT_3D('',#64637,#36470,#36471);
#30402=AXIS2_PLACEMENT_3D('',#64668,#36473,#36474);
#30403=AXIS2_PLACEMENT_3D('',#64710,#36476,#36477);
#30404=AXIS2_PLACEMENT_3D('',#64740,#36479,#36480);
#30405=AXIS2_PLACEMENT_3D('',#64769,#36482,#36483);
#30406=AXIS2_PLACEMENT_3D('',#64799,#36485,#36486);
#30407=AXIS2_PLACEMENT_3D('',#65336,#36521,#36522);
#30408=AXIS2_PLACEMENT_3D('',#65337,#36523,#36524);
#30409=AXIS2_PLACEMENT_3D('',#65346,#36529,#36530);
#30410=AXIS2_PLACEMENT_3D('',#65352,#36534,#36535);
#30411=AXIS2_PLACEMENT_3D('',#65358,#36539,#36540);
#30412=AXIS2_PLACEMENT_3D('',#65361,#36543,#36544);
#30413=AXIS2_PLACEMENT_3D('',#65857,#36578,#36579);
#30414=AXIS2_PLACEMENT_3D('',#65858,#36580,#36581);
#30415=AXIS2_PLACEMENT_3D('',#65859,#36582,#36583);
#30416=AXIS2_PLACEMENT_3D('',#65860,#36584,#36585);
#30417=AXIS2_PLACEMENT_3D('',#65861,#36586,#36587);
#30418=AXIS2_PLACEMENT_3D('',#65862,#36588,#36589);
#30419=AXIS2_PLACEMENT_3D('',#65937,#36590,#36591);
#30420=AXIS2_PLACEMENT_3D('',#65939,#36592,#36593);
#30421=AXIS2_PLACEMENT_3D('',#68257,#36594,#36595);
#30422=AXIS2_PLACEMENT_3D('',#68259,#36596,#36597);
#30423=AXIS2_PLACEMENT_3D('',#68260,#36598,#36599);
#30424=AXIS2_PLACEMENT_3D('',#68338,#36600,#36601);
#30425=AXIS2_PLACEMENT_3D('',#68339,#36602,#36603);
#30426=AXIS2_PLACEMENT_3D('',#70502,#36604,#36605);
#30427=AXIS2_PLACEMENT_3D('',#70504,#36606,#36607);
#30428=AXIS2_PLACEMENT_3D('',#70505,#36608,#36609);
#30429=AXIS2_PLACEMENT_3D('',#70506,#36610,#36611);
#30430=AXIS2_PLACEMENT_3D('',#70507,#36612,#36613);
#30431=AXIS2_PLACEMENT_3D('',#70520,#36620,#36621);
#30432=AXIS2_PLACEMENT_3D('',#70521,#36622,#36623);
#30433=AXIS2_PLACEMENT_3D('',#70545,#36625,#36626);
#30434=AXIS2_PLACEMENT_3D('',#70553,#36627,#36628);
#30435=AXIS2_PLACEMENT_3D('',#70556,#36631,#36632);
#30436=AXIS2_PLACEMENT_3D('',#70558,#36634,#36635);
#30437=AXIS2_PLACEMENT_3D('',#70560,#36637,#36638);
#30438=AXIS2_PLACEMENT_3D('',#70562,#36640,#36641);
#30439=AXIS2_PLACEMENT_3D('',#70564,#36643,#36644);
#30440=AXIS2_PLACEMENT_3D('',#70565,#36645,#36646);
#30441=AXIS2_PLACEMENT_3D('',#70566,#36647,#36648);
#30442=AXIS2_PLACEMENT_3D('',#70568,#36649,#36650);
#30443=AXIS2_PLACEMENT_3D('',#70569,#36651,#36652);
#30444=AXIS2_PLACEMENT_3D('',#70571,#36654,#36655);
#30445=AXIS2_PLACEMENT_3D('',#70572,#36656,#36657);
#30446=AXIS2_PLACEMENT_3D('',#70574,#36658,#36659);
#30447=AXIS2_PLACEMENT_3D('',#70577,#36661,#36662);
#30448=AXIS2_PLACEMENT_3D('',#70578,#36663,#36664);
#30449=AXIS2_PLACEMENT_3D('',#70580,#36665,#36666);
#30450=AXIS2_PLACEMENT_3D('',#70582,#36668,#36669);
#30451=AXIS2_PLACEMENT_3D('',#70584,#36670,#36671);
#30452=AXIS2_PLACEMENT_3D('',#70585,#36672,#36673);
#30453=AXIS2_PLACEMENT_3D('',#70587,#36674,#36675);
#30454=AXIS2_PLACEMENT_3D('',#70589,#36677,#36678);
#30455=AXIS2_PLACEMENT_3D('',#70591,#36679,#36680);
#30456=AXIS2_PLACEMENT_3D('',#70592,#36681,#36682);
#30457=AXIS2_PLACEMENT_3D('',#70622,#36684,#36685);
#30458=AXIS2_PLACEMENT_3D('',#70630,#36688,#36689);
#30459=AXIS2_PLACEMENT_3D('',#70636,#36691,#36692);
#30460=AXIS2_PLACEMENT_3D('',#70642,#36694,#36695);
#30461=AXIS2_PLACEMENT_3D('',#70659,#36697,#36698);
#30462=AXIS2_PLACEMENT_3D('',#70661,#36700,#36701);
#30463=AXIS2_PLACEMENT_3D('',#70663,#36703,#36704);
#30464=AXIS2_PLACEMENT_3D('',#70664,#36705,#36706);
#30465=AXIS2_PLACEMENT_3D('',#70665,#36707,#36708);
#30466=AXIS2_PLACEMENT_3D('',#70667,#36709,#36710);
#30467=AXIS2_PLACEMENT_3D('',#70670,#36712,#36713);
#30468=AXIS2_PLACEMENT_3D('',#70671,#36714,#36715);
#30469=AXIS2_PLACEMENT_3D('',#70673,#36716,#36717);
#30470=AXIS2_PLACEMENT_3D('',#70674,#36718,#36719);
#30471=AXIS2_PLACEMENT_3D('',#70676,#36720,#36721);
#30472=AXIS2_PLACEMENT_3D('',#70678,#36723,#36724);
#30473=AXIS2_PLACEMENT_3D('',#70680,#36725,#36726);
#30474=AXIS2_PLACEMENT_3D('',#70682,#36728,#36729);
#30475=AXIS2_PLACEMENT_3D('',#70684,#36730,#36731);
#30476=AXIS2_PLACEMENT_3D('',#70685,#36732,#36733);
#30477=AXIS2_PLACEMENT_3D('',#70687,#36735,#36736);
#30478=AXIS2_PLACEMENT_3D('',#70688,#36737,#36738);
#30479=AXIS2_PLACEMENT_3D('',#70690,#36739,#36740);
#30480=AXIS2_PLACEMENT_3D('',#70694,#36742,#36743);
#30481=AXIS2_PLACEMENT_3D('',#70695,#36744,#36745);
#30482=AXIS2_PLACEMENT_3D('',#70696,#36746,#36747);
#30483=AXIS2_PLACEMENT_3D('',#70700,#36749,#36750);
#30484=AXIS2_PLACEMENT_3D('',#70701,#36751,#36752);
#30485=AXIS2_PLACEMENT_3D('',#70702,#36753,#36754);
#30486=AXIS2_PLACEMENT_3D('',#70703,#36755,#36756);
#30487=AXIS2_PLACEMENT_3D('',#70707,#36758,#36759);
#30488=AXIS2_PLACEMENT_3D('',#70708,#36760,#36761);
#30489=AXIS2_PLACEMENT_3D('',#70709,#36762,#36763);
#30490=AXIS2_PLACEMENT_3D('',#70712,#36765,#36766);
#30491=AXIS2_PLACEMENT_3D('',#70713,#36767,#36768);
#30492=AXIS2_PLACEMENT_3D('',#70715,#36769,#36770);
#30493=AXIS2_PLACEMENT_3D('',#70718,#36772,#36773);
#30494=AXIS2_PLACEMENT_3D('',#70719,#36774,#36775);
#30495=AXIS2_PLACEMENT_3D('',#70721,#36776,#36777);
#30496=AXIS2_PLACEMENT_3D('',#70723,#36779,#36780);
#30497=AXIS2_PLACEMENT_3D('',#70730,#36783,#36784);
#30498=AXIS2_PLACEMENT_3D('',#70732,#36786,#36787);
#30499=AXIS2_PLACEMENT_3D('',#70734,#36788,#36789);
#30500=AXIS2_PLACEMENT_3D('',#70736,#36791,#36792);
#30501=AXIS2_PLACEMENT_3D('',#70743,#36795,#36796);
#30502=AXIS2_PLACEMENT_3D('',#70745,#36798,#36799);
#30503=AXIS2_PLACEMENT_3D('',#70748,#36800,#36801);
#30504=AXIS2_PLACEMENT_3D('',#70749,#36802,#36803);
#30505=AXIS2_PLACEMENT_3D('',#70752,#36805,#36806);
#30506=AXIS2_PLACEMENT_3D('',#70753,#36807,#36808);
#30507=AXIS2_PLACEMENT_3D('',#70755,#36809,#36810);
#30508=AXIS2_PLACEMENT_3D('',#70757,#36812,#36813);
#30509=AXIS2_PLACEMENT_3D('',#70759,#36814,#36815);
#30510=AXIS2_PLACEMENT_3D('',#70760,#36816,#36817);
#30511=AXIS2_PLACEMENT_3D('',#70762,#36818,#36819);
#30512=AXIS2_PLACEMENT_3D('',#70763,#36820,#36821);
#30513=AXIS2_PLACEMENT_3D('',#70765,#36822,#36823);
#30514=AXIS2_PLACEMENT_3D('',#70767,#36825,#36826);
#30515=AXIS2_PLACEMENT_3D('',#70769,#36827,#36828);
#30516=AXIS2_PLACEMENT_3D('',#70770,#36829,#36830);
#30517=AXIS2_PLACEMENT_3D('',#70773,#36832,#36833);
#30518=AXIS2_PLACEMENT_3D('',#70774,#36834,#36835);
#30519=AXIS2_PLACEMENT_3D('',#70776,#36836,#36837);
#30520=AXIS2_PLACEMENT_3D('',#70777,#36838,#36839);
#30521=AXIS2_PLACEMENT_3D('',#70779,#36840,#36841);
#30522=AXIS2_PLACEMENT_3D('',#70781,#36843,#36844);
#30523=AXIS2_PLACEMENT_3D('',#70783,#36845,#36846);
#30524=AXIS2_PLACEMENT_3D('',#70784,#36847,#36848);
#30525=AXIS2_PLACEMENT_3D('',#70787,#36850,#36851);
#30526=AXIS2_PLACEMENT_3D('',#70788,#36852,#36853);
#30527=AXIS2_PLACEMENT_3D('',#70790,#36854,#36855);
#30528=AXIS2_PLACEMENT_3D('',#70791,#36856,#36857);
#30529=AXIS2_PLACEMENT_3D('',#70793,#36858,#36859);
#30530=AXIS2_PLACEMENT_3D('',#70795,#36861,#36862);
#30531=AXIS2_PLACEMENT_3D('',#70796,#36863,#36864);
#30532=AXIS2_PLACEMENT_3D('',#70798,#36865,#36866);
#30533=AXIS2_PLACEMENT_3D('',#70809,#36873,#36874);
#30534=AXIS2_PLACEMENT_3D('',#70811,#36875,#36876);
#30535=AXIS2_PLACEMENT_3D('',#70813,#36878,#36879);
#30536=AXIS2_PLACEMENT_3D('',#70815,#36880,#36881);
#30537=AXIS2_PLACEMENT_3D('',#70817,#36883,#36884);
#30538=AXIS2_PLACEMENT_3D('',#70819,#36885,#36886);
#30539=AXIS2_PLACEMENT_3D('',#70821,#36888,#36889);
#30540=AXIS2_PLACEMENT_3D('',#70823,#36890,#36891);
#30541=AXIS2_PLACEMENT_3D('',#70824,#36892,#36893);
#30542=AXIS2_PLACEMENT_3D('',#70826,#36895,#36896);
#30543=AXIS2_PLACEMENT_3D('',#70830,#36899,#36900);
#30544=AXIS2_PLACEMENT_3D('',#70834,#36903,#36904);
#30545=AXIS2_PLACEMENT_3D('',#70836,#36906,#36907);
#30546=AXIS2_PLACEMENT_3D('',#70839,#36909,#36910);
#30547=AXIS2_PLACEMENT_3D('',#70840,#36911,#36912);
#30548=AXIS2_PLACEMENT_3D('',#70842,#36914,#36915);
#30549=AXIS2_PLACEMENT_3D('',#70844,#36916,#36917);
#30550=AXIS2_PLACEMENT_3D('',#70846,#36919,#36920);
#30551=AXIS2_PLACEMENT_3D('',#70849,#36923,#36924);
#30552=AXIS2_PLACEMENT_3D('',#70850,#36925,#36926);
#30553=AXIS2_PLACEMENT_3D('',#70851,#36927,#36928);
#30554=AXIS2_PLACEMENT_3D('',#70852,#36929,#36930);
#30555=AXIS2_PLACEMENT_3D('',#70854,#36931,#36932);
#30556=AXIS2_PLACEMENT_3D('',#70857,#36934,#36935);
#30557=AXIS2_PLACEMENT_3D('',#70858,#36936,#36937);
#30558=AXIS2_PLACEMENT_3D('',#70868,#36942,#36943);
#30559=AXIS2_PLACEMENT_3D('',#70870,#36944,#36945);
#30560=AXIS2_PLACEMENT_3D('',#70872,#36946,#36947);
#30561=AXIS2_PLACEMENT_3D('',#70874,#36948,#36949);
#30562=AXIS2_PLACEMENT_3D('',#70876,#36950,#36951);
#30563=AXIS2_PLACEMENT_3D('',#70878,#36952,#36953);
#30564=AXIS2_PLACEMENT_3D('',#70880,#36954,#36955);
#30565=AXIS2_PLACEMENT_3D('',#70882,#36956,#36957);
#30566=AXIS2_PLACEMENT_3D('',#70884,#36958,#36959);
#30567=AXIS2_PLACEMENT_3D('',#70886,#36960,#36961);
#30568=AXIS2_PLACEMENT_3D('',#70887,#36962,#36963);
#30569=AXIS2_PLACEMENT_3D('',#70890,#36965,#36966);
#30570=AXIS2_PLACEMENT_3D('',#70891,#36967,#36968);
#30571=AXIS2_PLACEMENT_3D('',#70894,#36970,#36971);
#30572=AXIS2_PLACEMENT_3D('',#70895,#36972,#36973);
#30573=AXIS2_PLACEMENT_3D('',#70898,#36975,#36976);
#30574=AXIS2_PLACEMENT_3D('',#70899,#36977,#36978);
#30575=AXIS2_PLACEMENT_3D('',#70902,#36980,#36981);
#30576=AXIS2_PLACEMENT_3D('',#70903,#36982,#36983);
#30577=AXIS2_PLACEMENT_3D('',#70906,#36985,#36986);
#30578=AXIS2_PLACEMENT_3D('',#70907,#36987,#36988);
#30579=AXIS2_PLACEMENT_3D('',#70910,#36990,#36991);
#30580=AXIS2_PLACEMENT_3D('',#70911,#36992,#36993);
#30581=AXIS2_PLACEMENT_3D('',#70914,#36995,#36996);
#30582=AXIS2_PLACEMENT_3D('',#70915,#36997,#36998);
#30583=AXIS2_PLACEMENT_3D('',#70918,#37000,#37001);
#30584=AXIS2_PLACEMENT_3D('',#70919,#37002,#37003);
#30585=AXIS2_PLACEMENT_3D('',#70922,#37005,#37006);
#30586=AXIS2_PLACEMENT_3D('',#70923,#37007,#37008);
#30587=AXIS2_PLACEMENT_3D('',#70926,#37010,#37011);
#30588=AXIS2_PLACEMENT_3D('',#70927,#37012,#37013);
#30589=AXIS2_PLACEMENT_3D('',#70930,#37015,#37016);
#30590=AXIS2_PLACEMENT_3D('',#70931,#37017,#37018);
#30591=AXIS2_PLACEMENT_3D('',#70934,#37020,#37021);
#30592=AXIS2_PLACEMENT_3D('',#70935,#37022,#37023);
#30593=AXIS2_PLACEMENT_3D('',#70938,#37025,#37026);
#30594=AXIS2_PLACEMENT_3D('',#70939,#37027,#37028);
#30595=AXIS2_PLACEMENT_3D('',#70941,#37029,#37030);
#30596=AXIS2_PLACEMENT_3D('',#70944,#37032,#37033);
#30597=AXIS2_PLACEMENT_3D('',#70945,#37034,#37035);
#30598=AXIS2_PLACEMENT_3D('',#70955,#37040,#37041);
#30599=AXIS2_PLACEMENT_3D('',#70957,#37042,#37043);
#30600=AXIS2_PLACEMENT_3D('',#70959,#37044,#37045);
#30601=AXIS2_PLACEMENT_3D('',#70961,#37046,#37047);
#30602=AXIS2_PLACEMENT_3D('',#70963,#37048,#37049);
#30603=AXIS2_PLACEMENT_3D('',#70965,#37050,#37051);
#30604=AXIS2_PLACEMENT_3D('',#70967,#37052,#37053);
#30605=AXIS2_PLACEMENT_3D('',#70969,#37054,#37055);
#30606=AXIS2_PLACEMENT_3D('',#70971,#37056,#37057);
#30607=AXIS2_PLACEMENT_3D('',#70973,#37058,#37059);
#30608=AXIS2_PLACEMENT_3D('',#70974,#37060,#37061);
#30609=AXIS2_PLACEMENT_3D('',#70976,#37062,#37063);
#30610=AXIS2_PLACEMENT_3D('',#70978,#37065,#37066);
#30611=AXIS2_PLACEMENT_3D('',#70981,#37068,#37069);
#30612=AXIS2_PLACEMENT_3D('',#70982,#37070,#37071);
#30613=AXIS2_PLACEMENT_3D('',#70984,#37072,#37073);
#30614=AXIS2_PLACEMENT_3D('',#70986,#37075,#37076);
#30615=AXIS2_PLACEMENT_3D('',#70989,#37078,#37079);
#30616=AXIS2_PLACEMENT_3D('',#70990,#37080,#37081);
#30617=AXIS2_PLACEMENT_3D('',#70992,#37082,#37083);
#30618=AXIS2_PLACEMENT_3D('',#70994,#37085,#37086);
#30619=AXIS2_PLACEMENT_3D('',#70997,#37088,#37089);
#30620=AXIS2_PLACEMENT_3D('',#70998,#37090,#37091);
#30621=AXIS2_PLACEMENT_3D('',#71000,#37092,#37093);
#30622=AXIS2_PLACEMENT_3D('',#71002,#37095,#37096);
#30623=AXIS2_PLACEMENT_3D('',#71005,#37098,#37099);
#30624=AXIS2_PLACEMENT_3D('',#71006,#37100,#37101);
#30625=AXIS2_PLACEMENT_3D('',#71008,#37102,#37103);
#30626=AXIS2_PLACEMENT_3D('',#71010,#37105,#37106);
#30627=AXIS2_PLACEMENT_3D('',#71016,#37110,#37111);
#30628=AXIS2_PLACEMENT_3D('',#71020,#37113,#37114);
#30629=AXIS2_PLACEMENT_3D('',#71021,#37115,#37116);
#30630=AXIS2_PLACEMENT_3D('',#71022,#37117,#37118);
#30631=AXIS2_PLACEMENT_3D('',#71028,#37122,#37123);
#30632=AXIS2_PLACEMENT_3D('',#71031,#37125,#37126);
#30633=AXIS2_PLACEMENT_3D('',#71032,#37127,#37128);
#30634=AXIS2_PLACEMENT_3D('',#71033,#37129,#37130);
#30635=AXIS2_PLACEMENT_3D('',#71037,#37133,#37134);
#30636=AXIS2_PLACEMENT_3D('',#71041,#37136,#37137);
#30637=AXIS2_PLACEMENT_3D('',#71042,#37138,#37139);
#30638=AXIS2_PLACEMENT_3D('',#71043,#37140,#37141);
#30639=AXIS2_PLACEMENT_3D('',#71049,#37145,#37146);
#30640=AXIS2_PLACEMENT_3D('',#71050,#37147,#37148);
#30641=AXIS2_PLACEMENT_3D('',#71051,#37149,#37150);
#30642=AXIS2_PLACEMENT_3D('',#71052,#37151,#37152);
#30643=AXIS2_PLACEMENT_3D('',#71055,#37154,#37155);
#30644=AXIS2_PLACEMENT_3D('',#71056,#37156,#37157);
#30645=AXIS2_PLACEMENT_3D('',#71060,#37160,#37161);
#30646=AXIS2_PLACEMENT_3D('',#71061,#37162,#37163);
#30647=AXIS2_PLACEMENT_3D('',#71062,#37164,#37165);
#30648=AXIS2_PLACEMENT_3D('',#71067,#37167,#37168);
#30649=AXIS2_PLACEMENT_3D('',#71071,#37170,#37171);
#30650=AXIS2_PLACEMENT_3D('',#71075,#37173,#37174);
#30651=AXIS2_PLACEMENT_3D('',#71078,#37176,#37177);
#30652=AXIS2_PLACEMENT_3D('',#71079,#37178,#37179);
#30653=AXIS2_PLACEMENT_3D('',#71082,#37181,#37182);
#30654=AXIS2_PLACEMENT_3D('',#71083,#37183,#37184);
#30655=AXIS2_PLACEMENT_3D('',#71085,#37185,#37186);
#30656=AXIS2_PLACEMENT_3D('',#71087,#37188,#37189);
#30657=AXIS2_PLACEMENT_3D('',#71090,#37191,#37192);
#30658=AXIS2_PLACEMENT_3D('',#71091,#37193,#37194);
#30659=AXIS2_PLACEMENT_3D('',#71093,#37195,#37196);
#30660=AXIS2_PLACEMENT_3D('',#71095,#37198,#37199);
#30661=AXIS2_PLACEMENT_3D('',#71098,#37201,#37202);
#30662=AXIS2_PLACEMENT_3D('',#71099,#37203,#37204);
#30663=AXIS2_PLACEMENT_3D('',#71101,#37205,#37206);
#30664=AXIS2_PLACEMENT_3D('',#71103,#37208,#37209);
#30665=AXIS2_PLACEMENT_3D('',#71106,#37211,#37212);
#30666=AXIS2_PLACEMENT_3D('',#71107,#37213,#37214);
#30667=AXIS2_PLACEMENT_3D('',#71110,#37216,#37217);
#30668=AXIS2_PLACEMENT_3D('',#71111,#37218,#37219);
#30669=AXIS2_PLACEMENT_3D('',#71114,#37221,#37222);
#30670=AXIS2_PLACEMENT_3D('',#71115,#37223,#37224);
#30671=AXIS2_PLACEMENT_3D('',#71117,#37225,#37226);
#30672=AXIS2_PLACEMENT_3D('',#71119,#37228,#37229);
#30673=AXIS2_PLACEMENT_3D('',#71122,#37231,#37232);
#30674=AXIS2_PLACEMENT_3D('',#71123,#37233,#37234);
#30675=AXIS2_PLACEMENT_3D('',#71126,#37236,#37237);
#30676=AXIS2_PLACEMENT_3D('',#71127,#37238,#37239);
#30677=AXIS2_PLACEMENT_3D('',#71130,#37241,#37242);
#30678=AXIS2_PLACEMENT_3D('',#71131,#37243,#37244);
#30679=AXIS2_PLACEMENT_3D('',#71133,#37245,#37246);
#30680=AXIS2_PLACEMENT_3D('',#71135,#37248,#37249);
#30681=AXIS2_PLACEMENT_3D('',#71138,#37251,#37252);
#30682=AXIS2_PLACEMENT_3D('',#71139,#37253,#37254);
#30683=AXIS2_PLACEMENT_3D('',#71142,#37256,#37257);
#30684=AXIS2_PLACEMENT_3D('',#71143,#37258,#37259);
#30685=AXIS2_PLACEMENT_3D('',#71146,#37261,#37262);
#30686=AXIS2_PLACEMENT_3D('',#71147,#37263,#37264);
#30687=AXIS2_PLACEMENT_3D('',#71149,#37265,#37266);
#30688=AXIS2_PLACEMENT_3D('',#71151,#37268,#37269);
#30689=AXIS2_PLACEMENT_3D('',#71153,#37270,#37271);
#30690=AXIS2_PLACEMENT_3D('',#71155,#37273,#37274);
#30691=AXIS2_PLACEMENT_3D('',#71165,#37279,#37280);
#30692=AXIS2_PLACEMENT_3D('',#71167,#37281,#37282);
#30693=AXIS2_PLACEMENT_3D('',#71169,#37283,#37284);
#30694=AXIS2_PLACEMENT_3D('',#71171,#37285,#37286);
#30695=AXIS2_PLACEMENT_3D('',#71173,#37287,#37288);
#30696=AXIS2_PLACEMENT_3D('',#71175,#37289,#37290);
#30697=AXIS2_PLACEMENT_3D('',#71177,#37291,#37292);
#30698=AXIS2_PLACEMENT_3D('',#71179,#37293,#37294);
#30699=AXIS2_PLACEMENT_3D('',#71181,#37295,#37296);
#30700=AXIS2_PLACEMENT_3D('',#71183,#37297,#37298);
#30701=AXIS2_PLACEMENT_3D('',#71184,#37299,#37300);
#30702=AXIS2_PLACEMENT_3D('',#71186,#37302,#37303);
#30703=AXIS2_PLACEMENT_3D('',#71188,#37305,#37306);
#30704=AXIS2_PLACEMENT_3D('',#71190,#37308,#37309);
#30705=AXIS2_PLACEMENT_3D('',#71192,#37311,#37312);
#30706=AXIS2_PLACEMENT_3D('',#71195,#37314,#37315);
#30707=AXIS2_PLACEMENT_3D('',#71196,#37316,#37317);
#30708=AXIS2_PLACEMENT_3D('',#71199,#37319,#37320);
#30709=AXIS2_PLACEMENT_3D('',#71200,#37321,#37322);
#30710=AXIS2_PLACEMENT_3D('',#71202,#37323,#37324);
#30711=AXIS2_PLACEMENT_3D('',#71204,#37326,#37327);
#30712=AXIS2_PLACEMENT_3D('',#71214,#37332,#37333);
#30713=AXIS2_PLACEMENT_3D('',#71216,#37334,#37335);
#30714=AXIS2_PLACEMENT_3D('',#71218,#37336,#37337);
#30715=AXIS2_PLACEMENT_3D('',#71220,#37338,#37339);
#30716=AXIS2_PLACEMENT_3D('',#71222,#37340,#37341);
#30717=AXIS2_PLACEMENT_3D('',#71224,#37342,#37343);
#30718=AXIS2_PLACEMENT_3D('',#71226,#37344,#37345);
#30719=AXIS2_PLACEMENT_3D('',#71228,#37346,#37347);
#30720=AXIS2_PLACEMENT_3D('',#71230,#37348,#37349);
#30721=AXIS2_PLACEMENT_3D('',#71232,#37350,#37351);
#30722=AXIS2_PLACEMENT_3D('',#71233,#37352,#37353);
#30723=AXIS2_PLACEMENT_3D('',#71235,#37355,#37356);
#30724=AXIS2_PLACEMENT_3D('',#71237,#37358,#37359);
#30725=AXIS2_PLACEMENT_3D('',#71239,#37361,#37362);
#30726=AXIS2_PLACEMENT_3D('',#71241,#37364,#37365);
#30727=AXIS2_PLACEMENT_3D('',#71244,#37368,#37369);
#30728=AXIS2_PLACEMENT_3D('',#71247,#37371,#37372);
#30729=AXIS2_PLACEMENT_3D('',#71248,#37373,#37374);
#30730=AXIS2_PLACEMENT_3D('',#71252,#37377,#37378);
#30731=AXIS2_PLACEMENT_3D('',#71254,#37380,#37381);
#30732=AXIS2_PLACEMENT_3D('',#71255,#37382,#37383);
#30733=AXIS2_PLACEMENT_3D('',#71257,#37385,#37386);
#30734=AXIS2_PLACEMENT_3D('',#71260,#37388,#37389);
#30735=AXIS2_PLACEMENT_3D('',#71261,#37390,#37391);
#30736=AXIS2_PLACEMENT_3D('',#71265,#37394,#37395);
#30737=AXIS2_PLACEMENT_3D('',#71266,#37396,#37397);
#30738=AXIS2_PLACEMENT_3D('',#71267,#37398,#37399);
#30739=AXIS2_PLACEMENT_3D('',#71270,#37401,#37402);
#30740=AXIS2_PLACEMENT_3D('',#71271,#37403,#37404);
#30741=AXIS2_PLACEMENT_3D('',#71275,#37407,#37408);
#30742=AXIS2_PLACEMENT_3D('',#71276,#37409,#37410);
#30743=AXIS2_PLACEMENT_3D('',#71277,#37411,#37412);
#30744=AXIS2_PLACEMENT_3D('',#71279,#37414,#37415);
#30745=AXIS2_PLACEMENT_3D('',#71281,#37417,#37418);
#30746=AXIS2_PLACEMENT_3D('',#71283,#37420,#37421);
#30747=AXIS2_PLACEMENT_3D('',#71285,#37423,#37424);
#30748=AXIS2_PLACEMENT_3D('',#71287,#37426,#37427);
#30749=AXIS2_PLACEMENT_3D('',#71289,#37429,#37430);
#30750=AXIS2_PLACEMENT_3D('',#71291,#37432,#37433);
#30751=AXIS2_PLACEMENT_3D('',#71293,#37435,#37436);
#30752=AXIS2_PLACEMENT_3D('',#71295,#37438,#37439);
#30753=AXIS2_PLACEMENT_3D('',#71297,#37441,#37442);
#30754=AXIS2_PLACEMENT_3D('',#71299,#37444,#37445);
#30755=AXIS2_PLACEMENT_3D('',#71301,#37447,#37448);
#30756=AXIS2_PLACEMENT_3D('',#71305,#37450,#37451);
#30757=AXIS2_PLACEMENT_3D('',#71308,#37453,#37454);
#30758=AXIS2_PLACEMENT_3D('',#71309,#37455,#37456);
#30759=AXIS2_PLACEMENT_3D('',#71315,#37460,#37461);
#30760=AXIS2_PLACEMENT_3D('',#71318,#37463,#37464);
#30761=AXIS2_PLACEMENT_3D('',#71319,#37465,#37466);
#30762=AXIS2_PLACEMENT_3D('',#71320,#37467,#37468);
#30763=AXIS2_PLACEMENT_3D('',#71324,#37471,#37472);
#30764=AXIS2_PLACEMENT_3D('',#71327,#37474,#37475);
#30765=AXIS2_PLACEMENT_3D('',#71328,#37476,#37477);
#30766=AXIS2_PLACEMENT_3D('',#71332,#37480,#37481);
#30767=AXIS2_PLACEMENT_3D('',#71335,#37483,#37484);
#30768=AXIS2_PLACEMENT_3D('',#71336,#37485,#37486);
#30769=AXIS2_PLACEMENT_3D('',#71338,#37488,#37489);
#30770=AXIS2_PLACEMENT_3D('',#71340,#37491,#37492);
#30771=AXIS2_PLACEMENT_3D('',#71343,#37493,#37494);
#30772=AXIS2_PLACEMENT_3D('',#71347,#37496,#37497);
#30773=AXIS2_PLACEMENT_3D('',#71351,#37499,#37500);
#30774=AXIS2_PLACEMENT_3D('',#71355,#37502,#37503);
#30775=AXIS2_PLACEMENT_3D('',#71357,#37505,#37506);
#30776=AXIS2_PLACEMENT_3D('',#71360,#37508,#37509);
#30777=AXIS2_PLACEMENT_3D('',#71362,#37511,#37512);
#30778=AXIS2_PLACEMENT_3D('',#71366,#37515,#37516);
#30779=AXIS2_PLACEMENT_3D('',#71368,#37518,#37519);
#30780=AXIS2_PLACEMENT_3D('',#71369,#37520,#37521);
#30781=AXIS2_PLACEMENT_3D('',#71371,#37523,#37524);
#30782=AXIS2_PLACEMENT_3D('',#71373,#37526,#37527);
#30783=AXIS2_PLACEMENT_3D('',#71375,#37529,#37530);
#30784=AXIS2_PLACEMENT_3D('',#71377,#37532,#37533);
#30785=AXIS2_PLACEMENT_3D('',#71378,#37534,#37535);
#30786=AXIS2_PLACEMENT_3D('',#71380,#37537,#37538);
#30787=AXIS2_PLACEMENT_3D('',#71382,#37540,#37541);
#30788=AXIS2_PLACEMENT_3D('',#71383,#37542,#37543);
#30789=AXIS2_PLACEMENT_3D('',#71385,#37545,#37546);
#30790=AXIS2_PLACEMENT_3D('',#71386,#37547,#37548);
#30791=AXIS2_PLACEMENT_3D('',#71387,#37549,#37550);
#30792=AXIS2_PLACEMENT_3D('',#71388,#37551,#37552);
#30793=AXIS2_PLACEMENT_3D('',#71389,#37553,#37554);
#30794=AXIS2_PLACEMENT_3D('',#71390,#37555,#37556);
#30795=AXIS2_PLACEMENT_3D('',#71391,#37557,#37558);
#30796=AXIS2_PLACEMENT_3D('',#71392,#37559,#37560);
#30797=AXIS2_PLACEMENT_3D('',#71393,#37561,#37562);
#30798=AXIS2_PLACEMENT_3D('',#71394,#37563,#37564);
#30799=AXIS2_PLACEMENT_3D('',#71395,#37565,#37566);
#30800=AXIS2_PLACEMENT_3D('',#71396,#37567,#37568);
#30801=AXIS2_PLACEMENT_3D('',#71397,#37569,#37570);
#30802=AXIS2_PLACEMENT_3D('',#71398,#37571,#37572);
#30803=AXIS2_PLACEMENT_3D('',#71399,#37573,#37574);
#30804=AXIS2_PLACEMENT_3D('',#71400,#37575,#37576);
#30805=AXIS2_PLACEMENT_3D('',#71401,#37577,#37578);
#30806=AXIS2_PLACEMENT_3D('',#71402,#37579,#37580);
#30807=AXIS2_PLACEMENT_3D('',#71403,#37581,#37582);
#30808=AXIS2_PLACEMENT_3D('',#71404,#37583,#37584);
#30809=AXIS2_PLACEMENT_3D('',#71405,#37585,#37586);
#30810=AXIS2_PLACEMENT_3D('',#71406,#37587,#37588);
#30811=AXIS2_PLACEMENT_3D('',#71407,#37589,#37590);
#30812=AXIS2_PLACEMENT_3D('',#71408,#37591,#37592);
#30813=AXIS2_PLACEMENT_3D('',#71409,#37593,#37594);
#30814=AXIS2_PLACEMENT_3D('',#71410,#37595,#37596);
#30815=AXIS2_PLACEMENT_3D('',#71411,#37597,#37598);
#30816=AXIS2_PLACEMENT_3D('',#71412,#37599,#37600);
#30817=AXIS2_PLACEMENT_3D('',#71413,#37601,#37602);
#30818=AXIS2_PLACEMENT_3D('',#71414,#37603,#37604);
#30819=AXIS2_PLACEMENT_3D('',#71415,#37605,#37606);
#30820=AXIS2_PLACEMENT_3D('',#71416,#37607,#37608);
#30821=AXIS2_PLACEMENT_3D('',#71417,#37609,#37610);
#30822=AXIS2_PLACEMENT_3D('',#71418,#37611,#37612);
#30823=AXIS2_PLACEMENT_3D('',#71419,#37613,#37614);
#30824=AXIS2_PLACEMENT_3D('',#71420,#37615,#37616);
#30825=AXIS2_PLACEMENT_3D('',#71421,#37617,#37618);
#30826=AXIS2_PLACEMENT_3D('',#71422,#37619,#37620);
#30827=AXIS2_PLACEMENT_3D('',#71423,#37621,#37622);
#30828=AXIS2_PLACEMENT_3D('',#71424,#37623,#37624);
#30829=AXIS2_PLACEMENT_3D('',#71425,#37625,#37626);
#30830=AXIS2_PLACEMENT_3D('',#71426,#37627,#37628);
#30831=AXIS2_PLACEMENT_3D('',#71427,#37629,#37630);
#30832=AXIS2_PLACEMENT_3D('',#71428,#37631,#37632);
#30833=AXIS2_PLACEMENT_3D('',#71429,#37633,#37634);
#30834=AXIS2_PLACEMENT_3D('',#71430,#37635,#37636);
#30835=AXIS2_PLACEMENT_3D('',#71431,#37637,#37638);
#30836=AXIS2_PLACEMENT_3D('',#71432,#37639,#37640);
#30837=AXIS2_PLACEMENT_3D('',#71433,#37641,#37642);
#30838=AXIS2_PLACEMENT_3D('',#71434,#37643,#37644);
#30839=AXIS2_PLACEMENT_3D('',#71435,#37645,#37646);
#30840=AXIS2_PLACEMENT_3D('',#71436,#37647,#37648);
#30841=AXIS2_PLACEMENT_3D('',#71437,#37649,#37650);
#30842=AXIS2_PLACEMENT_3D('',#71438,#37651,#37652);
#30843=AXIS2_PLACEMENT_3D('',#71439,#37653,#37654);
#30844=AXIS2_PLACEMENT_3D('',#71440,#37655,#37656);
#30845=AXIS2_PLACEMENT_3D('',#71441,#37657,#37658);
#30846=AXIS2_PLACEMENT_3D('',#71442,#37659,#37660);
#30847=AXIS2_PLACEMENT_3D('',#71443,#37661,#37662);
#30848=AXIS2_PLACEMENT_3D('',#71444,#37663,#37664);
#30849=AXIS2_PLACEMENT_3D('',#71445,#37665,#37666);
#30850=AXIS2_PLACEMENT_3D('',#71446,#37667,#37668);
#30851=AXIS2_PLACEMENT_3D('',#71447,#37669,#37670);
#30852=AXIS2_PLACEMENT_3D('',#71448,#37671,#37672);
#30853=AXIS2_PLACEMENT_3D('',#71449,#37673,#37674);
#30854=AXIS2_PLACEMENT_3D('',#71450,#37675,#37676);
#30855=DIRECTION('axis',(0.,0.,1.));
#30856=DIRECTION('refdir',(1.,0.,0.));
#30857=DIRECTION('axis',(0.,0.,1.));
#30858=DIRECTION('refdir',(1.,0.,0.));
#30859=DIRECTION('center_axis',(-0.707106781186548,0.707106781186548,0.));
#30860=DIRECTION('ref_axis',(0.,0.,1.));
#30861=DIRECTION('',(0.577350269189581,0.577350269189581,-0.577350269189715));
#30862=DIRECTION('',(0.,0.,-1.));
#30863=DIRECTION('',(-0.577350269189619,-0.577350269189619,-0.57735026918964));
#30864=DIRECTION('',(-0.577350269189617,-0.577350269189617,0.577350269189644));
#30865=DIRECTION('',(0.,0.,1.));
#30866=DIRECTION('center_axis',(0.,0.70710678118656,-0.707106781186535));
#30867=DIRECTION('ref_axis',(-1.,0.,0.));
#30868=DIRECTION('',(1.,0.,0.));
#30869=DIRECTION('',(-0.577350269189619,0.577350269189619,0.57735026918964));
#30870=DIRECTION('',(0.577350269189614,0.577350269189621,0.577350269189642));
#30871=DIRECTION('',(-1.,0.,0.));
#30872=DIRECTION('',(0.577350269189605,-0.577350269189626,-0.577350269189646));
#30873=DIRECTION('center_axis',(0.,1.,0.));
#30874=DIRECTION('ref_axis',(-1.,0.,0.));
#30875=DIRECTION('',(-1.,0.,0.));
#30876=DIRECTION('',(0.,0.,1.));
#30877=DIRECTION('center_axis',(0.,0.707106781186629,0.707106781186466));
#30878=DIRECTION('ref_axis',(1.,0.,0.));
#30879=DIRECTION('',(1.,0.,0.));
#30880=DIRECTION('',(-0.577350269189581,0.577350269189581,-0.577350269189715));
#30881=DIRECTION('center_axis',(0.707106781186548,0.707106781186548,0.));
#30882=DIRECTION('ref_axis',(0.,0.,-1.));
#30883=DIRECTION('',(0.,0.,-1.));
#30884=DIRECTION('',(-0.577350269189617,0.577350269189617,-0.577350269189644));
#30885=DIRECTION('center_axis',(0.707106781186564,0.,-0.707106781186531));
#30886=DIRECTION('ref_axis',(-0.707106781186531,0.,-0.707106781186564));
#30887=DIRECTION('',(0.,-1.,0.));
#30888=DIRECTION('',(0.577350269189617,0.577350269189617,0.577350269189644));
#30889=DIRECTION('',(0.577350269189614,-0.577350269189621,0.577350269189642));
#30890=DIRECTION('',(0.,1.,0.));
#30891=DIRECTION('center_axis',(1.,0.,0.));
#30892=DIRECTION('ref_axis',(0.,1.,0.));
#30893=DIRECTION('',(0.,1.,0.));
#30894=DIRECTION('',(0.,1.,0.));
#30895=DIRECTION('',(0.,1.,0.));
#30896=DIRECTION('',(0.,1.,0.));
#30897=DIRECTION('',(0.,1.,0.));
#30898=DIRECTION('',(0.,0.,1.));
#30899=DIRECTION('center_axis',(-0.707106781186548,-0.707106781186548,0.));
#30900=DIRECTION('ref_axis',(0.,0.,1.));
#30901=DIRECTION('',(-0.577350269189581,0.577350269189581,0.577350269189715));
#30902=DIRECTION('',(0.,0.,-1.));
#30903=DIRECTION('',(0.577350269189617,-0.577350269189617,-0.577350269189644));
#30904=DIRECTION('',(0.577350269189619,-0.577350269189619,0.57735026918964));
#30905=DIRECTION('',(0.,0.,1.));
#30906=DIRECTION('center_axis',(0.,-1.,0.));
#30907=DIRECTION('ref_axis',(1.,0.,0.));
#30908=DIRECTION('',(-1.,0.,0.));
#30909=DIRECTION('',(0.,0.,-1.));
#30910=DIRECTION('',(1.,0.,0.));
#30911=DIRECTION('center_axis',(0.,-0.70710678118656,-0.707106781186535));
#30912=DIRECTION('ref_axis',(-1.,0.,0.));
#30913=DIRECTION('',(-0.577350269189614,-0.577350269189621,0.577350269189642));
#30914=DIRECTION('',(1.,0.,0.));
#30915=DIRECTION('',(0.577350269189619,0.577350269189619,-0.57735026918964));
#30916=DIRECTION('center_axis',(-0.707106781186564,0.,-0.707106781186531));
#30917=DIRECTION('ref_axis',(-0.707106781186531,0.,0.707106781186564));
#30918=DIRECTION('',(0.,-1.,0.));
#30919=DIRECTION('',(0.,1.,0.));
#30920=DIRECTION('center_axis',(0.,-0.707106781186629,0.707106781186466));
#30921=DIRECTION('ref_axis',(1.,0.,0.));
#30922=DIRECTION('',(0.577350269189581,0.577350269189581,0.577350269189715));
#30923=DIRECTION('',(-1.,0.,0.));
#30924=DIRECTION('center_axis',(0.,0.,1.));
#30925=DIRECTION('ref_axis',(1.,0.,0.));
#30926=DIRECTION('',(1.,0.,0.));
#30927=DIRECTION('',(0.,-1.,0.));
#30928=DIRECTION('center_axis',(0.707106781186548,-0.707106781186548,0.));
#30929=DIRECTION('ref_axis',(0.,0.,-1.));
#30930=DIRECTION('center_axis',(0.,-1.,0.));
#30931=DIRECTION('ref_axis',(1.,0.,0.));
#30932=DIRECTION('center_axis',(0.,-1.,0.));
#30933=DIRECTION('ref_axis',(1.,0.,0.));
#30934=DIRECTION('',(0.707106781186554,0.707106781186541,8.65956056235501E-17));
#30935=DIRECTION('center_axis',(0.,1.,0.));
#30936=DIRECTION('ref_axis',(1.,0.,0.));
#30937=DIRECTION('center_axis',(0.,-1.,0.));
#30938=DIRECTION('ref_axis',(0.,0.,-1.));
#30939=DIRECTION('',(0.,0.,1.));
#30940=DIRECTION('',(-1.,0.,0.));
#30941=DIRECTION('',(0.,0.,-1.));
#30942=DIRECTION('',(1.,0.,0.));
#30943=DIRECTION('center_axis',(0.,-1.,0.));
#30944=DIRECTION('ref_axis',(1.,0.,0.));
#30945=DIRECTION('center_axis',(0.,-1.,0.));
#30946=DIRECTION('ref_axis',(1.,0.,0.));
#30947=DIRECTION('center_axis',(0.,-1.,0.));
#30948=DIRECTION('ref_axis',(1.,0.,0.));
#30949=DIRECTION('center_axis',(0.,1.,0.));
#30950=DIRECTION('ref_axis',(1.,0.,0.));
#30951=DIRECTION('',(0.,1.,0.));
#30952=DIRECTION('center_axis',(0.,-1.,0.));
#30953=DIRECTION('ref_axis',(1.,0.,0.));
#30954=DIRECTION('center_axis',(0.,-1.,0.));
#30955=DIRECTION('ref_axis',(1.,0.,0.));
#30956=DIRECTION('',(0.707106781186554,0.707106781186541,8.65956056235501E-17));
#30957=DIRECTION('center_axis',(0.,1.,0.));
#30958=DIRECTION('ref_axis',(1.,0.,0.));
#30959=DIRECTION('center_axis',(0.,1.,0.));
#30960=DIRECTION('ref_axis',(1.,0.,0.));
#30961=DIRECTION('',(0.,1.,0.));
#30962=DIRECTION('center_axis',(0.,-1.,0.));
#30963=DIRECTION('ref_axis',(1.,0.,0.));
#30964=DIRECTION('center_axis',(0.,-1.,0.));
#30965=DIRECTION('ref_axis',(1.,0.,0.));
#30966=DIRECTION('',(0.707106781186554,0.707106781186541,8.65956056235501E-17));
#30967=DIRECTION('center_axis',(0.,1.,0.));
#30968=DIRECTION('ref_axis',(1.,0.,0.));
#30969=DIRECTION('center_axis',(0.,1.,0.));
#30970=DIRECTION('ref_axis',(1.,0.,0.));
#30971=DIRECTION('',(0.,1.,0.));
#30972=DIRECTION('center_axis',(0.,-1.,0.));
#30973=DIRECTION('ref_axis',(1.,0.,0.));
#30974=DIRECTION('center_axis',(0.,-1.,0.));
#30975=DIRECTION('ref_axis',(1.,0.,0.));
#30976=DIRECTION('',(0.707106781186554,0.707106781186541,8.65956056235501E-17));
#30977=DIRECTION('center_axis',(0.,1.,0.));
#30978=DIRECTION('ref_axis',(1.,0.,0.));
#30979=DIRECTION('center_axis',(0.,1.,0.));
#30980=DIRECTION('ref_axis',(1.,0.,0.));
#30981=DIRECTION('',(0.,1.,0.));
#30982=DIRECTION('center_axis',(0.,-1.,0.));
#30983=DIRECTION('ref_axis',(1.,0.,0.));
#30984=DIRECTION('center_axis',(0.,1.,0.));
#30985=DIRECTION('ref_axis',(1.,0.,0.));
#30986=DIRECTION('center_axis',(0.,1.,0.));
#30987=DIRECTION('ref_axis',(1.,0.,0.));
#30988=DIRECTION('',(0.707106781186554,-0.707106781186541,-8.65956056235501E-17));
#30989=DIRECTION('center_axis',(0.,1.,0.));
#30990=DIRECTION('ref_axis',(0.,0.,1.));
#30991=DIRECTION('',(0.,0.,1.));
#30992=DIRECTION('',(1.,0.,0.));
#30993=DIRECTION('',(0.,0.,-1.));
#30994=DIRECTION('',(-1.,0.,0.));
#30995=DIRECTION('center_axis',(0.,1.,0.));
#30996=DIRECTION('ref_axis',(1.,0.,0.));
#30997=DIRECTION('center_axis',(0.,1.,0.));
#30998=DIRECTION('ref_axis',(1.,0.,0.));
#30999=DIRECTION('center_axis',(0.,1.,0.));
#31000=DIRECTION('ref_axis',(1.,0.,0.));
#31001=DIRECTION('center_axis',(0.,1.,0.));
#31002=DIRECTION('ref_axis',(1.,0.,0.));
#31003=DIRECTION('',(0.707106781186554,-0.707106781186541,-8.65956056235501E-17));
#31004=DIRECTION('center_axis',(0.,1.,0.));
#31005=DIRECTION('ref_axis',(1.,0.,0.));
#31006=DIRECTION('',(0.707106781186554,-0.707106781186541,-8.65956056235501E-17));
#31007=DIRECTION('center_axis',(0.,1.,0.));
#31008=DIRECTION('ref_axis',(1.,0.,0.));
#31009=DIRECTION('',(0.707106781186554,-0.707106781186541,-8.65956056235501E-17));
#31010=DIRECTION('center_axis',(0.,1.,0.));
#31011=DIRECTION('ref_axis',(1.,0.,0.));
#31012=DIRECTION('center_axis',(0.,1.,0.));
#31013=DIRECTION('ref_axis',(1.,0.,0.));
#31014=DIRECTION('',(0.707106781186554,-0.707106781186541,-8.65956056235501E-17));
#31015=DIRECTION('center_axis',(0.,-1.,0.));
#31016=DIRECTION('ref_axis',(1.,0.,0.));
#31017=DIRECTION('center_axis',(0.,1.,0.));
#31018=DIRECTION('ref_axis',(0.,0.,1.));
#31019=DIRECTION('',(0.,0.,1.));
#31020=DIRECTION('',(1.,0.,0.));
#31021=DIRECTION('',(0.,0.,-1.));
#31022=DIRECTION('',(-1.,0.,0.));
#31023=DIRECTION('center_axis',(0.,1.,0.));
#31024=DIRECTION('ref_axis',(1.,0.,0.));
#31025=DIRECTION('center_axis',(0.,1.,0.));
#31026=DIRECTION('ref_axis',(1.,0.,0.));
#31027=DIRECTION('center_axis',(0.,1.,0.));
#31028=DIRECTION('ref_axis',(1.,0.,0.));
#31029=DIRECTION('center_axis',(0.,1.,0.));
#31030=DIRECTION('ref_axis',(1.,0.,0.));
#31031=DIRECTION('center_axis',(0.,1.,0.));
#31032=DIRECTION('ref_axis',(1.,0.,0.));
#31033=DIRECTION('',(0.,1.,0.));
#31034=DIRECTION('center_axis',(0.,1.,0.));
#31035=DIRECTION('ref_axis',(1.,0.,0.));
#31036=DIRECTION('',(0.707106781186554,-0.707106781186541,-8.65956056235501E-17));
#31037=DIRECTION('center_axis',(0.,-1.,0.));
#31038=DIRECTION('ref_axis',(1.,0.,0.));
#31039=DIRECTION('center_axis',(0.,1.,0.));
#31040=DIRECTION('ref_axis',(1.,0.,0.));
#31041=DIRECTION('center_axis',(0.,1.,0.));
#31042=DIRECTION('ref_axis',(1.,0.,0.));
#31043=DIRECTION('',(0.,1.,0.));
#31044=DIRECTION('center_axis',(0.,1.,0.));
#31045=DIRECTION('ref_axis',(1.,0.,0.));
#31046=DIRECTION('',(0.707106781186554,-0.707106781186541,-8.65956056235501E-17));
#31047=DIRECTION('center_axis',(0.,-1.,0.));
#31048=DIRECTION('ref_axis',(1.,0.,0.));
#31049=DIRECTION('center_axis',(0.,1.,0.));
#31050=DIRECTION('ref_axis',(1.,0.,0.));
#31051=DIRECTION('center_axis',(0.,1.,0.));
#31052=DIRECTION('ref_axis',(1.,0.,0.));
#31053=DIRECTION('',(0.,1.,0.));
#31054=DIRECTION('center_axis',(0.,1.,0.));
#31055=DIRECTION('ref_axis',(1.,0.,0.));
#31056=DIRECTION('',(0.707106781186554,-0.707106781186541,-8.65956056235501E-17));
#31057=DIRECTION('center_axis',(0.,-1.,0.));
#31058=DIRECTION('ref_axis',(1.,0.,0.));
#31059=DIRECTION('center_axis',(0.,1.,0.));
#31060=DIRECTION('ref_axis',(1.,0.,0.));
#31061=DIRECTION('center_axis',(0.,1.,0.));
#31062=DIRECTION('ref_axis',(1.,0.,0.));
#31063=DIRECTION('',(0.,1.,0.));
#31064=DIRECTION('center_axis',(0.,-1.,0.));
#31065=DIRECTION('ref_axis',(6.12323399573677E-17,0.,-1.));
#31066=DIRECTION('',(-0.315789473684196,0.707106781186531,-0.632674488430095));
#31067=DIRECTION('center_axis',(0.,1.,0.));
#31068=DIRECTION('ref_axis',(1.,0.,0.));
#31069=DIRECTION('center_axis',(0.,1.,0.));
#31070=DIRECTION('ref_axis',(1.,0.,0.));
#31071=DIRECTION('',(-0.315789473684196,-0.707106781186531,0.632674488430095));
#31072=DIRECTION('center_axis',(0.,-1.,0.));
#31073=DIRECTION('ref_axis',(1.,0.,0.));
#31074=DIRECTION('',(0.238798209365739,-0.687106448937468,0.686192497067885));
#31075=DIRECTION('',(0.238798209365798,0.687106448937561,-0.686192497067771));
#31076=DIRECTION('center_axis',(1.,0.,0.));
#31077=DIRECTION('ref_axis',(0.,-0.707106781186543,0.707106781186552));
#31078=DIRECTION('',(1.,0.,0.));
#31079=DIRECTION('center_axis',(1.,0.,0.));
#31080=DIRECTION('ref_axis',(0.,-0.707106781186543,0.707106781186552));
#31081=DIRECTION('',(-1.,0.,0.));
#31082=DIRECTION('center_axis',(-1.,0.,0.));
#31083=DIRECTION('ref_axis',(0.,-0.707106781186543,0.707106781186552));
#31084=DIRECTION('',(1.,0.,0.));
#31085=DIRECTION('',(1.,0.,0.));
#31086=DIRECTION('center_axis',(0.,1.,0.));
#31087=DIRECTION('ref_axis',(1.,0.,0.));
#31088=DIRECTION('',(0.,1.,0.));
#31089=DIRECTION('center_axis',(0.,-1.,0.));
#31090=DIRECTION('ref_axis',(1.,0.,0.));
#31091=DIRECTION('center_axis',(0.,-1.,0.));
#31092=DIRECTION('ref_axis',(1.,0.,0.));
#31093=DIRECTION('center_axis',(0.,-1.,0.));
#31094=DIRECTION('ref_axis',(1.,0.,0.));
#31095=DIRECTION('center_axis',(0.,-1.,0.));
#31096=DIRECTION('ref_axis',(1.,0.,0.));
#31097=DIRECTION('',(0.707106781186554,0.707106781186541,8.65956056235501E-17));
#31098=DIRECTION('center_axis',(0.,-1.,0.));
#31099=DIRECTION('ref_axis',(0.,0.,-1.));
#31100=DIRECTION('',(0.,0.,1.));
#31101=DIRECTION('',(-1.,0.,0.));
#31102=DIRECTION('',(0.,0.,-1.));
#31103=DIRECTION('',(1.,0.,0.));
#31104=DIRECTION('center_axis',(0.,-1.,0.));
#31105=DIRECTION('ref_axis',(1.,0.,0.));
#31106=DIRECTION('center_axis',(0.,-1.,0.));
#31107=DIRECTION('ref_axis',(1.,0.,0.));
#31108=DIRECTION('center_axis',(0.,-1.,0.));
#31109=DIRECTION('ref_axis',(1.,0.,0.));
#31110=DIRECTION('center_axis',(0.,-1.,0.));
#31111=DIRECTION('ref_axis',(1.,0.,0.));
#31112=DIRECTION('',(0.707106781186554,0.707106781186541,8.65956056235501E-17));
#31113=DIRECTION('center_axis',(0.,-1.,0.));
#31114=DIRECTION('ref_axis',(1.,0.,0.));
#31115=DIRECTION('',(0.707106781186554,0.707106781186541,8.65956056235501E-17));
#31116=DIRECTION('center_axis',(0.,-1.,0.));
#31117=DIRECTION('ref_axis',(1.,0.,0.));
#31118=DIRECTION('',(0.707106781186554,0.707106781186541,8.65956056235501E-17));
#31119=DIRECTION('center_axis',(-1.,0.,0.));
#31120=DIRECTION('ref_axis',(0.,-0.707106781186543,-0.707106781186552));
#31121=DIRECTION('',(-0.707106781186566,-0.707106781186529,0.));
#31122=DIRECTION('center_axis',(1.,0.,0.));
#31123=DIRECTION('ref_axis',(0.,-0.707106781186543,-0.707106781186552));
#31124=DIRECTION('',(0.707106781186548,0.,0.707106781186548));
#31125=DIRECTION('center_axis',(-1.,0.,0.));
#31126=DIRECTION('ref_axis',(0.,-0.707106781186543,-0.707106781186552));
#31127=DIRECTION('center_axis',(0.707106781186566,-0.707106781186529,0.));
#31128=DIRECTION('ref_axis',(0.,0.,-1.));
#31129=DIRECTION('',(0.,0.,1.));
#31130=DIRECTION('',(-0.707106781186529,-0.707106781186566,0.));
#31131=DIRECTION('',(0.,0.,-1.));
#31132=DIRECTION('center_axis',(-1.,0.,0.));
#31133=DIRECTION('ref_axis',(0.,-0.707106781186543,0.707106781186552));
#31134=DIRECTION('',(-0.707106781186548,0.,0.707106781186548));
#31135=DIRECTION('center_axis',(-1.,0.,0.));
#31136=DIRECTION('ref_axis',(0.,-0.707106781186543,0.707106781186552));
#31137=DIRECTION('center_axis',(0.707106781186548,0.,0.707106781186548));
#31138=DIRECTION('ref_axis',(0.707106781186548,0.,-0.707106781186548));
#31139=DIRECTION('',(0.,1.,0.));
#31140=DIRECTION('',(-0.707106781186548,0.,0.707106781186548));
#31141=DIRECTION('',(0.,-1.,0.));
#31142=DIRECTION('center_axis',(-1.,0.,0.));
#31143=DIRECTION('ref_axis',(0.,0.707106781186543,0.707106781186552));
#31144=DIRECTION('',(-0.707106781186566,0.707106781186529,0.));
#31145=DIRECTION('center_axis',(1.,0.,0.));
#31146=DIRECTION('ref_axis',(0.,0.707106781186543,0.707106781186552));
#31147=DIRECTION('center_axis',(-1.,0.,0.));
#31148=DIRECTION('ref_axis',(0.,0.707106781186543,0.707106781186552));
#31149=DIRECTION('center_axis',(0.707106781186566,0.707106781186529,0.));
#31150=DIRECTION('ref_axis',(0.,0.,-1.));
#31151=DIRECTION('',(0.,0.,-1.));
#31152=DIRECTION('',(-0.707106781186529,0.707106781186566,0.));
#31153=DIRECTION('center_axis',(-1.,0.,0.));
#31154=DIRECTION('ref_axis',(0.,0.707106781186542,-0.707106781186553));
#31155=DIRECTION('',(-0.707106781186548,0.,-0.707106781186548));
#31156=DIRECTION('center_axis',(1.,0.,0.));
#31157=DIRECTION('ref_axis',(0.,0.707106781186542,-0.707106781186553));
#31158=DIRECTION('center_axis',(-1.,0.,0.));
#31159=DIRECTION('ref_axis',(0.,0.707106781186542,-0.707106781186553));
#31160=DIRECTION('center_axis',(0.707106781186548,0.,-0.707106781186548));
#31161=DIRECTION('ref_axis',(-0.707106781186548,0.,-0.707106781186548));
#31162=DIRECTION('',(0.,-1.,0.));
#31163=DIRECTION('',(0.,1.,0.));
#31164=DIRECTION('center_axis',(1.,0.,0.));
#31165=DIRECTION('ref_axis',(0.,0.707106781186542,-0.707106781186553));
#31166=DIRECTION('',(-1.,0.,0.));
#31167=DIRECTION('',(-1.,0.,0.));
#31168=DIRECTION('',(-1.,0.,0.));
#31169=DIRECTION('center_axis',(-1.,0.,0.));
#31170=DIRECTION('ref_axis',(0.,0.707106781186542,-0.707106781186553));
#31171=DIRECTION('center_axis',(0.,0.,-1.));
#31172=DIRECTION('ref_axis',(0.,1.,0.));
#31173=DIRECTION('',(1.,0.,0.));
#31174=DIRECTION('center_axis',(1.,0.,0.));
#31175=DIRECTION('ref_axis',(0.,-0.707106781186543,-0.707106781186552));
#31176=DIRECTION('',(-1.,0.,0.));
#31177=DIRECTION('',(-1.,0.,0.));
#31178=DIRECTION('',(-1.,0.,0.));
#31179=DIRECTION('center_axis',(-1.,0.,0.));
#31180=DIRECTION('ref_axis',(0.,-0.707106781186543,-0.707106781186552));
#31181=DIRECTION('',(1.,0.,0.));
#31182=DIRECTION('center_axis',(1.,0.,0.));
#31183=DIRECTION('ref_axis',(0.,0.,-1.));
#31184=DIRECTION('',(0.,0.,-1.));
#31185=DIRECTION('center_axis',(1.,0.,0.));
#31186=DIRECTION('ref_axis',(0.,-0.707106781186568,0.707106781186527));
#31187=DIRECTION('',(0.,-1.,0.));
#31188=DIRECTION('center_axis',(1.,0.,0.));
#31189=DIRECTION('ref_axis',(0.,0.707106781186568,0.707106781186527));
#31190=DIRECTION('',(0.,0.,1.));
#31191=DIRECTION('center_axis',(1.,0.,0.));
#31192=DIRECTION('ref_axis',(0.,0.707106781186568,-0.707106781186527));
#31193=DIRECTION('',(0.,1.,0.));
#31194=DIRECTION('center_axis',(1.,0.,0.));
#31195=DIRECTION('ref_axis',(0.,-0.707106781186566,-0.707106781186529));
#31196=DIRECTION('center_axis',(1.,0.,0.));
#31197=DIRECTION('ref_axis',(0.,-0.707106781186543,-0.707106781186552));
#31198=DIRECTION('',(0.707106781186573,0.,-0.707106781186522));
#31199=DIRECTION('',(-0.707106781186592,0.707106781186504,0.));
#31200=DIRECTION('center_axis',(1.,0.,0.));
#31201=DIRECTION('ref_axis',(0.,-0.707106781186543,-0.707106781186552));
#31202=DIRECTION('center_axis',(-0.707106781186548,0.,-0.707106781186548));
#31203=DIRECTION('ref_axis',(-0.707106781186548,0.,0.707106781186548));
#31204=DIRECTION('',(0.,1.,0.));
#31205=DIRECTION('',(0.707106781186548,0.,-0.707106781186548));
#31206=DIRECTION('',(0.,-1.,0.));
#31207=DIRECTION('center_axis',(1.,0.,0.));
#31208=DIRECTION('ref_axis',(0.,0.707106781186542,-0.707106781186553));
#31209=DIRECTION('',(0.707106781186592,0.707106781186504,0.));
#31210=DIRECTION('center_axis',(1.,0.,0.));
#31211=DIRECTION('ref_axis',(0.,0.707106781186542,-0.707106781186553));
#31212=DIRECTION('center_axis',(-0.707106781186566,0.707106781186529,0.));
#31213=DIRECTION('ref_axis',(0.,0.,1.));
#31214=DIRECTION('',(0.,0.,1.));
#31215=DIRECTION('',(0.707106781186529,0.707106781186566,0.));
#31216=DIRECTION('center_axis',(1.,0.,0.));
#31217=DIRECTION('ref_axis',(0.,0.707106781186543,0.707106781186552));
#31218=DIRECTION('',(0.707106781186573,0.,0.707106781186522));
#31219=DIRECTION('center_axis',(-1.,0.,0.));
#31220=DIRECTION('ref_axis',(0.,0.707106781186543,0.707106781186552));
#31221=DIRECTION('center_axis',(1.,0.,0.));
#31222=DIRECTION('ref_axis',(0.,0.707106781186543,0.707106781186552));
#31223=DIRECTION('center_axis',(-0.707106781186548,0.,0.707106781186548));
#31224=DIRECTION('ref_axis',(0.707106781186548,0.,0.707106781186548));
#31225=DIRECTION('',(0.,-1.,0.));
#31226=DIRECTION('',(0.707106781186548,0.,0.707106781186548));
#31227=DIRECTION('',(0.,1.,0.));
#31228=DIRECTION('center_axis',(1.,0.,0.));
#31229=DIRECTION('ref_axis',(0.,-0.707106781186543,0.707106781186552));
#31230=DIRECTION('',(0.707106781186592,-0.707106781186504,0.));
#31231=DIRECTION('center_axis',(1.,0.,0.));
#31232=DIRECTION('ref_axis',(0.,-0.707106781186543,0.707106781186552));
#31233=DIRECTION('center_axis',(-0.707106781186566,-0.707106781186529,0.));
#31234=DIRECTION('ref_axis',(0.,0.,1.));
#31235=DIRECTION('',(0.,0.,-1.));
#31236=DIRECTION('',(0.,0.,1.));
#31237=DIRECTION('center_axis',(0.,0.,1.));
#31238=DIRECTION('ref_axis',(0.,-1.,0.));
#31239=DIRECTION('',(1.,0.,0.));
#31240=DIRECTION('center_axis',(0.,-1.,0.));
#31241=DIRECTION('ref_axis',(0.,0.,-1.));
#31242=DIRECTION('center_axis',(0.,-1.,0.));
#31243=DIRECTION('ref_axis',(1.,0.,0.));
#31244=DIRECTION('center_axis',(0.,-1.,0.));
#31245=DIRECTION('ref_axis',(1.,0.,0.));
#31246=DIRECTION('center_axis',(0.,-1.,0.));
#31247=DIRECTION('ref_axis',(1.,0.,0.));
#31248=DIRECTION('',(-1.,0.,0.));
#31249=DIRECTION('',(0.,0.,1.));
#31250=DIRECTION('',(1.,0.,0.));
#31251=DIRECTION('',(0.,0.,-1.));
#31252=DIRECTION('',(-1.,0.,0.));
#31253=DIRECTION('',(0.,0.,-1.));
#31254=DIRECTION('',(-1.,0.,0.));
#31255=DIRECTION('',(0.,0.,1.));
#31256=DIRECTION('',(1.,0.,0.));
#31257=DIRECTION('',(0.,0.,-1.));
#31258=DIRECTION('',(-1.,0.,0.));
#31259=DIRECTION('',(-0.996744950321709,0.,0.0806195014135826));
#31260=DIRECTION('',(-1.,0.,0.));
#31261=DIRECTION('',(0.,0.,1.));
#31262=DIRECTION('',(1.,0.,0.));
#31263=DIRECTION('',(0.562642705730145,0.,-0.826700178836718));
#31264=DIRECTION('',(0.,0.,1.));
#31265=DIRECTION('',(1.,0.,0.));
#31266=DIRECTION('',(0.,0.,-1.));
#31267=DIRECTION('',(-1.,0.,0.));
#31268=DIRECTION('',(-0.563462182256227,0.,0.826141857774468));
#31269=DIRECTION('',(0.,0.,-1.));
#31270=DIRECTION('center_axis',(1.,0.,0.));
#31271=DIRECTION('ref_axis',(0.,0.,-1.));
#31272=DIRECTION('',(0.,0.,1.));
#31273=DIRECTION('center_axis',(-1.,0.,0.));
#31274=DIRECTION('ref_axis',(0.,-0.707106781186566,-0.707106781186529));
#31275=DIRECTION('',(0.,-1.,0.));
#31276=DIRECTION('center_axis',(-1.,0.,0.));
#31277=DIRECTION('ref_axis',(0.,0.707106781186568,-0.707106781186527));
#31278=DIRECTION('',(0.,0.,-1.));
#31279=DIRECTION('center_axis',(-1.,0.,0.));
#31280=DIRECTION('ref_axis',(0.,0.707106781186568,0.707106781186527));
#31281=DIRECTION('',(0.,1.,0.));
#31282=DIRECTION('center_axis',(-1.,0.,0.));
#31283=DIRECTION('ref_axis',(0.,-0.707106781186568,0.707106781186527));
#31284=DIRECTION('center_axis',(0.,-1.,0.));
#31285=DIRECTION('ref_axis',(-1.83697019872103E-16,0.,1.));
#31286=DIRECTION('',(0.315789473684196,0.707106781186531,0.632674488430095));
#31287=DIRECTION('center_axis',(0.,1.,0.));
#31288=DIRECTION('ref_axis',(1.,0.,0.));
#31289=DIRECTION('center_axis',(0.,1.,0.));
#31290=DIRECTION('ref_axis',(1.,0.,0.));
#31291=DIRECTION('',(0.315789473684196,-0.707106781186531,-0.632674488430095));
#31292=DIRECTION('',(-0.238798209365739,-0.687106448937468,-0.686192497067885));
#31293=DIRECTION('',(-0.238798209365764,0.687106448937464,0.686192497067881));
#31294=DIRECTION('center_axis',(0.,1.,0.));
#31295=DIRECTION('ref_axis',(1.,0.,0.));
#31296=DIRECTION('',(0.,1.,0.));
#31297=DIRECTION('center_axis',(0.,-1.,0.));
#31298=DIRECTION('ref_axis',(1.,0.,0.));
#31299=DIRECTION('center_axis',(0.,-1.,0.));
#31300=DIRECTION('ref_axis',(1.,0.,0.));
#31301=DIRECTION('center_axis',(0.,-1.,0.));
#31302=DIRECTION('ref_axis',(6.12323399573677E-17,0.,-1.));
#31303=DIRECTION('',(-0.315789473684196,0.707106781186531,-0.632674488430095));
#31304=DIRECTION('center_axis',(0.,1.,0.));
#31305=DIRECTION('ref_axis',(1.,0.,0.));
#31306=DIRECTION('center_axis',(0.,1.,0.));
#31307=DIRECTION('ref_axis',(1.,0.,0.));
#31308=DIRECTION('',(-0.315789473684196,-0.707106781186531,0.632674488430095));
#31309=DIRECTION('',(0.238798209365739,-0.687106448937468,0.686192497067885));
#31310=DIRECTION('',(0.238798209365798,0.687106448937561,-0.686192497067771));
#31311=DIRECTION('center_axis',(0.,1.,0.));
#31312=DIRECTION('ref_axis',(1.,0.,0.));
#31313=DIRECTION('',(0.,1.,0.));
#31314=DIRECTION('center_axis',(0.,-1.,0.));
#31315=DIRECTION('ref_axis',(1.,0.,0.));
#31316=DIRECTION('center_axis',(0.,-1.,0.));
#31317=DIRECTION('ref_axis',(1.,0.,0.));
#31318=DIRECTION('center_axis',(-0.707106781186541,0.707106781186554,0.));
#31319=DIRECTION('ref_axis',(0.,0.,1.));
#31320=DIRECTION('',(0.707106781186554,0.707106781186541,0.));
#31321=DIRECTION('',(0.,0.,-1.));
#31322=DIRECTION('',(-0.707106781186554,-0.707106781186541,0.));
#31323=DIRECTION('center_axis',(-1.,0.,0.));
#31324=DIRECTION('ref_axis',(0.,-0.707106781186568,0.707106781186527));
#31325=DIRECTION('',(0.707106781186673,0.,-0.707106781186422));
#31326=DIRECTION('center_axis',(1.,0.,0.));
#31327=DIRECTION('ref_axis',(0.,-0.707106781186568,0.707106781186527));
#31328=DIRECTION('center_axis',(-0.707106781186522,0.,-0.707106781186573));
#31329=DIRECTION('ref_axis',(-0.707106781186573,0.,0.707106781186522));
#31330=DIRECTION('',(0.707106781186573,0.,-0.707106781186522));
#31331=DIRECTION('',(0.,-1.,0.));
#31332=DIRECTION('center_axis',(-1.,0.,0.));
#31333=DIRECTION('ref_axis',(0.,0.707106781186568,0.707106781186527));
#31334=DIRECTION('',(0.707106781186607,-0.707106781186488,0.));
#31335=DIRECTION('center_axis',(1.,0.,0.));
#31336=DIRECTION('ref_axis',(0.,0.707106781186568,0.707106781186527));
#31337=DIRECTION('center_axis',(-0.707106781186541,-0.707106781186554,0.));
#31338=DIRECTION('ref_axis',(0.,0.,1.));
#31339=DIRECTION('',(0.707106781186554,-0.707106781186541,0.));
#31340=DIRECTION('center_axis',(-1.,0.,0.));
#31341=DIRECTION('ref_axis',(0.,0.707106781186568,-0.707106781186527));
#31342=DIRECTION('',(0.707106781186673,0.,0.707106781186422));
#31343=DIRECTION('center_axis',(1.,0.,0.));
#31344=DIRECTION('ref_axis',(0.,0.707106781186568,-0.707106781186527));
#31345=DIRECTION('center_axis',(-0.707106781186522,0.,0.707106781186573));
#31346=DIRECTION('ref_axis',(0.707106781186573,0.,0.707106781186522));
#31347=DIRECTION('',(0.707106781186573,0.,0.707106781186522));
#31348=DIRECTION('',(0.,1.,0.));
#31349=DIRECTION('center_axis',(-1.,0.,0.));
#31350=DIRECTION('ref_axis',(0.,-0.707106781186566,-0.707106781186529));
#31351=DIRECTION('center_axis',(1.,0.,0.));
#31352=DIRECTION('ref_axis',(0.,-0.707106781186566,-0.707106781186529));
#31353=DIRECTION('center_axis',(1.,0.,0.));
#31354=DIRECTION('ref_axis',(0.,0.707106781186568,-0.707106781186527));
#31355=DIRECTION('',(1.,0.,0.));
#31356=DIRECTION('center_axis',(-1.,0.,0.));
#31357=DIRECTION('ref_axis',(0.,0.707106781186568,-0.707106781186527));
#31358=DIRECTION('center_axis',(0.,0.,1.));
#31359=DIRECTION('ref_axis',(0.,-1.,0.));
#31360=DIRECTION('',(-1.,0.,0.));
#31361=DIRECTION('',(0.,-1.,0.));
#31362=DIRECTION('center_axis',(1.,0.,0.));
#31363=DIRECTION('ref_axis',(0.,-0.707106781186566,-0.707106781186529));
#31364=DIRECTION('',(1.,0.,0.));
#31365=DIRECTION('',(1.,0.,0.));
#31366=DIRECTION('',(1.,0.,0.));
#31367=DIRECTION('center_axis',(-1.,0.,0.));
#31368=DIRECTION('ref_axis',(0.,-0.707106781186566,-0.707106781186529));
#31369=DIRECTION('center_axis',(0.,1.,0.));
#31370=DIRECTION('ref_axis',(0.,0.,1.));
#31371=DIRECTION('',(-1.,0.,0.));
#31372=DIRECTION('center_axis',(0.,1.,0.));
#31373=DIRECTION('ref_axis',(1.,0.,0.));
#31374=DIRECTION('',(-1.,0.,0.));
#31375=DIRECTION('center_axis',(0.,1.,0.));
#31376=DIRECTION('ref_axis',(1.,0.,0.));
#31377=DIRECTION('',(-1.,0.,0.));
#31378=DIRECTION('',(0.,0.,1.));
#31379=DIRECTION('center_axis',(0.,1.,0.));
#31380=DIRECTION('ref_axis',(1.,0.,0.));
#31381=DIRECTION('center_axis',(0.,1.,0.));
#31382=DIRECTION('ref_axis',(1.,0.,0.));
#31383=DIRECTION('',(0.373458905374385,-0.737256835467264,0.563010483519946));
#31384=DIRECTION('',(-0.373458905374355,-0.737256835467348,0.563010483519854));
#31385=DIRECTION('center_axis',(0.,1.,0.));
#31386=DIRECTION('ref_axis',(6.12323399573677E-17,0.,1.));
#31387=DIRECTION('',(-0.43401111848607,-0.707106781186588,0.558242195673539));
#31388=DIRECTION('',(-0.43401111848607,0.707106781186588,-0.558242195673539));
#31389=DIRECTION('center_axis',(0.707106781186566,0.707106781186529,0.));
#31390=DIRECTION('ref_axis',(0.,0.,-1.));
#31391=DIRECTION('',(0.707106781186529,-0.707106781186566,0.));
#31392=DIRECTION('',(-0.707106781186529,0.707106781186566,0.));
#31393=DIRECTION('center_axis',(1.,0.,0.));
#31394=DIRECTION('ref_axis',(0.,-0.707106781186568,0.707106781186527));
#31395=DIRECTION('center_axis',(-1.,0.,0.));
#31396=DIRECTION('ref_axis',(0.,-0.707106781186568,0.707106781186527));
#31397=DIRECTION('',(0.707106781186648,0.,0.707106781186447));
#31398=DIRECTION('center_axis',(0.707106781186548,0.,-0.707106781186548));
#31399=DIRECTION('ref_axis',(-0.707106781186548,0.,-0.707106781186548));
#31400=DIRECTION('',(0.707106781186548,0.,0.707106781186548));
#31401=DIRECTION('',(0.,1.,0.));
#31402=DIRECTION('center_axis',(1.,0.,0.));
#31403=DIRECTION('ref_axis',(0.,0.707106781186568,0.707106781186527));
#31404=DIRECTION('center_axis',(-1.,0.,0.));
#31405=DIRECTION('ref_axis',(0.,0.707106781186568,0.707106781186527));
#31406=DIRECTION('',(0.707106781186582,0.707106781186513,0.));
#31407=DIRECTION('center_axis',(0.707106781186566,-0.707106781186529,0.));
#31408=DIRECTION('ref_axis',(0.,0.,-1.));
#31409=DIRECTION('',(0.707106781186529,0.707106781186566,0.));
#31410=DIRECTION('center_axis',(1.,0.,0.));
#31411=DIRECTION('ref_axis',(0.,0.707106781186568,-0.707106781186527));
#31412=DIRECTION('',(0.707106781186648,0.,-0.707106781186447));
#31413=DIRECTION('center_axis',(0.707106781186548,0.,0.707106781186548));
#31414=DIRECTION('ref_axis',(0.707106781186548,0.,-0.707106781186548));
#31415=DIRECTION('',(0.707106781186548,0.,-0.707106781186548));
#31416=DIRECTION('center_axis',(1.,0.,0.));
#31417=DIRECTION('ref_axis',(0.,-0.707106781186566,-0.707106781186529));
#31418=DIRECTION('center_axis',(1.,0.,0.));
#31419=DIRECTION('ref_axis',(0.,0.707106781186568,0.707106781186527));
#31420=DIRECTION('',(-1.,0.,0.));
#31421=DIRECTION('center_axis',(0.,0.,-1.));
#31422=DIRECTION('ref_axis',(0.,1.,0.));
#31423=DIRECTION('',(1.,0.,0.));
#31424=DIRECTION('center_axis',(1.,0.,0.));
#31425=DIRECTION('ref_axis',(0.,-0.707106781186568,0.707106781186527));
#31426=DIRECTION('',(-0.373458905374326,-0.737256835467278,-0.563010483519966));
#31427=DIRECTION('',(0.373458905374459,-0.737256835467315,-0.563010483519829));
#31428=DIRECTION('center_axis',(0.,1.,0.));
#31429=DIRECTION('ref_axis',(-1.83697019872103E-16,0.,-1.));
#31430=DIRECTION('',(0.43401111848607,-0.707106781186588,-0.558242195673539));
#31431=DIRECTION('',(0.43401111848607,0.707106781186588,0.558242195673539));
#31432=DIRECTION('',(-0.373458905374367,-0.737256835467265,-0.563010483519956));
#31433=DIRECTION('',(0.373458905374397,-0.737256835467335,-0.563010483519844));
#31434=DIRECTION('center_axis',(0.,1.,0.));
#31435=DIRECTION('ref_axis',(-1.83697019872103E-16,0.,-1.));
#31436=DIRECTION('',(0.43401111848607,-0.707106781186588,-0.558242195673539));
#31437=DIRECTION('',(0.43401111848607,0.707106781186588,0.558242195673539));
#31438=DIRECTION('center_axis',(0.,-1.,0.));
#31439=DIRECTION('ref_axis',(-1.83697019872103E-16,0.,1.));
#31440=DIRECTION('',(0.315789473684196,0.707106781186531,0.632674488430095));
#31441=DIRECTION('center_axis',(0.,1.,0.));
#31442=DIRECTION('ref_axis',(1.,0.,0.));
#31443=DIRECTION('center_axis',(0.,1.,0.));
#31444=DIRECTION('ref_axis',(1.,0.,0.));
#31445=DIRECTION('',(0.315789473684196,-0.707106781186531,-0.632674488430095));
#31446=DIRECTION('',(-0.238798209365739,-0.687106448937468,-0.686192497067885));
#31447=DIRECTION('',(-0.23879820936573,0.687106448937366,0.68619249706799));
#31448=DIRECTION('center_axis',(0.,1.,0.));
#31449=DIRECTION('ref_axis',(1.,0.,0.));
#31450=DIRECTION('',(0.,1.,0.));
#31451=DIRECTION('center_axis',(0.,-1.,0.));
#31452=DIRECTION('ref_axis',(1.,0.,0.));
#31453=DIRECTION('center_axis',(0.,-1.,0.));
#31454=DIRECTION('ref_axis',(1.,0.,0.));
#31455=DIRECTION('',(0.373458905374429,-0.737256835467245,0.56301048351994));
#31456=DIRECTION('',(-0.373458905374459,-0.737256835467315,0.563010483519829));
#31457=DIRECTION('center_axis',(0.,1.,0.));
#31458=DIRECTION('ref_axis',(6.12323399573677E-17,0.,1.));
#31459=DIRECTION('',(-0.43401111848607,-0.707106781186588,0.558242195673539));
#31460=DIRECTION('',(-0.43401111848607,0.707106781186588,-0.558242195673539));
#31461=DIRECTION('center_axis',(1.,0.,0.));
#31462=DIRECTION('ref_axis',(0.,0.707106781186543,-0.707106781186552));
#31463=DIRECTION('',(0.707106781186592,0.707106781186504,0.));
#31464=DIRECTION('center_axis',(-1.,0.,0.));
#31465=DIRECTION('ref_axis',(0.,0.707106781186543,-0.707106781186552));
#31466=DIRECTION('',(-0.707106781186573,0.,0.707106781186522));
#31467=DIRECTION('center_axis',(1.,0.,0.));
#31468=DIRECTION('ref_axis',(0.,0.707106781186543,-0.707106781186552));
#31469=DIRECTION('center_axis',(-0.707106781186541,0.707106781186554,0.));
#31470=DIRECTION('ref_axis',(0.,0.,1.));
#31471=DIRECTION('',(0.707106781186554,0.707106781186541,0.));
#31472=DIRECTION('',(0.,0.,-1.));
#31473=DIRECTION('',(0.,0.,1.));
#31474=DIRECTION('center_axis',(1.,0.,0.));
#31475=DIRECTION('ref_axis',(0.,0.707106781186543,0.707106781186552));
#31476=DIRECTION('',(0.707106781186573,0.,0.707106781186522));
#31477=DIRECTION('center_axis',(-1.,0.,0.));
#31478=DIRECTION('ref_axis',(0.,0.707106781186543,0.707106781186552));
#31479=DIRECTION('center_axis',(1.,0.,0.));
#31480=DIRECTION('ref_axis',(0.,0.707106781186543,0.707106781186552));
#31481=DIRECTION('center_axis',(-0.707106781186623,0.,0.707106781186472));
#31482=DIRECTION('ref_axis',(0.707106781186472,0.,0.707106781186623));
#31483=DIRECTION('',(0.707106781186472,0.,0.707106781186623));
#31484=DIRECTION('',(0.,1.,0.));
#31485=DIRECTION('',(0.,-1.,0.));
#31486=DIRECTION('center_axis',(1.,0.,0.));
#31487=DIRECTION('ref_axis',(0.,-0.707106781186542,0.707106781186553));
#31488=DIRECTION('',(0.707106781186592,-0.707106781186504,0.));
#31489=DIRECTION('center_axis',(-1.,0.,0.));
#31490=DIRECTION('ref_axis',(0.,-0.707106781186542,0.707106781186553));
#31491=DIRECTION('center_axis',(1.,0.,0.));
#31492=DIRECTION('ref_axis',(0.,-0.707106781186542,0.707106781186553));
#31493=DIRECTION('center_axis',(-0.707106781186541,-0.707106781186554,0.));
#31494=DIRECTION('ref_axis',(0.,0.,1.));
#31495=DIRECTION('',(0.707106781186554,-0.707106781186541,0.));
#31496=DIRECTION('',(0.,0.,-1.));
#31497=DIRECTION('center_axis',(1.,0.,0.));
#31498=DIRECTION('ref_axis',(0.,-0.707106781186543,-0.707106781186552));
#31499=DIRECTION('',(0.707106781186573,0.,-0.707106781186522));
#31500=DIRECTION('center_axis',(-1.,0.,0.));
#31501=DIRECTION('ref_axis',(0.,-0.707106781186543,-0.707106781186552));
#31502=DIRECTION('center_axis',(1.,0.,0.));
#31503=DIRECTION('ref_axis',(0.,-0.707106781186543,-0.707106781186552));
#31504=DIRECTION('center_axis',(-0.707106781186623,0.,-0.707106781186472));
#31505=DIRECTION('ref_axis',(-0.707106781186472,0.,0.707106781186623));
#31506=DIRECTION('',(0.,-1.,0.));
#31507=DIRECTION('',(0.,1.,0.));
#31508=DIRECTION('center_axis',(1.,0.,0.));
#31509=DIRECTION('ref_axis',(0.,-0.707106781186543,-0.707106781186552));
#31510=DIRECTION('',(1.,0.,0.));
#31511=DIRECTION('',(1.,0.,0.));
#31512=DIRECTION('',(1.,0.,0.));
#31513=DIRECTION('center_axis',(1.,0.,0.));
#31514=DIRECTION('ref_axis',(0.,-0.707106781186543,-0.707106781186552));
#31515=DIRECTION('center_axis',(0.,0.,-1.));
#31516=DIRECTION('ref_axis',(0.,1.,0.));
#31517=DIRECTION('',(-1.,0.,0.));
#31518=DIRECTION('',(0.,-1.,0.));
#31519=DIRECTION('center_axis',(1.,0.,0.));
#31520=DIRECTION('ref_axis',(0.,0.707106781186543,-0.707106781186552));
#31521=DIRECTION('',(1.,0.,0.));
#31522=DIRECTION('',(1.,0.,0.));
#31523=DIRECTION('',(1.,0.,0.));
#31524=DIRECTION('center_axis',(1.,0.,0.));
#31525=DIRECTION('ref_axis',(0.,0.707106781186543,-0.707106781186552));
#31526=DIRECTION('',(-1.,0.,0.));
#31527=DIRECTION('',(-1.,0.,0.));
#31528=DIRECTION('center_axis',(1.,0.,0.));
#31529=DIRECTION('ref_axis',(0.,0.,-1.));
#31530=DIRECTION('',(0.,0.,-1.));
#31531=DIRECTION('center_axis',(-1.,0.,0.));
#31532=DIRECTION('ref_axis',(0.,0.707106781186566,0.707106781186529));
#31533=DIRECTION('',(0.,1.,0.));
#31534=DIRECTION('center_axis',(-1.,0.,0.));
#31535=DIRECTION('ref_axis',(0.,-0.707106781186568,0.707106781186527));
#31536=DIRECTION('',(0.,0.,1.));
#31537=DIRECTION('center_axis',(-1.,0.,0.));
#31538=DIRECTION('ref_axis',(0.,-0.707106781186568,-0.707106781186527));
#31539=DIRECTION('',(0.,-1.,0.));
#31540=DIRECTION('center_axis',(-1.,0.,0.));
#31541=DIRECTION('ref_axis',(0.,0.707106781186568,-0.707106781186527));
#31542=DIRECTION('center_axis',(-1.,0.,0.));
#31543=DIRECTION('ref_axis',(0.,0.707106781186543,-0.707106781186552));
#31544=DIRECTION('',(-0.707106781186548,0.,-0.707106781186548));
#31545=DIRECTION('',(0.707106781186566,-0.707106781186529,0.));
#31546=DIRECTION('center_axis',(-1.,0.,0.));
#31547=DIRECTION('ref_axis',(0.,0.707106781186543,-0.707106781186552));
#31548=DIRECTION('center_axis',(0.707106781186548,0.,-0.707106781186548));
#31549=DIRECTION('ref_axis',(-0.707106781186548,0.,-0.707106781186548));
#31550=DIRECTION('',(0.,-1.,0.));
#31551=DIRECTION('',(-0.707106781186548,0.,-0.707106781186548));
#31552=DIRECTION('',(0.,1.,0.));
#31553=DIRECTION('center_axis',(-1.,0.,0.));
#31554=DIRECTION('ref_axis',(0.,-0.707106781186543,-0.707106781186552));
#31555=DIRECTION('',(-0.707106781186566,-0.707106781186529,0.));
#31556=DIRECTION('center_axis',(-1.,0.,0.));
#31557=DIRECTION('ref_axis',(0.,-0.707106781186543,-0.707106781186552));
#31558=DIRECTION('center_axis',(0.707106781186566,-0.707106781186529,0.));
#31559=DIRECTION('ref_axis',(0.,0.,-1.));
#31560=DIRECTION('',(0.,0.,1.));
#31561=DIRECTION('',(-0.707106781186529,-0.707106781186566,0.));
#31562=DIRECTION('center_axis',(-1.,0.,0.));
#31563=DIRECTION('ref_axis',(0.,-0.707106781186542,0.707106781186553));
#31564=DIRECTION('',(-0.707106781186548,0.,0.707106781186548));
#31565=DIRECTION('center_axis',(1.,0.,0.));
#31566=DIRECTION('ref_axis',(0.,-0.707106781186542,0.707106781186553));
#31567=DIRECTION('center_axis',(-1.,0.,0.));
#31568=DIRECTION('ref_axis',(0.,-0.707106781186542,0.707106781186553));
#31569=DIRECTION('center_axis',(0.707106781186548,0.,0.707106781186548));
#31570=DIRECTION('ref_axis',(0.707106781186548,0.,-0.707106781186548));
#31571=DIRECTION('',(0.,1.,0.));
#31572=DIRECTION('',(-0.707106781186548,0.,0.707106781186548));
#31573=DIRECTION('',(0.,-1.,0.));
#31574=DIRECTION('center_axis',(-1.,0.,0.));
#31575=DIRECTION('ref_axis',(0.,0.707106781186543,0.707106781186552));
#31576=DIRECTION('',(-0.707106781186566,0.707106781186529,0.));
#31577=DIRECTION('center_axis',(1.,0.,0.));
#31578=DIRECTION('ref_axis',(0.,0.707106781186543,0.707106781186552));
#31579=DIRECTION('center_axis',(-1.,0.,0.));
#31580=DIRECTION('ref_axis',(0.,0.707106781186543,0.707106781186552));
#31581=DIRECTION('center_axis',(0.707106781186566,0.707106781186529,0.));
#31582=DIRECTION('ref_axis',(0.,0.,-1.));
#31583=DIRECTION('',(0.,0.,-1.));
#31584=DIRECTION('',(0.,0.,1.));
#31585=DIRECTION('center_axis',(0.,0.,1.));
#31586=DIRECTION('ref_axis',(0.,-1.,0.));
#31587=DIRECTION('',(-1.,0.,0.));
#31588=DIRECTION('',(1.,0.,0.));
#31589=DIRECTION('center_axis',(1.,0.,0.));
#31590=DIRECTION('ref_axis',(0.,0.707106781186543,0.707106781186552));
#31591=DIRECTION('',(-1.,0.,0.));
#31592=DIRECTION('',(-1.,0.,0.));
#31593=DIRECTION('',(-1.,0.,0.));
#31594=DIRECTION('center_axis',(0.,1.,0.));
#31595=DIRECTION('ref_axis',(0.,0.,1.));
#31596=DIRECTION('center_axis',(0.,1.,0.));
#31597=DIRECTION('ref_axis',(1.,0.,0.));
#31598=DIRECTION('center_axis',(0.,1.,0.));
#31599=DIRECTION('ref_axis',(1.,0.,0.));
#31600=DIRECTION('center_axis',(0.,1.,0.));
#31601=DIRECTION('ref_axis',(1.,0.,0.));
#31602=DIRECTION('center_axis',(0.,1.,0.));
#31603=DIRECTION('ref_axis',(1.,0.,0.));
#31604=DIRECTION('center_axis',(1.,0.,0.));
#31605=DIRECTION('ref_axis',(0.,0.,-1.));
#31606=DIRECTION('',(0.,0.,1.));
#31607=DIRECTION('center_axis',(1.,0.,0.));
#31608=DIRECTION('ref_axis',(0.,0.707106781186568,-0.707106781186527));
#31609=DIRECTION('',(0.,1.,0.));
#31610=DIRECTION('center_axis',(1.,0.,0.));
#31611=DIRECTION('ref_axis',(0.,-0.707106781186568,-0.707106781186527));
#31612=DIRECTION('',(0.,0.,-1.));
#31613=DIRECTION('center_axis',(1.,0.,0.));
#31614=DIRECTION('ref_axis',(0.,-0.707106781186568,0.707106781186527));
#31615=DIRECTION('',(0.,-1.,0.));
#31616=DIRECTION('center_axis',(1.,0.,0.));
#31617=DIRECTION('ref_axis',(0.,0.707106781186566,0.707106781186529));
#31618=DIRECTION('',(-0.238798209365737,0.687106448937475,0.686192497067879));
#31619=DIRECTION('',(-0.238798209365775,-0.687106448937559,-0.686192497067782));
#31620=DIRECTION('center_axis',(0.,1.,0.));
#31621=DIRECTION('ref_axis',(-1.83697019872103E-16,0.,-1.));
#31622=DIRECTION('',(0.315789473684196,-0.707106781186531,-0.632674488430095));
#31623=DIRECTION('center_axis',(0.,-1.,0.));
#31624=DIRECTION('ref_axis',(1.,0.,0.));
#31625=DIRECTION('center_axis',(0.,-1.,0.));
#31626=DIRECTION('ref_axis',(1.,0.,0.));
#31627=DIRECTION('',(0.315789473684196,0.707106781186531,0.632674488430095));
#31628=DIRECTION('center_axis',(0.,-1.,0.));
#31629=DIRECTION('ref_axis',(1.,0.,0.));
#31630=DIRECTION('',(0.,-1.,0.));
#31631=DIRECTION('center_axis',(0.,1.,0.));
#31632=DIRECTION('ref_axis',(1.,0.,0.));
#31633=DIRECTION('center_axis',(0.,1.,0.));
#31634=DIRECTION('ref_axis',(1.,0.,0.));
#31635=DIRECTION('center_axis',(0.707106781186566,-0.707106781186529,0.));
#31636=DIRECTION('ref_axis',(0.,0.,-1.));
#31637=DIRECTION('',(0.707106781186529,0.707106781186566,0.));
#31638=DIRECTION('',(-0.707106781186529,-0.707106781186566,0.));
#31639=DIRECTION('',(0.,0.,-1.));
#31640=DIRECTION('center_axis',(1.,0.,0.));
#31641=DIRECTION('ref_axis',(0.,0.707106781186568,-0.707106781186527));
#31642=DIRECTION('center_axis',(-1.,0.,0.));
#31643=DIRECTION('ref_axis',(0.,0.707106781186568,-0.707106781186527));
#31644=DIRECTION('',(0.707106781186648,0.,-0.707106781186447));
#31645=DIRECTION('center_axis',(0.707106781186548,0.,0.707106781186548));
#31646=DIRECTION('ref_axis',(0.707106781186548,0.,-0.707106781186548));
#31647=DIRECTION('',(0.707106781186548,0.,-0.707106781186548));
#31648=DIRECTION('',(0.,-1.,0.));
#31649=DIRECTION('center_axis',(1.,0.,0.));
#31650=DIRECTION('ref_axis',(0.,-0.707106781186568,-0.707106781186527));
#31651=DIRECTION('center_axis',(-1.,0.,0.));
#31652=DIRECTION('ref_axis',(0.,-0.707106781186568,-0.707106781186527));
#31653=DIRECTION('',(0.707106781186582,-0.707106781186513,0.));
#31654=DIRECTION('center_axis',(0.707106781186566,0.707106781186529,0.));
#31655=DIRECTION('ref_axis',(0.,0.,-1.));
#31656=DIRECTION('',(0.707106781186529,-0.707106781186566,0.));
#31657=DIRECTION('center_axis',(1.,0.,0.));
#31658=DIRECTION('ref_axis',(0.,-0.707106781186568,0.707106781186527));
#31659=DIRECTION('center_axis',(-1.,0.,0.));
#31660=DIRECTION('ref_axis',(0.,-0.707106781186568,0.707106781186527));
#31661=DIRECTION('',(0.707106781186648,0.,0.707106781186447));
#31662=DIRECTION('center_axis',(0.707106781186548,0.,-0.707106781186548));
#31663=DIRECTION('ref_axis',(-0.707106781186548,0.,-0.707106781186548));
#31664=DIRECTION('',(0.707106781186548,0.,0.707106781186548));
#31665=DIRECTION('',(0.,1.,0.));
#31666=DIRECTION('center_axis',(1.,0.,0.));
#31667=DIRECTION('ref_axis',(0.,0.707106781186566,0.707106781186529));
#31668=DIRECTION('center_axis',(-1.,0.,0.));
#31669=DIRECTION('ref_axis',(0.,0.707106781186566,0.707106781186529));
#31670=DIRECTION('center_axis',(1.,0.,0.));
#31671=DIRECTION('ref_axis',(0.,-0.707106781186568,-0.707106781186527));
#31672=DIRECTION('',(-1.,0.,0.));
#31673=DIRECTION('center_axis',(1.,0.,0.));
#31674=DIRECTION('ref_axis',(0.,-0.707106781186568,-0.707106781186527));
#31675=DIRECTION('center_axis',(0.,0.,1.));
#31676=DIRECTION('ref_axis',(0.,-1.,0.));
#31677=DIRECTION('',(1.,0.,0.));
#31678=DIRECTION('',(0.,1.,0.));
#31679=DIRECTION('center_axis',(1.,0.,0.));
#31680=DIRECTION('ref_axis',(0.,0.707106781186568,-0.707106781186527));
#31681=DIRECTION('',(-1.,0.,0.));
#31682=DIRECTION('',(-1.,0.,0.));
#31683=DIRECTION('',(-1.,0.,0.));
#31684=DIRECTION('center_axis',(1.,0.,0.));
#31685=DIRECTION('ref_axis',(0.,0.707106781186568,-0.707106781186527));
#31686=DIRECTION('center_axis',(0.,-1.,0.));
#31687=DIRECTION('ref_axis',(0.,0.,-1.));
#31688=DIRECTION('',(1.,0.,0.));
#31689=DIRECTION('center_axis',(0.,-1.,0.));
#31690=DIRECTION('ref_axis',(1.,0.,0.));
#31691=DIRECTION('',(1.,0.,0.));
#31692=DIRECTION('center_axis',(0.,-1.,0.));
#31693=DIRECTION('ref_axis',(1.,0.,0.));
#31694=DIRECTION('',(1.,0.,0.));
#31695=DIRECTION('',(0.,0.,1.));
#31696=DIRECTION('center_axis',(0.,-1.,0.));
#31697=DIRECTION('ref_axis',(1.,0.,0.));
#31698=DIRECTION('center_axis',(0.,-1.,0.));
#31699=DIRECTION('ref_axis',(1.,0.,0.));
#31700=DIRECTION('center_axis',(-0.707106781186541,-0.707106781186554,0.));
#31701=DIRECTION('ref_axis',(0.,0.,1.));
#31702=DIRECTION('',(0.707106781186554,-0.707106781186541,0.));
#31703=DIRECTION('',(-0.707106781186554,0.707106781186541,0.));
#31704=DIRECTION('center_axis',(-1.,0.,0.));
#31705=DIRECTION('ref_axis',(0.,0.707106781186568,-0.707106781186527));
#31706=DIRECTION('',(0.707106781186673,0.,0.707106781186422));
#31707=DIRECTION('center_axis',(-0.707106781186522,0.,0.707106781186573));
#31708=DIRECTION('ref_axis',(0.707106781186573,0.,0.707106781186522));
#31709=DIRECTION('',(0.707106781186573,0.,0.707106781186522));
#31710=DIRECTION('center_axis',(-1.,0.,0.));
#31711=DIRECTION('ref_axis',(0.,-0.707106781186568,-0.707106781186527));
#31712=DIRECTION('',(0.707106781186607,0.707106781186488,0.));
#31713=DIRECTION('center_axis',(-0.707106781186541,0.707106781186554,0.));
#31714=DIRECTION('ref_axis',(0.,0.,1.));
#31715=DIRECTION('',(0.707106781186554,0.707106781186541,0.));
#31716=DIRECTION('center_axis',(-1.,0.,0.));
#31717=DIRECTION('ref_axis',(0.,-0.707106781186568,0.707106781186527));
#31718=DIRECTION('',(0.707106781186673,0.,-0.707106781186422));
#31719=DIRECTION('center_axis',(1.,0.,0.));
#31720=DIRECTION('ref_axis',(0.,-0.707106781186568,0.707106781186527));
#31721=DIRECTION('center_axis',(-0.707106781186522,0.,-0.707106781186573));
#31722=DIRECTION('ref_axis',(-0.707106781186573,0.,0.707106781186522));
#31723=DIRECTION('',(0.707106781186573,0.,-0.707106781186522));
#31724=DIRECTION('',(0.,-1.,0.));
#31725=DIRECTION('center_axis',(-1.,0.,0.));
#31726=DIRECTION('ref_axis',(0.,0.707106781186566,0.707106781186529));
#31727=DIRECTION('center_axis',(1.,0.,0.));
#31728=DIRECTION('ref_axis',(0.,0.707106781186566,0.707106781186529));
#31729=DIRECTION('center_axis',(1.,0.,0.));
#31730=DIRECTION('ref_axis',(0.,-0.707106781186568,0.707106781186527));
#31731=DIRECTION('',(1.,0.,0.));
#31732=DIRECTION('center_axis',(0.,0.,-1.));
#31733=DIRECTION('ref_axis',(0.,1.,0.));
#31734=DIRECTION('',(-1.,0.,0.));
#31735=DIRECTION('center_axis',(1.,0.,0.));
#31736=DIRECTION('ref_axis',(0.,0.707106781186566,0.707106781186529));
#31737=DIRECTION('',(0.373458905374385,0.737256835467264,-0.563010483519946));
#31738=DIRECTION('',(-0.373458905374456,0.73725683546732,-0.563010483519824));
#31739=DIRECTION('center_axis',(0.,-1.,0.));
#31740=DIRECTION('ref_axis',(6.12323399573677E-17,0.,-1.));
#31741=DIRECTION('',(-0.43401111848607,0.707106781186588,-0.558242195673539));
#31742=DIRECTION('',(-0.43401111848607,-0.707106781186588,0.558242195673539));
#31743=DIRECTION('center_axis',(0.,1.,0.));
#31744=DIRECTION('ref_axis',(6.12323399573677E-17,0.,1.));
#31745=DIRECTION('',(-0.315789473684196,-0.707106781186531,0.632674488430095));
#31746=DIRECTION('center_axis',(0.,-1.,0.));
#31747=DIRECTION('ref_axis',(1.,0.,0.));
#31748=DIRECTION('center_axis',(0.,-1.,0.));
#31749=DIRECTION('ref_axis',(1.,0.,0.));
#31750=DIRECTION('',(-0.315789473684196,0.707106781186531,-0.632674488430095));
#31751=DIRECTION('',(0.238798209365739,0.687106448937468,-0.686192497067885));
#31752=DIRECTION('',(0.238798209365766,-0.687106448937457,0.686192497067887));
#31753=DIRECTION('center_axis',(0.,-1.,0.));
#31754=DIRECTION('ref_axis',(1.,0.,0.));
#31755=DIRECTION('',(0.,-1.,0.));
#31756=DIRECTION('center_axis',(0.,1.,0.));
#31757=DIRECTION('ref_axis',(1.,0.,0.));
#31758=DIRECTION('center_axis',(0.,1.,0.));
#31759=DIRECTION('ref_axis',(1.,0.,0.));
#31760=DIRECTION('',(-0.373458905374388,0.737256835467258,0.563010483519951));
#31761=DIRECTION('',(0.3734589053744,0.737256835467329,0.563010483519849));
#31762=DIRECTION('center_axis',(0.,-1.,0.));
#31763=DIRECTION('ref_axis',(-1.83697019872103E-16,0.,1.));
#31764=DIRECTION('',(0.43401111848607,0.707106781186588,0.558242195673539));
#31765=DIRECTION('',(0.43401111848607,-0.707106781186588,-0.558242195673539));
#31766=DIRECTION('',(-0.238798209365762,0.687106448937471,0.686192497067875));
#31767=DIRECTION('',(-0.238798209365739,-0.687106448937468,-0.686192497067885));
#31768=DIRECTION('center_axis',(0.,1.,0.));
#31769=DIRECTION('ref_axis',(-1.83697019872103E-16,0.,-1.));
#31770=DIRECTION('',(0.315789473684196,-0.707106781186531,-0.632674488430095));
#31771=DIRECTION('center_axis',(0.,-1.,0.));
#31772=DIRECTION('ref_axis',(1.,0.,0.));
#31773=DIRECTION('center_axis',(0.,-1.,0.));
#31774=DIRECTION('ref_axis',(1.,0.,0.));
#31775=DIRECTION('',(0.315789473684196,0.707106781186531,0.632674488430095));
#31776=DIRECTION('center_axis',(0.,-1.,0.));
#31777=DIRECTION('ref_axis',(1.,0.,0.));
#31778=DIRECTION('',(0.,-1.,0.));
#31779=DIRECTION('center_axis',(0.,1.,0.));
#31780=DIRECTION('ref_axis',(1.,0.,0.));
#31781=DIRECTION('center_axis',(0.,1.,0.));
#31782=DIRECTION('ref_axis',(1.,0.,0.));
#31783=DIRECTION('',(0.373458905374343,0.737256835467277,-0.563010483519956));
#31784=DIRECTION('',(-0.373458905374373,0.737256835467347,-0.563010483519844));
#31785=DIRECTION('center_axis',(0.,-1.,0.));
#31786=DIRECTION('ref_axis',(6.12323399573677E-17,0.,-1.));
#31787=DIRECTION('',(-0.43401111848607,0.707106781186588,-0.558242195673539));
#31788=DIRECTION('',(-0.43401111848607,-0.707106781186588,0.558242195673539));
#31789=DIRECTION('center_axis',(0.,1.,0.));
#31790=DIRECTION('ref_axis',(6.12323399573677E-17,0.,1.));
#31791=DIRECTION('',(-0.315789473684196,-0.707106781186531,0.632674488430095));
#31792=DIRECTION('center_axis',(0.,-1.,0.));
#31793=DIRECTION('ref_axis',(1.,0.,0.));
#31794=DIRECTION('center_axis',(0.,-1.,0.));
#31795=DIRECTION('ref_axis',(1.,0.,0.));
#31796=DIRECTION('',(-0.315789473684196,0.707106781186531,-0.632674488430095));
#31797=DIRECTION('',(0.238798209365762,0.687106448937471,-0.686192497067875));
#31798=DIRECTION('',(0.238798209365737,-0.687106448937475,0.686192497067879));
#31799=DIRECTION('center_axis',(0.,-1.,0.));
#31800=DIRECTION('ref_axis',(1.,0.,0.));
#31801=DIRECTION('',(0.,-1.,0.));
#31802=DIRECTION('center_axis',(0.,1.,0.));
#31803=DIRECTION('ref_axis',(1.,0.,0.));
#31804=DIRECTION('center_axis',(0.,1.,0.));
#31805=DIRECTION('ref_axis',(1.,0.,0.));
#31806=DIRECTION('',(-0.373458905374388,0.737256835467258,0.563010483519951));
#31807=DIRECTION('',(0.373458905374438,0.737256835467322,0.563010483519834));
#31808=DIRECTION('center_axis',(0.,-1.,0.));
#31809=DIRECTION('ref_axis',(-1.83697019872103E-16,0.,1.));
#31810=DIRECTION('',(0.43401111848607,0.707106781186588,0.558242195673539));
#31811=DIRECTION('',(0.43401111848607,-0.707106781186588,-0.558242195673539));
#31812=DIRECTION('center_axis',(0.,0.,-1.));
#31813=DIRECTION('ref_axis',(1.,0.,0.));
#31814=DIRECTION('center_axis',(0.,0.,-1.));
#31815=DIRECTION('ref_axis',(1.,0.,0.));
#31816=DIRECTION('',(0.707106781186573,-8.65956056235524E-17,0.707106781186522));
#31817=DIRECTION('center_axis',(0.,0.,1.));
#31818=DIRECTION('ref_axis',(1.,0.,0.));
#31819=DIRECTION('center_axis',(0.,0.,1.));
#31820=DIRECTION('ref_axis',(1.,0.,0.));
#31821=DIRECTION('',(0.,0.,1.));
#31822=DIRECTION('center_axis',(0.,0.,-1.));
#31823=DIRECTION('ref_axis',(1.,0.,0.));
#31824=DIRECTION('center_axis',(0.,0.,1.));
#31825=DIRECTION('ref_axis',(1.,0.,0.));
#31826=DIRECTION('center_axis',(0.,0.,-1.));
#31827=DIRECTION('ref_axis',(1.,0.,0.));
#31828=DIRECTION('center_axis',(0.,0.,1.));
#31829=DIRECTION('ref_axis',(1.,0.,0.));
#31830=DIRECTION('center_axis',(0.,0.,1.));
#31831=DIRECTION('ref_axis',(1.,0.,0.));
#31832=DIRECTION('',(0.707106781186573,8.65956056235524E-17,-0.707106781186522));
#31833=DIRECTION('center_axis',(0.,0.,1.));
#31834=DIRECTION('ref_axis',(1.,0.,0.));
#31835=DIRECTION('',(0.,-1.,0.));
#31836=DIRECTION('center_axis',(0.,0.,1.));
#31837=DIRECTION('ref_axis',(1.,0.,0.));
#31838=DIRECTION('center_axis',(0.,0.,-1.));
#31839=DIRECTION('ref_axis',(1.,0.,0.));
#31840=DIRECTION('',(0.707106781186573,-8.65956056235524E-17,0.707106781186522));
#31841=DIRECTION('center_axis',(0.,0.,1.));
#31842=DIRECTION('ref_axis',(1.,0.,0.));
#31843=DIRECTION('center_axis',(0.,0.,1.));
#31844=DIRECTION('ref_axis',(1.,0.,0.));
#31845=DIRECTION('',(0.,0.,1.));
#31846=DIRECTION('center_axis',(0.,0.,-1.));
#31847=DIRECTION('ref_axis',(1.,0.,0.));
#31848=DIRECTION('center_axis',(0.,0.,1.));
#31849=DIRECTION('ref_axis',(1.,0.,0.));
#31850=DIRECTION('',(0.707106781186573,8.65956056235524E-17,-0.707106781186522));
#31851=DIRECTION('',(0.,1.,0.));
#31852=DIRECTION('',(0.,1.,0.));
#31853=DIRECTION('',(0.,1.,0.));
#31854=DIRECTION('',(0.,1.,0.));
#31855=DIRECTION('',(0.,1.,0.));
#31856=DIRECTION('',(0.,1.,0.));
#31857=DIRECTION('',(0.,1.,0.));
#31858=DIRECTION('',(0.,1.,0.));
#31859=DIRECTION('',(0.,1.,0.));
#31860=DIRECTION('',(0.,1.,0.));
#31861=DIRECTION('',(0.,1.,0.));
#31862=DIRECTION('',(0.,1.,0.));
#31863=DIRECTION('',(0.,1.,0.));
#31864=DIRECTION('',(0.,1.,0.));
#31865=DIRECTION('',(0.,1.,0.));
#31866=DIRECTION('',(0.,1.,0.));
#31867=DIRECTION('',(0.,1.,0.));
#31868=DIRECTION('',(0.,1.,0.));
#31869=DIRECTION('center_axis',(5.78607088678386E-16,1.,-3.04931671898278E-16));
#31870=DIRECTION('ref_axis',(1.,-5.78607088678386E-16,0.));
#31871=DIRECTION('center_axis',(0.,0.,-1.));
#31872=DIRECTION('ref_axis',(-1.,7.44994596638861E-32,0.));
#31873=DIRECTION('',(0.,1.,0.));
#31874=DIRECTION('',(-1.,7.44994596638861E-32,0.));
#31875=DIRECTION('',(0.,1.,0.));
#31876=DIRECTION('center_axis',(-1.,0.,0.));
#31877=DIRECTION('ref_axis',(0.,1.22464679914735E-16,1.));
#31878=DIRECTION('',(0.,1.,0.));
#31879=DIRECTION('',(0.,1.22464679914735E-16,1.));
#31880=DIRECTION('center_axis',(0.,0.,-1.));
#31881=DIRECTION('ref_axis',(-1.,-7.59796397489589E-32,0.));
#31882=DIRECTION('',(0.,1.,0.));
#31883=DIRECTION('',(-1.,-7.59796397489589E-32,0.));
#31884=DIRECTION('center_axis',(1.,0.,0.));
#31885=DIRECTION('ref_axis',(0.,-1.22464679914735E-16,-1.));
#31886=DIRECTION('',(0.,1.,0.));
#31887=DIRECTION('',(0.,-1.22464679914735E-16,-1.));
#31888=DIRECTION('center_axis',(0.,0.,-1.));
#31889=DIRECTION('ref_axis',(-1.,1.86248514964948E-32,0.));
#31890=DIRECTION('',(0.,1.,0.));
#31891=DIRECTION('',(-1.,1.86248514964948E-32,0.));
#31892=DIRECTION('center_axis',(1.,0.,0.));
#31893=DIRECTION('ref_axis',(0.,-1.22464679914735E-16,-1.));
#31894=DIRECTION('',(0.,1.,0.));
#31895=DIRECTION('',(0.,-1.22464679914735E-16,-1.));
#31896=DIRECTION('center_axis',(0.,0.,1.));
#31897=DIRECTION('ref_axis',(1.,0.,0.));
#31898=DIRECTION('',(0.,1.,0.));
#31899=DIRECTION('',(1.,0.,0.));
#31900=DIRECTION('center_axis',(-1.,0.,0.));
#31901=DIRECTION('ref_axis',(0.,1.22464679914735E-16,1.));
#31902=DIRECTION('',(0.,1.22464679914735E-16,1.));
#31903=DIRECTION('center_axis',(0.,1.,0.));
#31904=DIRECTION('ref_axis',(0.,0.,1.));
#31905=DIRECTION('',(0.,1.,0.));
#31906=DIRECTION('',(0.,1.,0.));
#31907=DIRECTION('',(0.,1.,0.));
#31908=DIRECTION('',(0.,1.,0.));
#31909=DIRECTION('',(0.,1.,0.));
#31910=DIRECTION('',(0.,1.,0.));
#31911=DIRECTION('',(0.,1.,0.));
#31912=DIRECTION('',(0.,1.,0.));
#31913=DIRECTION('',(0.,1.,0.));
#31914=DIRECTION('',(0.,1.,0.));
#31915=DIRECTION('',(0.,1.,0.));
#31916=DIRECTION('',(0.,1.,0.));
#31917=DIRECTION('',(0.,1.,0.));
#31918=DIRECTION('',(0.,1.,0.));
#31919=DIRECTION('',(0.,1.,0.));
#31920=DIRECTION('',(0.,1.,0.));
#31921=DIRECTION('',(0.,1.,0.));
#31922=DIRECTION('',(0.,1.,0.));
#31923=DIRECTION('',(0.,1.,0.));
#31924=DIRECTION('',(0.,1.,0.));
#31925=DIRECTION('',(0.,1.,0.));
#31926=DIRECTION('',(0.,1.,0.));
#31927=DIRECTION('center_axis',(6.36041226292982E-16,1.,-2.54585982322281E-16));
#31928=DIRECTION('ref_axis',(1.,-6.36041226292982E-16,0.));
#31929=DIRECTION('center_axis',(0.,0.,1.));
#31930=DIRECTION('ref_axis',(1.,0.,0.));
#31931=DIRECTION('',(0.,1.,0.));
#31932=DIRECTION('',(1.,0.,0.));
#31933=DIRECTION('',(0.,1.,0.));
#31934=DIRECTION('',(0.,1.,0.));
#31935=DIRECTION('',(0.,1.,0.));
#31936=DIRECTION('',(0.,1.,0.));
#31937=DIRECTION('',(0.,1.,0.));
#31938=DIRECTION('',(0.,1.,0.));
#31939=DIRECTION('',(0.,1.,0.));
#31940=DIRECTION('',(0.,1.,0.));
#31941=DIRECTION('',(0.,1.,0.));
#31942=DIRECTION('',(0.,1.,0.));
#31943=DIRECTION('',(0.,1.,0.));
#31944=DIRECTION('center_axis',(-0.0806195014135826,0.,-0.996744950321709));
#31945=DIRECTION('ref_axis',(-0.996744950321709,9.87304143549995E-18,0.0806195014135826));
#31946=DIRECTION('',(0.,1.,0.));
#31947=DIRECTION('',(-0.996744950321709,9.87304143549995E-18,0.0806195014135826));
#31948=DIRECTION('',(0.,1.,0.));
#31949=DIRECTION('',(0.,1.,0.));
#31950=DIRECTION('',(0.,1.,0.));
#31951=DIRECTION('',(0.,1.,0.));
#31952=DIRECTION('',(0.,1.,0.));
#31953=DIRECTION('',(0.,1.,0.));
#31954=DIRECTION('',(0.,1.,0.));
#31955=DIRECTION('',(0.,1.,0.));
#31956=DIRECTION('center_axis',(0.,0.,-1.));
#31957=DIRECTION('ref_axis',(-1.,0.,0.));
#31958=DIRECTION('',(0.,1.,0.));
#31959=DIRECTION('',(-1.,0.,0.));
#31960=DIRECTION('center_axis',(1.,0.,0.));
#31961=DIRECTION('ref_axis',(0.,-1.22464679914735E-16,-1.));
#31962=DIRECTION('',(0.,-1.22464679914735E-16,-1.));
#31963=DIRECTION('center_axis',(1.79916134966616E-15,1.,-7.85768930404053E-16));
#31964=DIRECTION('ref_axis',(1.,-1.79916134966616E-15,0.));
#31965=DIRECTION('center_axis',(0.,0.,-1.));
#31966=DIRECTION('ref_axis',(-1.,-8.07952632620863E-32,0.));
#31967=DIRECTION('',(0.,1.,0.));
#31968=DIRECTION('',(-1.,-8.07952632620863E-32,0.));
#31969=DIRECTION('',(0.,1.,0.));
#31970=DIRECTION('center_axis',(1.,0.,0.));
#31971=DIRECTION('ref_axis',(0.,-1.22464679914735E-16,-1.));
#31972=DIRECTION('',(0.,1.,0.));
#31973=DIRECTION('',(0.,-1.22464679914735E-16,-1.));
#31974=DIRECTION('center_axis',(-0.826141857774468,0.,-0.563462182256227));
#31975=DIRECTION('ref_axis',(-0.563462182256227,1.01173198176515E-16,0.826141857774468));
#31976=DIRECTION('',(0.,1.,0.));
#31977=DIRECTION('',(-0.563462182256227,1.01173198176515E-16,0.826141857774468));
#31978=DIRECTION('center_axis',(0.,0.,-1.));
#31979=DIRECTION('ref_axis',(-1.,-4.03029640013317E-32,0.));
#31980=DIRECTION('',(0.,1.,0.));
#31981=DIRECTION('',(-1.,-4.03029640013317E-32,0.));
#31982=DIRECTION('center_axis',(1.,0.,0.));
#31983=DIRECTION('ref_axis',(0.,-1.22464679914735E-16,-1.));
#31984=DIRECTION('',(0.,1.,0.));
#31985=DIRECTION('',(0.,-1.22464679914735E-16,-1.));
#31986=DIRECTION('center_axis',(0.,0.,1.));
#31987=DIRECTION('ref_axis',(1.,0.,0.));
#31988=DIRECTION('',(0.,1.,0.));
#31989=DIRECTION('',(1.,0.,0.));
#31990=DIRECTION('center_axis',(-1.,0.,0.));
#31991=DIRECTION('ref_axis',(0.,1.22464679914735E-16,1.));
#31992=DIRECTION('',(0.,1.,0.));
#31993=DIRECTION('',(0.,1.22464679914735E-16,1.));
#31994=DIRECTION('center_axis',(0.826700178836718,0.,0.562642705730145));
#31995=DIRECTION('ref_axis',(0.562642705730145,-1.01241572786693E-16,-0.826700178836718));
#31996=DIRECTION('',(0.,1.,0.));
#31997=DIRECTION('',(0.562642705730145,-1.01241572786693E-16,-0.826700178836718));
#31998=DIRECTION('center_axis',(0.,0.,1.));
#31999=DIRECTION('ref_axis',(1.,0.,0.));
#32000=DIRECTION('',(0.,1.,0.));
#32001=DIRECTION('',(1.,0.,0.));
#32002=DIRECTION('center_axis',(-1.,0.,0.));
#32003=DIRECTION('ref_axis',(0.,1.22464679914735E-16,1.));
#32004=DIRECTION('',(0.,1.22464679914735E-16,1.));
#32005=DIRECTION('center_axis',(0.,1.,0.));
#32006=DIRECTION('ref_axis',(0.,0.,1.));
#32007=DIRECTION('center_axis',(0.,-1.,0.));
#32008=DIRECTION('ref_axis',(0.,0.,-1.));
#32009=DIRECTION('center_axis',(0.,-1.,0.));
#32010=DIRECTION('ref_axis',(0.,0.,-1.));
#32011=DIRECTION('center_axis',(0.,0.,1.));
#32012=DIRECTION('ref_axis',(1.,0.,0.));
#32013=DIRECTION('',(0.,-1.,0.));
#32014=DIRECTION('center_axis',(-1.,0.,0.));
#32015=DIRECTION('ref_axis',(0.,-1.,0.));
#32016=DIRECTION('',(0.,-1.,0.));
#32017=DIRECTION('center_axis',(0.,0.,-1.));
#32018=DIRECTION('ref_axis',(0.,1.,0.));
#32019=DIRECTION('center_axis',(1.,0.,0.));
#32020=DIRECTION('ref_axis',(0.,-0.707106781186542,0.707106781186553));
#32021=DIRECTION('center_axis',(0.,0.,-1.));
#32022=DIRECTION('ref_axis',(0.,1.,0.));
#32023=DIRECTION('center_axis',(1.,0.,0.));
#32024=DIRECTION('ref_axis',(0.,0.707106781186543,0.707106781186552));
#32025=DIRECTION('axis',(0.,0.,1.));
#32026=DIRECTION('refdir',(1.,0.,0.));
#32027=DIRECTION('center_axis',(-0.707106781186544,-0.707106781186551,0.));
#32028=DIRECTION('ref_axis',(0.,0.,1.));
#32029=DIRECTION('',(0.,0.,1.));
#32030=DIRECTION('',(0.577350269189641,-0.577350269189636,-0.5773502691896));
#32031=DIRECTION('',(0.,0.,-1.));
#32032=DIRECTION('',(0.577350269189641,-0.577350269189636,0.5773502691896));
#32033=DIRECTION('center_axis',(-0.707106781186522,0.,0.707106781186573));
#32034=DIRECTION('ref_axis',(0.707106781186573,0.,0.707106781186522));
#32035=DIRECTION('',(0.,-1.,0.));
#32036=DIRECTION('',(0.577350269189643,-0.577350269189633,0.577350269189602));
#32037=DIRECTION('',(0.577350269189643,0.577350269189633,0.577350269189602));
#32038=DIRECTION('',(0.,1.,0.));
#32039=DIRECTION('center_axis',(0.,-1.,0.));
#32040=DIRECTION('ref_axis',(0.,0.,-1.));
#32041=DIRECTION('',(1.,0.,0.));
#32042=DIRECTION('',(0.,0.,-1.));
#32043=DIRECTION('',(1.,0.,0.));
#32044=DIRECTION('center_axis',(0.,0.,1.));
#32045=DIRECTION('ref_axis',(0.,-1.,0.));
#32046=DIRECTION('',(-1.,0.,0.));
#32047=DIRECTION('',(0.,-1.,0.));
#32048=DIRECTION('center_axis',(0.,-0.707106781186529,0.707106781186566));
#32049=DIRECTION('ref_axis',(1.,0.,0.));
#32050=DIRECTION('',(0.577350269189643,-0.577350269189633,-0.577350269189602));
#32051=DIRECTION('',(1.,0.,0.));
#32052=DIRECTION('',(0.577350269189616,0.577350269189646,0.577350269189616));
#32053=DIRECTION('',(0.577350269189616,-0.577350269189646,-0.577350269189616));
#32054=DIRECTION('center_axis',(-0.707106781186548,0.,0.707106781186548));
#32055=DIRECTION('ref_axis',(0.707106781186548,0.,0.707106781186548));
#32056=DIRECTION('',(0.,1.,0.));
#32057=DIRECTION('',(-0.577350269189616,0.577350269189646,-0.577350269189616));
#32058=DIRECTION('',(-0.577350269189616,-0.577350269189646,-0.577350269189616));
#32059=DIRECTION('',(0.,-1.,0.));
#32060=DIRECTION('',(0.577350269189616,0.577350269189646,0.577350269189616));
#32061=DIRECTION('center_axis',(-0.707106781186566,0.707106781186529,0.));
#32062=DIRECTION('ref_axis',(0.,0.,1.));
#32063=DIRECTION('',(0.,0.,-1.));
#32064=DIRECTION('',(0.,0.,1.));
#32065=DIRECTION('',(0.577350269189616,0.577350269189646,-0.577350269189616));
#32066=DIRECTION('center_axis',(-0.707106781186548,0.,-0.707106781186548));
#32067=DIRECTION('ref_axis',(-0.707106781186548,0.,0.707106781186548));
#32068=DIRECTION('',(0.,1.,0.));
#32069=DIRECTION('',(0.577350269189616,0.577350269189646,-0.577350269189616));
#32070=DIRECTION('',(0.577350269189616,-0.577350269189646,-0.577350269189616));
#32071=DIRECTION('',(0.,-1.,0.));
#32072=DIRECTION('center_axis',(0.,0.707106781186529,0.707106781186566));
#32073=DIRECTION('ref_axis',(1.,0.,0.));
#32074=DIRECTION('',(1.,0.,0.));
#32075=DIRECTION('',(0.577350269189616,0.577350269189646,-0.577350269189616));
#32076=DIRECTION('',(-0.577350269189616,0.577350269189646,-0.577350269189616));
#32077=DIRECTION('',(-1.,0.,0.));
#32078=DIRECTION('',(-0.577350269189616,-0.577350269189646,0.577350269189616));
#32079=DIRECTION('center_axis',(0.,0.,1.));
#32080=DIRECTION('ref_axis',(0.,-1.,0.));
#32081=DIRECTION('',(1.,0.,0.));
#32082=DIRECTION('',(0.,-1.,0.));
#32083=DIRECTION('center_axis',(0.,1.,0.));
#32084=DIRECTION('ref_axis',(0.,0.,1.));
#32085=DIRECTION('',(1.,0.,0.));
#32086=DIRECTION('',(0.,0.,1.));
#32087=DIRECTION('center_axis',(0.,0.,-1.));
#32088=DIRECTION('ref_axis',(0.,1.,0.));
#32089=DIRECTION('',(-1.,0.,0.));
#32090=DIRECTION('',(0.,1.,0.));
#32091=DIRECTION('center_axis',(0.,0.707106781186529,-0.707106781186566));
#32092=DIRECTION('ref_axis',(-1.,0.,0.));
#32093=DIRECTION('',(0.577350269189616,0.577350269189646,0.577350269189616));
#32094=DIRECTION('',(1.,0.,0.));
#32095=DIRECTION('',(0.577350269189616,-0.577350269189646,-0.577350269189616));
#32096=DIRECTION('',(0.577350269189616,0.577350269189646,0.577350269189616));
#32097=DIRECTION('center_axis',(-0.707106781186522,0.,0.707106781186573));
#32098=DIRECTION('ref_axis',(0.707106781186573,0.,0.707106781186522));
#32099=DIRECTION('',(0.577350269189643,0.577350269189633,0.577350269189602));
#32100=DIRECTION('',(0.,1.,0.));
#32101=DIRECTION('',(-0.577350269189643,0.577350269189633,-0.577350269189602));
#32102=DIRECTION('',(-0.577350269189643,-0.577350269189633,-0.577350269189602));
#32103=DIRECTION('',(0.,-1.,0.));
#32104=DIRECTION('',(0.577350269189643,-0.577350269189633,0.577350269189602));
#32105=DIRECTION('center_axis',(0.,-0.707106781186529,0.707106781186566));
#32106=DIRECTION('ref_axis',(1.,0.,0.));
#32107=DIRECTION('',(0.577350269189643,-0.577350269189633,-0.577350269189602));
#32108=DIRECTION('',(1.,0.,0.));
#32109=DIRECTION('',(-0.577350269189616,0.577350269189646,0.577350269189616));
#32110=DIRECTION('',(-1.,0.,0.));
#32111=DIRECTION('center_axis',(-0.707106781186541,-0.707106781186554,0.));
#32112=DIRECTION('ref_axis',(0.,0.,1.));
#32113=DIRECTION('',(0.,0.,-1.));
#32114=DIRECTION('',(-0.577350269189643,0.577350269189633,0.577350269189602));
#32115=DIRECTION('',(-0.577350269189643,0.577350269189633,-0.577350269189602));
#32116=DIRECTION('',(0.,0.,1.));
#32117=DIRECTION('center_axis',(1.,0.,0.));
#32118=DIRECTION('ref_axis',(0.,0.,-1.));
#32119=DIRECTION('',(0.,1.,0.));
#32120=DIRECTION('',(0.,0.,1.));
#32121=DIRECTION('',(0.,1.,0.));
#32122=DIRECTION('',(0.,0.,-1.));
#32123=DIRECTION('center_axis',(0.,-0.707106781186529,0.707106781186566));
#32124=DIRECTION('ref_axis',(1.,0.,0.));
#32125=DIRECTION('',(1.,0.,0.));
#32126=DIRECTION('',(0.577350269189616,0.577350269189646,0.577350269189616));
#32127=DIRECTION('',(-0.577350269189616,0.577350269189646,0.577350269189616));
#32128=DIRECTION('',(-1.,0.,0.));
#32129=DIRECTION('',(-0.577350269189616,-0.577350269189646,-0.577350269189616));
#32130=DIRECTION('center_axis',(0.707106781186554,-0.707106781186541,0.));
#32131=DIRECTION('ref_axis',(0.,0.,-1.));
#32132=DIRECTION('',(0.,0.,1.));
#32133=DIRECTION('',(-0.577350269189613,-0.577350269189624,0.577350269189641));
#32134=DIRECTION('',(-0.577350269189612,-0.577350269189622,-0.577350269189643));
#32135=DIRECTION('',(0.,0.,-1.));
#32136=DIRECTION('center_axis',(0.,-1.,0.));
#32137=DIRECTION('ref_axis',(0.,0.,-1.));
#32138=DIRECTION('',(1.,0.,0.));
#32139=DIRECTION('',(0.,0.,1.));
#32140=DIRECTION('',(-1.,0.,0.));
#32141=DIRECTION('',(0.,0.,-1.));
#32142=DIRECTION('center_axis',(0.,-0.70710678118656,0.707106781186535));
#32143=DIRECTION('ref_axis',(1.,0.,0.));
#32144=DIRECTION('',(0.577350269189605,-0.577350269189626,-0.577350269189646));
#32145=DIRECTION('',(-1.,0.,0.));
#32146=DIRECTION('',(-0.577350269189614,-0.577350269189621,-0.577350269189642));
#32147=DIRECTION('',(-0.577350269189612,0.577350269189622,0.577350269189643));
#32148=DIRECTION('center_axis',(0.707106781186564,0.,0.707106781186531));
#32149=DIRECTION('ref_axis',(0.707106781186531,0.,-0.707106781186564));
#32150=DIRECTION('',(0.,1.,0.));
#32151=DIRECTION('',(0.577350269189613,-0.577350269189624,-0.577350269189641));
#32152=DIRECTION('',(0.577350269189614,0.577350269189621,-0.577350269189642));
#32153=DIRECTION('',(0.,-1.,0.));
#32154=DIRECTION('center_axis',(-0.707106781186522,0.,-0.707106781186573));
#32155=DIRECTION('ref_axis',(-0.707106781186573,0.,0.707106781186522));
#32156=DIRECTION('',(0.,-1.,0.));
#32157=DIRECTION('',(-0.577350269189643,-0.577350269189633,0.577350269189602));
#32158=DIRECTION('center_axis',(0.,-0.707106781186529,-0.707106781186566));
#32159=DIRECTION('ref_axis',(-1.,0.,0.));
#32160=DIRECTION('',(1.,0.,0.));
#32161=DIRECTION('',(0.577350269189616,-0.577350269189646,0.577350269189616));
#32162=DIRECTION('',(-0.577350269189616,-0.577350269189646,0.577350269189616));
#32163=DIRECTION('center_axis',(0.707106781186566,-0.707106781186529,0.));
#32164=DIRECTION('ref_axis',(0.,0.,-1.));
#32165=DIRECTION('',(-0.577350269189616,-0.577350269189646,-0.577350269189616));
#32166=DIRECTION('',(0.,0.,1.));
#32167=DIRECTION('',(0.577350269189616,0.577350269189646,-0.577350269189616));
#32168=DIRECTION('center_axis',(0.707106781186548,0.,-0.707106781186548));
#32169=DIRECTION('ref_axis',(-0.707106781186548,0.,-0.707106781186548));
#32170=DIRECTION('',(0.,1.,0.));
#32171=DIRECTION('',(-0.577350269189616,-0.577350269189646,-0.577350269189616));
#32172=DIRECTION('',(0.,-1.,0.));
#32173=DIRECTION('center_axis',(-0.707106781186566,0.707106781186529,0.));
#32174=DIRECTION('ref_axis',(0.,0.,1.));
#32175=DIRECTION('',(0.,0.,-1.));
#32176=DIRECTION('',(0.577350269189616,0.577350269189646,0.577350269189616));
#32177=DIRECTION('',(0.577350269189616,0.577350269189646,-0.577350269189616));
#32178=DIRECTION('',(0.,0.,1.));
#32179=DIRECTION('center_axis',(0.,1.,0.));
#32180=DIRECTION('ref_axis',(0.,0.,1.));
#32181=DIRECTION('',(0.,0.,1.));
#32182=DIRECTION('',(1.,0.,0.));
#32183=DIRECTION('',(0.,0.,1.));
#32184=DIRECTION('',(1.,0.,0.));
#32185=DIRECTION('',(0.,0.,-1.));
#32186=DIRECTION('',(1.,0.,0.));
#32187=DIRECTION('center_axis',(0.,0.707106781186529,-0.707106781186566));
#32188=DIRECTION('ref_axis',(-1.,0.,0.));
#32189=DIRECTION('',(0.577350269189643,0.577350269189633,0.577350269189602));
#32190=DIRECTION('',(-1.,0.,0.));
#32191=DIRECTION('',(-0.577350269189616,0.577350269189646,0.577350269189616));
#32192=DIRECTION('center_axis',(-0.707106781186548,0.,-0.707106781186548));
#32193=DIRECTION('ref_axis',(-0.707106781186548,0.,0.707106781186548));
#32194=DIRECTION('',(0.,-1.,0.));
#32195=DIRECTION('',(-0.707106781186548,0.,0.707106781186548));
#32196=DIRECTION('',(0.,1.,0.));
#32197=DIRECTION('center_axis',(-0.707106781186554,-0.707106781186541,0.));
#32198=DIRECTION('ref_axis',(0.,0.,1.));
#32199=DIRECTION('',(-0.577350269189613,0.577350269189624,-0.577350269189641));
#32200=DIRECTION('',(0.,0.,-1.));
#32201=DIRECTION('center_axis',(0.,0.,1.));
#32202=DIRECTION('ref_axis',(0.,-1.,0.));
#32203=DIRECTION('',(0.,1.,0.));
#32204=DIRECTION('',(1.,0.,0.));
#32205=DIRECTION('center_axis',(-1.,0.,0.));
#32206=DIRECTION('ref_axis',(0.,-1.,0.));
#32207=DIRECTION('',(0.,-1.,0.));
#32208=DIRECTION('',(0.,0.,1.));
#32209=DIRECTION('',(0.,1.,0.));
#32210=DIRECTION('',(0.,-0.707106781186566,-0.707106781186529));
#32211=DIRECTION('',(0.,0.,-1.));
#32212=DIRECTION('',(0.,1.,0.));
#32213=DIRECTION('',(0.,0.,-1.));
#32214=DIRECTION('',(0.,-0.707106781186566,0.707106781186529));
#32215=DIRECTION('center_axis',(-0.707106781186564,0.,0.707106781186531));
#32216=DIRECTION('ref_axis',(0.707106781186531,0.,0.707106781186564));
#32217=DIRECTION('',(0.,1.,0.));
#32218=DIRECTION('',(-0.577350269189614,0.577350269189621,-0.577350269189642));
#32219=DIRECTION('',(0.57735026918962,0.57735026918961,0.577350269189647));
#32220=DIRECTION('center_axis',(-0.577350269189636,-0.577350269189605,-0.577350269189636));
#32221=DIRECTION('ref_axis',(-0.707106781186548,0.,0.707106781186548));
#32222=DIRECTION('',(0.,0.707106781186566,-0.707106781186529));
#32223=DIRECTION('',(0.707106781186529,-0.707106781186566,0.));
#32224=DIRECTION('center_axis',(-0.707106781186566,-0.707106781186529,0.));
#32225=DIRECTION('ref_axis',(0.,0.,1.));
#32226=DIRECTION('',(-0.577350269189616,0.577350269189646,-0.577350269189616));
#32227=DIRECTION('',(0.,0.,-1.));
#32228=DIRECTION('',(0.,0.,1.));
#32229=DIRECTION('',(-0.577350269189616,0.577350269189646,0.577350269189616));
#32230=DIRECTION('center_axis',(0.,-0.707106781186529,-0.707106781186566));
#32231=DIRECTION('ref_axis',(-1.,0.,0.));
#32232=DIRECTION('',(0.,0.707106781186566,-0.707106781186529));
#32233=DIRECTION('',(-1.,0.,0.));
#32234=DIRECTION('',(1.,0.,0.));
#32235=DIRECTION('center_axis',(1.,0.,0.));
#32236=DIRECTION('ref_axis',(0.,0.,-1.));
#32237=DIRECTION('',(0.,-1.,0.));
#32238=DIRECTION('',(0.,0.,1.));
#32239=DIRECTION('center_axis',(-0.707106781186548,0.,0.707106781186548));
#32240=DIRECTION('ref_axis',(0.707106781186548,0.,0.707106781186548));
#32241=DIRECTION('',(0.577350269189616,0.577350269189646,0.577350269189616));
#32242=DIRECTION('',(0.,1.,0.));
#32243=DIRECTION('',(0.577350269189616,-0.577350269189646,0.577350269189616));
#32244=DIRECTION('',(-0.577350269189616,-0.577350269189646,-0.577350269189616));
#32245=DIRECTION('center_axis',(0.,-0.707106781186529,0.707106781186566));
#32246=DIRECTION('ref_axis',(1.,0.,0.));
#32247=DIRECTION('',(1.,0.,0.));
#32248=DIRECTION('',(-1.,0.,0.));
#32249=DIRECTION('center_axis',(0.,-1.,0.));
#32250=DIRECTION('ref_axis',(0.,0.,-1.));
#32251=DIRECTION('',(0.,0.,-1.));
#32252=DIRECTION('',(0.707106781186573,0.,0.707106781186522));
#32253=DIRECTION('',(1.,0.,0.));
#32254=DIRECTION('',(0.707106781186573,0.,-0.707106781186522));
#32255=DIRECTION('',(0.,0.,-1.));
#32256=DIRECTION('',(-1.,0.,0.));
#32257=DIRECTION('',(0.,0.,-1.));
#32258=DIRECTION('',(1.,0.,0.));
#32259=DIRECTION('',(0.,0.,1.));
#32260=DIRECTION('',(-0.707106781186573,0.,-0.707106781186522));
#32261=DIRECTION('',(1.,0.,0.));
#32262=DIRECTION('',(-0.707106781186573,0.,0.707106781186522));
#32263=DIRECTION('center_axis',(0.,-0.707106781186529,0.707106781186566));
#32264=DIRECTION('ref_axis',(1.,0.,0.));
#32265=DIRECTION('',(-0.577350269189616,0.577350269189646,0.577350269189616));
#32266=DIRECTION('',(-1.,0.,0.));
#32267=DIRECTION('',(0.,0.707106781186566,0.707106781186529));
#32268=DIRECTION('',(0.577350269189616,0.577350269189646,0.577350269189616));
#32269=DIRECTION('center_axis',(0.707106781186548,0.,0.707106781186548));
#32270=DIRECTION('ref_axis',(0.707106781186548,0.,-0.707106781186548));
#32271=DIRECTION('',(-0.577350269189616,-0.577350269189646,0.577350269189616));
#32272=DIRECTION('',(0.,1.,0.));
#32273=DIRECTION('',(-0.577350269189616,0.577350269189646,0.577350269189616));
#32274=DIRECTION('',(-0.577350269189616,-0.577350269189646,0.577350269189616));
#32275=DIRECTION('',(0.,-1.,0.));
#32276=DIRECTION('center_axis',(0.707106781186566,-0.707106781186529,0.));
#32277=DIRECTION('ref_axis',(0.,0.,-1.));
#32278=DIRECTION('',(-0.577350269189616,-0.577350269189646,0.577350269189616));
#32279=DIRECTION('',(-0.577350269189616,-0.577350269189646,-0.577350269189616));
#32280=DIRECTION('',(0.,0.,1.));
#32281=DIRECTION('center_axis',(0.,0.707106781186529,-0.707106781186566));
#32282=DIRECTION('ref_axis',(-1.,0.,0.));
#32283=DIRECTION('',(0.577350269189616,-0.577350269189646,-0.577350269189616));
#32284=DIRECTION('',(-0.577350269189616,-0.577350269189646,-0.577350269189616));
#32285=DIRECTION('',(-1.,0.,0.));
#32286=DIRECTION('',(-0.577350269189616,0.577350269189646,0.577350269189616));
#32287=DIRECTION('center_axis',(0.707106781186554,0.707106781186541,0.));
#32288=DIRECTION('ref_axis',(0.,0.,-1.));
#32289=DIRECTION('',(0.,0.,-1.));
#32290=DIRECTION('',(-0.577350269189613,0.577350269189624,-0.577350269189641));
#32291=DIRECTION('',(-0.577350269189612,0.577350269189622,0.577350269189643));
#32292=DIRECTION('center_axis',(0.707106781186566,0.707106781186529,0.));
#32293=DIRECTION('ref_axis',(0.,0.,-1.));
#32294=DIRECTION('',(-0.577350269189616,0.577350269189646,0.577350269189616));
#32295=DIRECTION('',(0.,0.,-1.));
#32296=DIRECTION('',(0.577350269189616,-0.577350269189646,0.577350269189616));
#32297=DIRECTION('center_axis',(0.,0.70710678118656,-0.707106781186535));
#32298=DIRECTION('ref_axis',(-1.,0.,0.));
#32299=DIRECTION('',(0.577350269189605,0.577350269189626,0.577350269189646));
#32300=DIRECTION('',(-1.,0.,0.));
#32301=DIRECTION('',(0.577350269189614,-0.577350269189621,-0.577350269189642));
#32302=DIRECTION('',(-0.577350269189626,-0.577350269189615,-0.577350269189636));
#32303=DIRECTION('center_axis',(0.707106781186522,0.,0.707106781186573));
#32304=DIRECTION('ref_axis',(0.707106781186573,0.,-0.707106781186522));
#32305=DIRECTION('',(-0.707106781186573,0.,0.707106781186522));
#32306=DIRECTION('',(0.,1.,0.));
#32307=DIRECTION('',(0.,-1.,0.));
#32308=DIRECTION('center_axis',(1.,0.,0.));
#32309=DIRECTION('ref_axis',(0.,1.,0.));
#32310=DIRECTION('',(0.,1.,0.));
#32311=DIRECTION('',(0.,-0.707106781186566,0.707106781186529));
#32312=DIRECTION('',(0.,0.,1.));
#32313=DIRECTION('',(0.,-0.707106781186566,-0.707106781186529));
#32314=DIRECTION('',(0.,1.,0.));
#32315=DIRECTION('',(0.,0.,1.));
#32316=DIRECTION('',(0.,-1.,0.));
#32317=DIRECTION('center_axis',(0.,-0.707106781186529,-0.707106781186566));
#32318=DIRECTION('ref_axis',(-1.,0.,0.));
#32319=DIRECTION('',(1.,0.,0.));
#32320=DIRECTION('',(0.577350269189616,-0.577350269189646,0.577350269189616));
#32321=DIRECTION('center_axis',(0.707106781186548,0.,-0.707106781186548));
#32322=DIRECTION('ref_axis',(-0.707106781186548,0.,-0.707106781186548));
#32323=DIRECTION('',(0.,-1.,0.));
#32324=DIRECTION('',(0.,1.,0.));
#32325=DIRECTION('center_axis',(0.707106781186548,0.,-0.707106781186548));
#32326=DIRECTION('ref_axis',(-0.707106781186548,0.,-0.707106781186548));
#32327=DIRECTION('',(0.577350269189616,-0.577350269189646,0.577350269189616));
#32328=DIRECTION('',(0.,-1.,0.));
#32329=DIRECTION('',(-0.577350269189616,0.577350269189646,-0.577350269189616));
#32330=DIRECTION('center_axis',(0.707106781186566,0.707106781186529,0.));
#32331=DIRECTION('ref_axis',(0.,0.,-1.));
#32332=DIRECTION('',(0.,0.,-1.));
#32333=DIRECTION('',(-0.577350269189616,0.577350269189646,0.577350269189616));
#32334=DIRECTION('center_axis',(0.707106781186548,0.,0.707106781186548));
#32335=DIRECTION('ref_axis',(0.707106781186548,0.,-0.707106781186548));
#32336=DIRECTION('',(0.,1.,0.));
#32337=DIRECTION('center_axis',(1.,0.,0.));
#32338=DIRECTION('ref_axis',(0.,0.,-1.));
#32339=DIRECTION('',(0.,0.,-1.));
#32340=DIRECTION('center_axis',(0.707106781186566,0.707106781186529,0.));
#32341=DIRECTION('ref_axis',(0.,0.,-1.));
#32342=DIRECTION('',(0.,0.,1.));
#32343=DIRECTION('',(-0.577350269189616,0.577350269189646,-0.577350269189616));
#32344=DIRECTION('center_axis',(0.,0.,-1.));
#32345=DIRECTION('ref_axis',(0.,1.,0.));
#32346=DIRECTION('center_axis',(0.,0.,1.));
#32347=DIRECTION('ref_axis',(0.,-1.,0.));
#32348=DIRECTION('',(1.,0.,0.));
#32349=DIRECTION('',(0.,-1.,0.));
#32350=DIRECTION('center_axis',(0.,0.707106781186529,0.707106781186566));
#32351=DIRECTION('ref_axis',(1.,0.,0.));
#32352=DIRECTION('',(-1.,0.,0.));
#32353=DIRECTION('',(0.577350269189616,-0.577350269189646,0.577350269189616));
#32354=DIRECTION('center_axis',(0.,1.,0.));
#32355=DIRECTION('ref_axis',(0.,0.,1.));
#32356=DIRECTION('',(0.,0.,-1.));
#32357=DIRECTION('',(-1.,0.,0.));
#32358=DIRECTION('',(0.,0.,-1.));
#32359=DIRECTION('',(-1.,0.,0.));
#32360=DIRECTION('',(0.,0.,1.));
#32361=DIRECTION('center_axis',(0.707106781186554,0.707106781186541,0.));
#32362=DIRECTION('ref_axis',(0.,0.,-1.));
#32363=DIRECTION('',(0.577350269189612,-0.577350269189622,0.577350269189643));
#32364=DIRECTION('',(0.,0.,-1.));
#32365=DIRECTION('center_axis',(0.,0.70710678118656,0.707106781186535));
#32366=DIRECTION('ref_axis',(1.,0.,0.));
#32367=DIRECTION('',(0.577350269189626,0.577350269189615,-0.577350269189636));
#32368=DIRECTION('',(1.,0.,0.));
#32369=DIRECTION('center_axis',(-0.707106781186541,0.707106781186554,0.));
#32370=DIRECTION('ref_axis',(0.,0.,1.));
#32371=DIRECTION('',(-0.577350269189629,-0.577350269189639,0.577350269189609));
#32372=DIRECTION('center_axis',(0.,0.707106781186529,0.707106781186566));
#32373=DIRECTION('ref_axis',(1.,0.,0.));
#32374=DIRECTION('',(-0.577350269189616,-0.577350269189646,0.577350269189616));
#32375=DIRECTION('',(1.,0.,0.));
#32376=DIRECTION('center_axis',(0.,0.,1.));
#32377=DIRECTION('ref_axis',(0.,-1.,0.));
#32378=DIRECTION('center_axis',(-0.707106781186541,0.707106781186554,0.));
#32379=DIRECTION('ref_axis',(0.,0.,1.));
#32380=DIRECTION('',(-0.57735026918962,-0.57735026918961,0.577350269189647));
#32381=DIRECTION('',(0.,0.,1.));
#32382=DIRECTION('center_axis',(-0.707106781186522,0.,0.707106781186573));
#32383=DIRECTION('ref_axis',(0.707106781186573,0.,0.707106781186522));
#32384=DIRECTION('',(0.,-1.,0.));
#32385=DIRECTION('',(-0.707106781186573,0.,-0.707106781186522));
#32386=DIRECTION('',(0.,1.,0.));
#32387=DIRECTION('center_axis',(-1.,0.,0.));
#32388=DIRECTION('ref_axis',(0.,-1.,0.));
#32389=DIRECTION('',(0.,1.,0.));
#32390=DIRECTION('',(0.,0.,-1.));
#32391=DIRECTION('',(0.,-1.,0.));
#32392=DIRECTION('',(0.,0.707106781186566,0.707106781186529));
#32393=DIRECTION('',(0.,0.,-1.));
#32394=DIRECTION('',(0.,-1.,0.));
#32395=DIRECTION('center_axis',(0.707106781186522,0.,-0.707106781186573));
#32396=DIRECTION('ref_axis',(-0.707106781186573,0.,-0.707106781186522));
#32397=DIRECTION('',(0.,-1.,0.));
#32398=DIRECTION('',(0.707106781186573,0.,0.707106781186522));
#32399=DIRECTION('',(0.,1.,0.));
#32400=DIRECTION('center_axis',(0.,0.,1.));
#32401=DIRECTION('ref_axis',(1.,0.,0.));
#32402=DIRECTION('',(1.,0.,0.));
#32403=DIRECTION('',(0.,-1.,0.));
#32404=DIRECTION('center_axis',(0.,0.,-1.));
#32405=DIRECTION('ref_axis',(1.,0.,0.));
#32406=DIRECTION('center_axis',(0.,0.,-1.));
#32407=DIRECTION('ref_axis',(1.,0.,0.));
#32408=DIRECTION('center_axis',(0.,0.707106781186529,0.707106781186566));
#32409=DIRECTION('ref_axis',(1.,0.,0.));
#32410=DIRECTION('',(-0.577350269189616,0.577350269189646,-0.577350269189616));
#32411=DIRECTION('',(-1.,0.,0.));
#32412=DIRECTION('',(0.,0.707106781186566,-0.707106781186529));
#32413=DIRECTION('',(1.,0.,0.));
#32414=DIRECTION('',(0.577350269189616,0.577350269189646,-0.577350269189616));
#32415=DIRECTION('center_axis',(0.,1.,0.));
#32416=DIRECTION('ref_axis',(0.,0.,1.));
#32417=DIRECTION('',(0.,0.,1.));
#32418=DIRECTION('',(0.,0.,1.));
#32419=DIRECTION('',(1.,0.,0.));
#32420=DIRECTION('',(1.,0.,0.));
#32421=DIRECTION('',(1.,0.,0.));
#32422=DIRECTION('',(0.,0.,-1.));
#32423=DIRECTION('',(-1.,0.,0.));
#32424=DIRECTION('',(0.707106781186573,0.,-0.707106781186522));
#32425=DIRECTION('center_axis',(0.707106781186566,0.707106781186529,0.));
#32426=DIRECTION('ref_axis',(0.,0.,-1.));
#32427=DIRECTION('',(-0.577350269189616,0.577350269189646,0.577350269189616));
#32428=DIRECTION('',(0.,0.,-1.));
#32429=DIRECTION('',(-0.707106781186529,0.707106781186566,0.));
#32430=DIRECTION('center_axis',(0.707106781186548,0.,0.707106781186548));
#32431=DIRECTION('ref_axis',(0.707106781186548,0.,-0.707106781186548));
#32432=DIRECTION('',(0.,1.,0.));
#32433=DIRECTION('',(0.,-1.,0.));
#32434=DIRECTION('center_axis',(-0.707106781186566,0.707106781186529,0.));
#32435=DIRECTION('ref_axis',(0.,0.,1.));
#32436=DIRECTION('center_axis',(-0.707106781186522,0.,-0.707106781186573));
#32437=DIRECTION('ref_axis',(-0.707106781186573,0.,0.707106781186522));
#32438=DIRECTION('center_axis',(-0.707106781186541,0.707106781186554,0.));
#32439=DIRECTION('ref_axis',(0.,0.,1.));
#32440=DIRECTION('',(0.577350269189643,0.577350269189633,-0.577350269189602));
#32441=DIRECTION('',(-0.577350269189643,-0.577350269189633,-0.577350269189602));
#32442=DIRECTION('',(-0.577350269189643,-0.577350269189633,0.577350269189602));
#32443=DIRECTION('center_axis',(0.,0.707106781186529,0.707106781186566));
#32444=DIRECTION('ref_axis',(1.,0.,0.));
#32445=DIRECTION('center_axis',(0.,0.707106781186529,-0.707106781186566));
#32446=DIRECTION('ref_axis',(-1.,0.,0.));
#32447=DIRECTION('',(-1.,0.,0.));
#32448=DIRECTION('',(0.577350269189643,-0.577350269189633,-0.577350269189602));
#32449=DIRECTION('center_axis',(0.707106781186548,0.,0.707106781186548));
#32450=DIRECTION('ref_axis',(0.707106781186548,0.,-0.707106781186548));
#32451=DIRECTION('',(0.577350269189616,0.577350269189646,-0.577350269189616));
#32452=DIRECTION('',(0.,1.,0.));
#32453=DIRECTION('',(-0.577350269189616,-0.577350269189646,0.577350269189616));
#32454=DIRECTION('center_axis',(0.707106781186566,-0.707106781186529,0.));
#32455=DIRECTION('ref_axis',(0.,0.,-1.));
#32456=DIRECTION('',(0.,0.,1.));
#32457=DIRECTION('center_axis',(1.,0.,0.));
#32458=DIRECTION('ref_axis',(0.,0.,-1.));
#32459=DIRECTION('',(0.,0.,1.));
#32460=DIRECTION('',(0.,-1.,0.));
#32461=DIRECTION('center_axis',(0.707106781186566,-0.707106781186529,0.));
#32462=DIRECTION('ref_axis',(0.,0.,-1.));
#32463=DIRECTION('',(0.,0.,-1.));
#32464=DIRECTION('',(-0.577350269189616,-0.577350269189646,0.577350269189616));
#32465=DIRECTION('',(-0.577350269189616,-0.577350269189646,-0.577350269189616));
#32466=DIRECTION('center_axis',(0.577350269189636,0.577350269189605,-0.577350269189636));
#32467=DIRECTION('ref_axis',(-0.707106781186548,0.,-0.707106781186548));
#32468=DIRECTION('',(0.707106781186548,0.,0.707106781186548));
#32469=DIRECTION('',(0.,-0.707106781186566,-0.707106781186529));
#32470=DIRECTION('center_axis',(0.,0.707106781186529,-0.707106781186566));
#32471=DIRECTION('ref_axis',(-1.,0.,0.));
#32472=DIRECTION('',(-1.,0.,0.));
#32473=DIRECTION('center_axis',(0.707106781186548,0.,-0.707106781186548));
#32474=DIRECTION('ref_axis',(-0.707106781186548,0.,-0.707106781186548));
#32475=DIRECTION('',(-0.577350269189616,0.577350269189646,-0.577350269189616));
#32476=DIRECTION('',(0.,1.,0.));
#32477=DIRECTION('center_axis',(0.,0.,-1.));
#32478=DIRECTION('ref_axis',(0.,1.,0.));
#32479=DIRECTION('',(1.,0.,0.));
#32480=DIRECTION('center_axis',(0.,-0.707106781186529,-0.707106781186566));
#32481=DIRECTION('ref_axis',(-1.,0.,0.));
#32482=DIRECTION('',(-1.,0.,0.));
#32483=DIRECTION('',(0.577350269189616,0.577350269189646,-0.577350269189616));
#32484=DIRECTION('center_axis',(-0.707106781186522,0.,-0.707106781186573));
#32485=DIRECTION('ref_axis',(-0.707106781186573,0.,0.707106781186522));
#32486=DIRECTION('',(0.,-1.,0.));
#32487=DIRECTION('',(-0.577350269189643,-0.577350269189633,0.577350269189602));
#32488=DIRECTION('',(-0.577350269189643,0.577350269189633,0.577350269189602));
#32489=DIRECTION('center_axis',(0.,-0.707106781186529,-0.707106781186566));
#32490=DIRECTION('ref_axis',(-1.,0.,0.));
#32491=DIRECTION('',(1.,0.,0.));
#32492=DIRECTION('',(-0.577350269189616,0.577350269189646,-0.577350269189616));
#32493=DIRECTION('',(-1.,0.,0.));
#32494=DIRECTION('',(-0.577350269189643,0.577350269189633,-0.577350269189602));
#32495=DIRECTION('center_axis',(0.,0.,-1.));
#32496=DIRECTION('ref_axis',(0.,1.,0.));
#32497=DIRECTION('center_axis',(0.,-1.,0.));
#32498=DIRECTION('ref_axis',(0.,0.,-1.));
#32499=DIRECTION('',(0.,0.,1.));
#32500=DIRECTION('',(0.,0.,1.));
#32501=DIRECTION('',(-1.,0.,0.));
#32502=DIRECTION('',(0.,0.,-1.));
#32503=DIRECTION('center_axis',(0.707106781186554,-0.707106781186541,0.));
#32504=DIRECTION('ref_axis',(0.,0.,-1.));
#32505=DIRECTION('',(0.577350269189612,0.577350269189622,-0.577350269189643));
#32506=DIRECTION('',(0.577350269189613,0.577350269189624,0.577350269189641));
#32507=DIRECTION('center_axis',(0.707106781186564,0.,-0.707106781186531));
#32508=DIRECTION('ref_axis',(-0.707106781186531,0.,-0.707106781186564));
#32509=DIRECTION('',(0.577350269189614,-0.577350269189621,0.577350269189642));
#32510=DIRECTION('',(0.,1.,0.));
#32511=DIRECTION('center_axis',(0.,-0.70710678118656,-0.707106781186535));
#32512=DIRECTION('ref_axis',(-1.,0.,0.));
#32513=DIRECTION('',(0.577350269189612,-0.577350269189622,0.577350269189643));
#32514=DIRECTION('',(-0.577350269189614,-0.577350269189621,0.577350269189642));
#32515=DIRECTION('',(1.,0.,0.));
#32516=DIRECTION('center_axis',(-0.707106781186554,-0.707106781186541,0.));
#32517=DIRECTION('ref_axis',(0.,0.,1.));
#32518=DIRECTION('',(0.577350269189613,-0.577350269189624,-0.577350269189641));
#32519=DIRECTION('center_axis',(-0.707106781186564,0.,-0.707106781186531));
#32520=DIRECTION('ref_axis',(-0.707106781186531,0.,0.707106781186564));
#32521=DIRECTION('',(0.,-1.,0.));
#32522=DIRECTION('center_axis',(-0.707106781186541,-0.707106781186554,0.));
#32523=DIRECTION('ref_axis',(0.,0.,1.));
#32524=DIRECTION('center_axis',(0.,8.71363591613481E-16,1.));
#32525=DIRECTION('ref_axis',(-1.,-3.01769808787504E-17,0.));
#32526=DIRECTION('center_axis',(0.,0.,-1.));
#32527=DIRECTION('ref_axis',(-1.,0.,0.));
#32528=DIRECTION('center_axis',(0.,0.,-1.));
#32529=DIRECTION('ref_axis',(-1.,0.,0.));
#32530=DIRECTION('',(-0.382683432365075,-8.63448422341581E-16,-0.923879532511293));
#32531=DIRECTION('center_axis',(0.,0.,1.));
#32532=DIRECTION('ref_axis',(-1.,-6.12323399573677E-17,0.));
#32533=DIRECTION('center_axis',(0.,0.,1.));
#32534=DIRECTION('ref_axis',(-1.,-6.12323399573677E-17,0.));
#32535=DIRECTION('center_axis',(0.,0.,1.));
#32536=DIRECTION('ref_axis',(1.,0.,0.));
#32537=DIRECTION('',(0.707106781186543,8.65956056235488E-17,-0.707106781186552));
#32538=DIRECTION('center_axis',(0.,0.,-1.));
#32539=DIRECTION('ref_axis',(-1.,-6.12323399573677E-17,0.));
#32540=DIRECTION('center_axis',(0.,0.,-1.));
#32541=DIRECTION('ref_axis',(-1.,-6.12323399573677E-17,0.));
#32542=DIRECTION('center_axis',(0.,0.,1.));
#32543=DIRECTION('ref_axis',(1.,0.,0.));
#32544=DIRECTION('center_axis',(0.,0.,1.));
#32545=DIRECTION('ref_axis',(1.,0.,0.));
#32546=DIRECTION('',(0.,0.,-1.));
#32547=DIRECTION('center_axis',(0.,-2.05293126929891E-15,1.));
#32548=DIRECTION('ref_axis',(-1.,-3.17596479860489E-17,0.));
#32549=DIRECTION('',(-0.923879532511284,6.43138084582096E-16,-0.382683432365096));
#32550=DIRECTION('center_axis',(0.,0.,1.));
#32551=DIRECTION('ref_axis',(-1.,0.,0.));
#32552=DIRECTION('center_axis',(0.,0.,-1.));
#32553=DIRECTION('ref_axis',(-1.,0.,0.));
#32554=DIRECTION('center_axis',(0.,0.,-1.));
#32555=DIRECTION('ref_axis',(1.,0.,0.));
#32556=DIRECTION('',(0.707106781186573,-8.65956056235524E-17,0.707106781186522));
#32557=DIRECTION('center_axis',(0.,0.,1.));
#32558=DIRECTION('ref_axis',(1.,0.,0.));
#32559=DIRECTION('center_axis',(0.,0.,1.));
#32560=DIRECTION('ref_axis',(1.,0.,0.));
#32561=DIRECTION('',(0.,0.,1.));
#32562=DIRECTION('center_axis',(0.,0.,-1.));
#32563=DIRECTION('ref_axis',(1.,0.,0.));
#32564=DIRECTION('center_axis',(0.,0.,1.));
#32565=DIRECTION('ref_axis',(1.,0.,0.));
#32566=DIRECTION('center_axis',(0.,0.,1.));
#32567=DIRECTION('ref_axis',(1.,0.,0.));
#32568=DIRECTION('',(0.707106781186573,8.65956056235524E-17,-0.707106781186522));
#32569=DIRECTION('center_axis',(0.,0.,1.));
#32570=DIRECTION('ref_axis',(1.,0.,0.));
#32571=DIRECTION('center_axis',(0.,0.,1.));
#32572=DIRECTION('ref_axis',(1.,0.,0.));
#32573=DIRECTION('center_axis',(0.,0.,-1.));
#32574=DIRECTION('ref_axis',(1.,0.,0.));
#32575=DIRECTION('',(0.707106781186573,-8.65956056235524E-17,0.707106781186522));
#32576=DIRECTION('center_axis',(0.,0.,1.));
#32577=DIRECTION('ref_axis',(1.,0.,0.));
#32578=DIRECTION('center_axis',(0.,0.,1.));
#32579=DIRECTION('ref_axis',(1.,0.,0.));
#32580=DIRECTION('',(0.,0.,1.));
#32581=DIRECTION('center_axis',(0.,0.,-1.));
#32582=DIRECTION('ref_axis',(1.,0.,0.));
#32583=DIRECTION('center_axis',(0.,0.,1.));
#32584=DIRECTION('ref_axis',(1.,0.,0.));
#32585=DIRECTION('',(0.707106781186573,8.65956056235524E-17,-0.707106781186522));
#32586=DIRECTION('center_axis',(0.,0.,1.));
#32587=DIRECTION('ref_axis',(1.,0.,0.));
#32588=DIRECTION('center_axis',(0.,0.,1.));
#32589=DIRECTION('ref_axis',(1.,0.,0.));
#32590=DIRECTION('',(0.650791373455974,7.96989572415569E-17,-0.759256602365292));
#32591=DIRECTION('center_axis',(0.,0.,-1.));
#32592=DIRECTION('ref_axis',(0.,1.,0.));
#32593=DIRECTION('center_axis',(0.,0.,-1.));
#32594=DIRECTION('ref_axis',(0.,1.,0.));
#32595=DIRECTION('center_axis',(0.,0.,1.));
#32596=DIRECTION('ref_axis',(1.,0.,0.));
#32597=DIRECTION('center_axis',(0.,0.,1.));
#32598=DIRECTION('ref_axis',(1.,0.,0.));
#32599=DIRECTION('center_axis',(1.,0.,0.));
#32600=DIRECTION('ref_axis',(0.,1.,0.));
#32601=DIRECTION('',(0.,-1.,0.));
#32602=DIRECTION('center_axis',(0.,0.,1.));
#32603=DIRECTION('ref_axis',(0.,-1.,0.));
#32604=DIRECTION('axis',(0.,0.,1.));
#32605=DIRECTION('refdir',(1.,0.,0.));
#32606=DIRECTION('center_axis',(-0.707106781186548,0.,-0.707106781186548));
#32607=DIRECTION('ref_axis',(-0.707106781186548,0.,0.707106781186548));
#32608=DIRECTION('',(-0.707106781186548,0.,0.707106781186548));
#32609=DIRECTION('',(0.,-1.,0.));
#32610=DIRECTION('',(0.707106781186548,0.,-0.707106781186548));
#32611=DIRECTION('',(0.,1.,0.));
#32612=DIRECTION('center_axis',(0.,0.,1.));
#32613=DIRECTION('ref_axis',(1.,0.,0.));
#32614=DIRECTION('',(-1.,0.,0.));
#32615=DIRECTION('',(0.,1.,0.));
#32616=DIRECTION('',(1.,0.,0.));
#32617=DIRECTION('center_axis',(0.,0.707106781186529,-0.707106781186566));
#32618=DIRECTION('ref_axis',(-1.,0.,0.));
#32619=DIRECTION('',(-0.577350269189616,-0.577350269189646,-0.577350269189616));
#32620=DIRECTION('',(-1.,0.,0.));
#32621=DIRECTION('',(-0.577350269189616,0.577350269189646,0.577350269189616));
#32622=DIRECTION('',(0.577350269189616,0.577350269189646,0.577350269189616));
#32623=DIRECTION('',(1.,0.,0.));
#32624=DIRECTION('',(0.577350269189616,-0.577350269189646,-0.577350269189616));
#32625=DIRECTION('center_axis',(0.,1.,0.));
#32626=DIRECTION('ref_axis',(0.,0.,1.));
#32627=DIRECTION('',(0.,0.,-1.));
#32628=DIRECTION('',(-1.,0.,0.));
#32629=DIRECTION('',(0.,0.,1.));
#32630=DIRECTION('center_axis',(-0.707106781186566,0.707106781186529,0.));
#32631=DIRECTION('ref_axis',(0.,0.,1.));
#32632=DIRECTION('',(0.577350269189616,0.577350269189646,-0.577350269189616));
#32633=DIRECTION('',(0.,0.,1.));
#32634=DIRECTION('',(-0.577350269189616,-0.577350269189646,-0.577350269189616));
#32635=DIRECTION('',(-0.577350269189616,-0.577350269189646,0.577350269189616));
#32636=DIRECTION('center_axis',(-0.707106781186548,0.,-0.707106781186548));
#32637=DIRECTION('ref_axis',(-0.707106781186548,0.,0.707106781186548));
#32638=DIRECTION('',(0.,-1.,0.));
#32639=DIRECTION('',(0.577350269189616,0.577350269189646,-0.577350269189616));
#32640=DIRECTION('',(0.577350269189616,-0.577350269189646,-0.577350269189616));
#32641=DIRECTION('',(0.,1.,0.));
#32642=DIRECTION('center_axis',(-0.707106781186522,0.,0.707106781186573));
#32643=DIRECTION('ref_axis',(0.707106781186573,0.,0.707106781186522));
#32644=DIRECTION('',(0.707106781186573,0.,0.707106781186522));
#32645=DIRECTION('',(0.,-1.,0.));
#32646=DIRECTION('',(-0.707106781186573,0.,-0.707106781186522));
#32647=DIRECTION('',(0.,1.,0.));
#32648=DIRECTION('center_axis',(-1.,0.,0.));
#32649=DIRECTION('ref_axis',(0.,-1.,0.));
#32650=DIRECTION('',(0.,0.,-1.));
#32651=DIRECTION('',(0.,0.,1.));
#32652=DIRECTION('center_axis',(0.707106781186548,0.,-0.707106781186548));
#32653=DIRECTION('ref_axis',(-0.707106781186548,0.,-0.707106781186548));
#32654=DIRECTION('',(0.707106781186548,0.,0.707106781186548));
#32655=DIRECTION('',(0.,1.,0.));
#32656=DIRECTION('',(-0.707106781186548,0.,-0.707106781186548));
#32657=DIRECTION('',(0.,-1.,0.));
#32658=DIRECTION('center_axis',(0.,0.,1.));
#32659=DIRECTION('ref_axis',(1.,0.,0.));
#32660=DIRECTION('',(1.,0.,0.));
#32661=DIRECTION('',(0.,-1.,0.));
#32662=DIRECTION('',(-1.,0.,0.));
#32663=DIRECTION('center_axis',(0.,-0.707106781186529,0.707106781186566));
#32664=DIRECTION('ref_axis',(1.,0.,0.));
#32665=DIRECTION('',(-0.577350269189616,0.577350269189646,0.577350269189616));
#32666=DIRECTION('',(-1.,0.,0.));
#32667=DIRECTION('',(-0.577350269189643,-0.577350269189633,-0.577350269189602));
#32668=DIRECTION('',(0.577350269189643,-0.577350269189633,-0.577350269189602));
#32669=DIRECTION('',(1.,0.,0.));
#32670=DIRECTION('',(0.577350269189616,0.577350269189646,0.577350269189616));
#32671=DIRECTION('center_axis',(0.707106781186566,-0.707106781186529,0.));
#32672=DIRECTION('ref_axis',(0.,0.,-1.));
#32673=DIRECTION('',(0.,0.,-1.));
#32674=DIRECTION('',(-0.577350269189616,-0.577350269189646,0.577350269189616));
#32675=DIRECTION('',(-0.577350269189616,-0.577350269189646,-0.577350269189616));
#32676=DIRECTION('',(0.,0.,1.));
#32677=DIRECTION('',(0.577350269189616,0.577350269189646,-0.577350269189616));
#32678=DIRECTION('center_axis',(0.,-1.,0.));
#32679=DIRECTION('ref_axis',(0.,0.,-1.));
#32680=DIRECTION('',(0.,0.,1.));
#32681=DIRECTION('',(-1.,0.,0.));
#32682=DIRECTION('center_axis',(-0.707106781186541,-0.707106781186554,0.));
#32683=DIRECTION('ref_axis',(0.,0.,1.));
#32684=DIRECTION('',(0.577350269189643,-0.577350269189633,0.577350269189602));
#32685=DIRECTION('',(0.,0.,-1.));
#32686=DIRECTION('',(-0.577350269189643,0.577350269189633,0.577350269189602));
#32687=DIRECTION('',(-0.577350269189643,0.577350269189633,-0.577350269189602));
#32688=DIRECTION('center_axis',(0.,-0.707106781186529,-0.707106781186566));
#32689=DIRECTION('ref_axis',(-1.,0.,0.));
#32690=DIRECTION('',(0.577350269189643,0.577350269189633,-0.577350269189602));
#32691=DIRECTION('',(1.,0.,0.));
#32692=DIRECTION('',(0.577350269189616,-0.577350269189646,0.577350269189616));
#32693=DIRECTION('center_axis',(0.707106781186548,0.,-0.707106781186548));
#32694=DIRECTION('ref_axis',(-0.707106781186548,0.,-0.707106781186548));
#32695=DIRECTION('',(0.,1.,0.));
#32696=DIRECTION('',(0.707106781186548,0.,0.707106781186548));
#32697=DIRECTION('',(0.,-1.,0.));
#32698=DIRECTION('center_axis',(0.,0.,-1.));
#32699=DIRECTION('ref_axis',(0.,1.,0.));
#32700=DIRECTION('',(0.,-1.,0.));
#32701=DIRECTION('',(-1.,0.,0.));
#32702=DIRECTION('center_axis',(-0.707106781186522,0.,-0.707106781186573));
#32703=DIRECTION('ref_axis',(-0.707106781186573,0.,0.707106781186522));
#32704=DIRECTION('',(0.,1.,0.));
#32705=DIRECTION('',(0.577350269189643,0.577350269189633,-0.577350269189602));
#32706=DIRECTION('',(-0.577350269189643,0.577350269189633,0.577350269189602));
#32707=DIRECTION('center_axis',(0.707106781186548,0.,0.707106781186548));
#32708=DIRECTION('ref_axis',(0.707106781186548,0.,-0.707106781186548));
#32709=DIRECTION('',(0.,1.,0.));
#32710=DIRECTION('',(-0.577350269189614,-0.57735026918965,0.577350269189614));
#32711=DIRECTION('',(0.,-1.,0.));
#32712=DIRECTION('center_axis',(0.70710678118657,-0.707106781186526,0.));
#32713=DIRECTION('ref_axis',(0.,0.,-1.));
#32714=DIRECTION('',(0.,0.,1.));
#32715=DIRECTION('',(0.577350269189614,0.57735026918965,0.577350269189614));
#32716=DIRECTION('',(0.,0.,-1.));
#32717=DIRECTION('center_axis',(0.,0.,1.));
#32718=DIRECTION('ref_axis',(0.,-1.,0.));
#32719=DIRECTION('',(1.,0.,0.));
#32720=DIRECTION('',(0.,1.,0.));
#32721=DIRECTION('center_axis',(0.,-1.,0.));
#32722=DIRECTION('ref_axis',(0.,0.,-1.));
#32723=DIRECTION('',(1.,0.,0.));
#32724=DIRECTION('',(0.,0.,1.));
#32725=DIRECTION('center_axis',(0.707106781186522,0.,0.707106781186573));
#32726=DIRECTION('ref_axis',(0.707106781186573,0.,-0.707106781186522));
#32727=DIRECTION('',(-0.707106781186573,0.,0.707106781186522));
#32728=DIRECTION('',(0.,1.,0.));
#32729=DIRECTION('',(0.707106781186573,0.,-0.707106781186522));
#32730=DIRECTION('',(0.,-1.,0.));
#32731=DIRECTION('center_axis',(1.,0.,0.));
#32732=DIRECTION('ref_axis',(0.,1.,0.));
#32733=DIRECTION('',(0.,0.,-1.));
#32734=DIRECTION('',(0.,0.,1.));
#32735=DIRECTION('center_axis',(0.577350269189636,0.577350269189605,-0.577350269189636));
#32736=DIRECTION('ref_axis',(-0.707106781186548,0.,-0.707106781186548));
#32737=DIRECTION('',(0.,-0.707106781186566,-0.707106781186529));
#32738=DIRECTION('',(-0.707106781186529,0.707106781186566,0.));
#32739=DIRECTION('center_axis',(0.,0.707106781186529,-0.707106781186566));
#32740=DIRECTION('ref_axis',(-1.,0.,0.));
#32741=DIRECTION('',(0.577350269189643,0.577350269189633,0.577350269189602));
#32742=DIRECTION('',(1.,0.,0.));
#32743=DIRECTION('center_axis',(0.577350269189636,-0.577350269189605,-0.577350269189636));
#32744=DIRECTION('ref_axis',(-0.707106781186548,0.,-0.707106781186548));
#32745=DIRECTION('',(0.707106781186529,0.707106781186566,0.));
#32746=DIRECTION('',(0.,-0.707106781186566,0.707106781186529));
#32747=DIRECTION('',(-0.707106781186548,0.,-0.707106781186548));
#32748=DIRECTION('center_axis',(0.,-0.707106781186529,-0.707106781186566));
#32749=DIRECTION('ref_axis',(-1.,0.,0.));
#32750=DIRECTION('',(1.,0.,0.));
#32751=DIRECTION('',(-1.,0.,0.));
#32752=DIRECTION('',(-0.577350269189616,0.577350269189646,-0.577350269189616));
#32753=DIRECTION('center_axis',(0.707106781186548,0.,-0.707106781186548));
#32754=DIRECTION('ref_axis',(-0.707106781186548,0.,-0.707106781186548));
#32755=DIRECTION('',(0.577350269189616,-0.577350269189646,0.577350269189616));
#32756=DIRECTION('',(0.,-1.,0.));
#32757=DIRECTION('',(0.,1.,0.));
#32758=DIRECTION('center_axis',(0.707106781186566,-0.707106781186529,0.));
#32759=DIRECTION('ref_axis',(0.,0.,-1.));
#32760=DIRECTION('',(0.,0.,-1.));
#32761=DIRECTION('',(0.,0.,1.));
#32762=DIRECTION('',(-0.577350269189616,-0.577350269189646,-0.577350269189616));
#32763=DIRECTION('center_axis',(0.707106781186548,0.,-0.707106781186548));
#32764=DIRECTION('ref_axis',(-0.707106781186548,0.,-0.707106781186548));
#32765=DIRECTION('',(0.,-1.,0.));
#32766=DIRECTION('',(-0.577350269189616,0.577350269189646,-0.577350269189616));
#32767=DIRECTION('center_axis',(0.707106781186566,0.707106781186529,0.));
#32768=DIRECTION('ref_axis',(0.,0.,-1.));
#32769=DIRECTION('',(0.,0.,-1.));
#32770=DIRECTION('',(0.,0.,1.));
#32771=DIRECTION('center_axis',(-0.707106781186541,0.707106781186554,0.));
#32772=DIRECTION('ref_axis',(0.,0.,1.));
#32773=DIRECTION('',(0.,0.,1.));
#32774=DIRECTION('',(0.577350269189616,0.577350269189646,-0.577350269189616));
#32775=DIRECTION('',(0.,0.,-1.));
#32776=DIRECTION('center_axis',(1.,0.,0.));
#32777=DIRECTION('ref_axis',(0.,0.,-1.));
#32778=DIRECTION('',(0.,0.,-1.));
#32779=DIRECTION('',(0.,1.,0.));
#32780=DIRECTION('',(0.,0.,-1.));
#32781=DIRECTION('',(0.,-1.,0.));
#32782=DIRECTION('',(0.,0.,-1.));
#32783=DIRECTION('',(0.,1.,0.));
#32784=DIRECTION('',(0.,0.,1.));
#32785=DIRECTION('',(0.,1.,0.));
#32786=DIRECTION('',(0.,0.,-1.));
#32787=DIRECTION('',(0.,1.,0.));
#32788=DIRECTION('',(0.,0.,1.));
#32789=DIRECTION('',(0.,-1.,0.));
#32790=DIRECTION('center_axis',(0.,0.707106781186529,0.707106781186566));
#32791=DIRECTION('ref_axis',(1.,0.,0.));
#32792=DIRECTION('',(-0.577350269189616,0.577350269189646,-0.577350269189616));
#32793=DIRECTION('',(0.577350269189616,-0.577350269189646,0.577350269189616));
#32794=DIRECTION('',(1.,0.,0.));
#32795=DIRECTION('',(0.577350269189616,0.577350269189646,-0.577350269189616));
#32796=DIRECTION('center_axis',(0.707106781186548,0.,0.707106781186548));
#32797=DIRECTION('ref_axis',(0.707106781186548,0.,-0.707106781186548));
#32798=DIRECTION('',(0.,-1.,0.));
#32799=DIRECTION('',(-0.577350269189616,0.577350269189646,0.577350269189616));
#32800=DIRECTION('',(-0.577350269189616,0.577350269189646,0.577350269189616));
#32801=DIRECTION('center_axis',(0.,0.,1.));
#32802=DIRECTION('ref_axis',(0.,-1.,0.));
#32803=DIRECTION('',(0.,1.,0.));
#32804=DIRECTION('',(1.,0.,0.));
#32805=DIRECTION('center_axis',(-0.707106781186548,0.,0.707106781186548));
#32806=DIRECTION('ref_axis',(0.707106781186548,0.,0.707106781186548));
#32807=DIRECTION('',(0.,-1.,0.));
#32808=DIRECTION('',(0.577350269189614,0.57735026918965,0.577350269189614));
#32809=DIRECTION('center_axis',(0.707106781186566,0.707106781186529,0.));
#32810=DIRECTION('ref_axis',(0.,0.,-1.));
#32811=DIRECTION('',(0.,0.,1.));
#32812=DIRECTION('',(-0.577350269189616,0.577350269189646,-0.577350269189616));
#32813=DIRECTION('center_axis',(0.707106781186566,0.707106781186529,0.));
#32814=DIRECTION('ref_axis',(0.,0.,-1.));
#32815=DIRECTION('',(0.,0.,1.));
#32816=DIRECTION('',(0.577350269189616,-0.577350269189646,0.577350269189616));
#32817=DIRECTION('',(0.577350269189616,-0.577350269189646,-0.577350269189616));
#32818=DIRECTION('',(-0.577350269189616,0.577350269189646,0.577350269189616));
#32819=DIRECTION('center_axis',(0.707106781186522,0.,0.707106781186573));
#32820=DIRECTION('ref_axis',(0.707106781186573,0.,-0.707106781186522));
#32821=DIRECTION('',(-0.577350269189616,-0.577350269189646,0.577350269189616));
#32822=DIRECTION('',(0.,-1.,0.));
#32823=DIRECTION('center_axis',(0.577350269189636,-0.577350269189605,0.577350269189636));
#32824=DIRECTION('ref_axis',(0.707106781186548,0.,-0.707106781186548));
#32825=DIRECTION('',(0.707106781186548,0.,-0.707106781186548));
#32826=DIRECTION('',(0.,0.707106781186566,0.707106781186529));
#32827=DIRECTION('',(-0.707106781186529,-0.707106781186566,0.));
#32828=DIRECTION('center_axis',(0.,-0.707106781186529,0.707106781186566));
#32829=DIRECTION('ref_axis',(1.,0.,0.));
#32830=DIRECTION('',(0.577350269189616,-0.577350269189646,-0.577350269189616));
#32831=DIRECTION('',(1.,0.,0.));
#32832=DIRECTION('',(-1.,0.,0.));
#32833=DIRECTION('',(-0.577350269189616,-0.577350269189646,-0.577350269189616));
#32834=DIRECTION('center_axis',(0.707106781186566,-0.707106781186529,0.));
#32835=DIRECTION('ref_axis',(0.,0.,-1.));
#32836=DIRECTION('',(0.,0.,-1.));
#32837=DIRECTION('center_axis',(0.707106781186548,0.,0.707106781186548));
#32838=DIRECTION('ref_axis',(0.707106781186548,0.,-0.707106781186548));
#32839=DIRECTION('',(-0.577350269189616,-0.577350269189646,0.577350269189616));
#32840=DIRECTION('',(0.,-1.,0.));
#32841=DIRECTION('',(-0.577350269189616,0.577350269189646,0.577350269189616));
#32842=DIRECTION('center_axis',(0.,0.,1.));
#32843=DIRECTION('ref_axis',(1.,0.,0.));
#32844=DIRECTION('',(-1.,0.,0.));
#32845=DIRECTION('',(1.,0.,0.));
#32846=DIRECTION('center_axis',(0.,-1.,0.));
#32847=DIRECTION('ref_axis',(0.,0.,-1.));
#32848=DIRECTION('',(0.,0.,1.));
#32849=DIRECTION('',(1.,0.,0.));
#32850=DIRECTION('',(0.,0.,1.));
#32851=DIRECTION('center_axis',(-0.707106781186566,-0.707106781186529,0.));
#32852=DIRECTION('ref_axis',(0.,0.,1.));
#32853=DIRECTION('',(0.577350269189616,-0.577350269189646,0.577350269189616));
#32854=DIRECTION('',(0.,0.,-1.));
#32855=DIRECTION('',(0.577350269189616,-0.577350269189646,0.577350269189616));
#32856=DIRECTION('center_axis',(-0.707106781186548,0.,0.707106781186548));
#32857=DIRECTION('ref_axis',(0.707106781186548,0.,0.707106781186548));
#32858=DIRECTION('',(0.,1.,0.));
#32859=DIRECTION('',(0.577350269189616,-0.577350269189646,0.577350269189616));
#32860=DIRECTION('',(-0.577350269189616,-0.577350269189646,-0.577350269189616));
#32861=DIRECTION('',(0.,-1.,0.));
#32862=DIRECTION('center_axis',(0.,0.,1.));
#32863=DIRECTION('ref_axis',(0.,-1.,0.));
#32864=DIRECTION('',(1.,0.,0.));
#32865=DIRECTION('',(1.,0.,0.));
#32866=DIRECTION('center_axis',(0.,0.,1.));
#32867=DIRECTION('ref_axis',(0.,1.,0.));
#32868=DIRECTION('',(-1.,0.,0.));
#32869=DIRECTION('center_axis',(0.,0.,1.));
#32870=DIRECTION('ref_axis',(0.,-1.,0.));
#32871=DIRECTION('center_axis',(0.,0.707106781186529,0.707106781186566));
#32872=DIRECTION('ref_axis',(1.,0.,0.));
#32873=DIRECTION('',(-0.577350269189616,0.577350269189646,-0.577350269189616));
#32874=DIRECTION('',(-1.,0.,0.));
#32875=DIRECTION('',(-0.577350269189616,-0.577350269189646,0.577350269189616));
#32876=DIRECTION('center_axis',(-0.707106781186566,0.707106781186529,0.));
#32877=DIRECTION('ref_axis',(0.,0.,1.));
#32878=DIRECTION('',(0.,0.,-1.));
#32879=DIRECTION('',(0.577350269189616,0.577350269189646,0.577350269189616));
#32880=DIRECTION('',(0.577350269189616,0.577350269189646,-0.577350269189616));
#32881=DIRECTION('',(0.,0.,1.));
#32882=DIRECTION('center_axis',(0.,0.707106781186529,-0.707106781186566));
#32883=DIRECTION('ref_axis',(-1.,0.,0.));
#32884=DIRECTION('',(-0.577350269189616,-0.577350269189646,-0.577350269189616));
#32885=DIRECTION('',(-1.,0.,0.));
#32886=DIRECTION('',(-0.577350269189616,0.577350269189646,0.577350269189616));
#32887=DIRECTION('',(1.,0.,0.));
#32888=DIRECTION('',(0.577350269189616,-0.577350269189646,-0.577350269189616));
#32889=DIRECTION('center_axis',(-0.707106781186548,0.,-0.707106781186548));
#32890=DIRECTION('ref_axis',(-0.707106781186548,0.,0.707106781186548));
#32891=DIRECTION('',(0.,-1.,0.));
#32892=DIRECTION('',(0.577350269189614,0.57735026918965,-0.577350269189614));
#32893=DIRECTION('',(0.,1.,0.));
#32894=DIRECTION('center_axis',(0.,0.,-1.));
#32895=DIRECTION('ref_axis',(0.,1.,0.));
#32896=DIRECTION('',(0.,1.,0.));
#32897=DIRECTION('',(1.,0.,0.));
#32898=DIRECTION('',(-1.,0.,0.));
#32899=DIRECTION('center_axis',(0.,0.,-1.));
#32900=DIRECTION('ref_axis',(0.,-1.,0.));
#32901=DIRECTION('',(1.,0.,0.));
#32902=DIRECTION('center_axis',(0.,0.,-1.));
#32903=DIRECTION('ref_axis',(0.,1.,0.));
#32904=DIRECTION('center_axis',(0.707106781186548,0.,-0.707106781186548));
#32905=DIRECTION('ref_axis',(-0.707106781186548,0.,-0.707106781186548));
#32906=DIRECTION('',(0.577350269189616,-0.577350269189646,0.577350269189616));
#32907=DIRECTION('center_axis',(0.707106781186566,0.707106781186529,0.));
#32908=DIRECTION('ref_axis',(0.,0.,-1.));
#32909=DIRECTION('',(0.,0.,1.));
#32910=DIRECTION('center_axis',(-0.707106781186548,0.,-0.707106781186548));
#32911=DIRECTION('ref_axis',(-0.707106781186548,0.,0.707106781186548));
#32912=DIRECTION('',(0.,1.,0.));
#32913=DIRECTION('',(0.577350269189616,-0.577350269189646,-0.577350269189616));
#32914=DIRECTION('center_axis',(-0.707106781186566,-0.707106781186529,0.));
#32915=DIRECTION('ref_axis',(0.,0.,1.));
#32916=DIRECTION('',(0.,0.,-1.));
#32917=DIRECTION('center_axis',(1.,0.,0.));
#32918=DIRECTION('ref_axis',(0.,0.,-1.));
#32919=DIRECTION('',(0.,-1.,0.));
#32920=DIRECTION('',(0.,0.,-1.));
#32921=DIRECTION('',(0.,1.,0.));
#32922=DIRECTION('',(0.,0.,-1.));
#32923=DIRECTION('',(0.,-1.,0.));
#32924=DIRECTION('',(0.,0.,1.));
#32925=DIRECTION('',(0.,-1.,0.));
#32926=DIRECTION('',(0.,0.,1.));
#32927=DIRECTION('center_axis',(-0.70710678118657,0.707106781186526,0.));
#32928=DIRECTION('ref_axis',(0.,0.,1.));
#32929=DIRECTION('',(0.,0.,-1.));
#32930=DIRECTION('center_axis',(0.,1.,0.));
#32931=DIRECTION('ref_axis',(0.,0.,1.));
#32932=DIRECTION('center_axis',(-0.577350269189609,0.577350269189619,0.57735026918965));
#32933=DIRECTION('ref_axis',(0.707106781186573,0.,0.707106781186523));
#32934=DIRECTION('',(0.,-0.707106781186566,0.707106781186529));
#32935=DIRECTION('',(0.707106781186554,0.707106781186541,0.));
#32936=DIRECTION('',(-0.707106781186573,0.,-0.707106781186522));
#32937=DIRECTION('center_axis',(-0.707106781186541,0.707106781186554,0.));
#32938=DIRECTION('ref_axis',(0.,0.,1.));
#32939=DIRECTION('',(0.,0.,-1.));
#32940=DIRECTION('',(-0.577350269189643,-0.577350269189633,-0.577350269189602));
#32941=DIRECTION('center_axis',(-0.707106781186522,0.,0.707106781186573));
#32942=DIRECTION('ref_axis',(0.707106781186573,0.,0.707106781186522));
#32943=DIRECTION('',(0.577350269189643,0.577350269189633,0.577350269189602));
#32944=DIRECTION('',(0.,1.,0.));
#32945=DIRECTION('',(0.577350269189643,-0.577350269189633,0.577350269189602));
#32946=DIRECTION('center_axis',(0.,0.707106781186529,0.707106781186566));
#32947=DIRECTION('ref_axis',(1.,0.,0.));
#32948=DIRECTION('',(-1.,0.,0.));
#32949=DIRECTION('',(1.,0.,0.));
#32950=DIRECTION('',(0.577350269189616,0.577350269189646,-0.577350269189616));
#32951=DIRECTION('center_axis',(-0.707106781186522,0.,0.707106781186573));
#32952=DIRECTION('ref_axis',(0.707106781186573,0.,0.707106781186522));
#32953=DIRECTION('',(0.,1.,0.));
#32954=DIRECTION('center_axis',(0.707106781186548,0.,0.707106781186548));
#32955=DIRECTION('ref_axis',(0.707106781186548,0.,-0.707106781186548));
#32956=DIRECTION('',(0.,-1.,0.));
#32957=DIRECTION('',(0.577350269189616,-0.577350269189646,-0.577350269189616));
#32958=DIRECTION('',(0.577350269189616,0.577350269189646,-0.577350269189616));
#32959=DIRECTION('center_axis',(0.,0.,1.));
#32960=DIRECTION('ref_axis',(1.,0.,0.));
#32961=DIRECTION('',(-1.,0.,0.));
#32962=DIRECTION('center_axis',(0.,1.,0.));
#32963=DIRECTION('ref_axis',(0.,0.,1.));
#32964=DIRECTION('center_axis',(0.707106781186566,-0.707106781186529,0.));
#32965=DIRECTION('ref_axis',(0.,0.,-1.));
#32966=DIRECTION('',(0.577350269189616,0.577350269189646,0.577350269189616));
#32967=DIRECTION('',(0.,0.,-1.));
#32968=DIRECTION('',(-0.577350269189616,-0.577350269189646,0.577350269189616));
#32969=DIRECTION('',(-0.577350269189616,-0.577350269189646,-0.577350269189616));
#32970=DIRECTION('center_axis',(-0.707106781186544,-0.707106781186551,0.));
#32971=DIRECTION('ref_axis',(0.,0.,1.));
#32972=DIRECTION('',(0.577350269189641,-0.577350269189636,-0.5773502691896));
#32973=DIRECTION('',(0.577350269189641,-0.577350269189636,0.5773502691896));
#32974=DIRECTION('center_axis',(-0.707106781186522,0.,0.707106781186573));
#32975=DIRECTION('ref_axis',(0.707106781186573,0.,0.707106781186522));
#32976=DIRECTION('center_axis',(0.707106781186548,0.,-0.707106781186548));
#32977=DIRECTION('ref_axis',(-0.707106781186548,0.,-0.707106781186548));
#32978=DIRECTION('',(-0.577350269189616,0.577350269189646,-0.577350269189616));
#32979=DIRECTION('',(0.,1.,0.));
#32980=DIRECTION('center_axis',(0.,0.,-1.));
#32981=DIRECTION('ref_axis',(0.,1.,0.));
#32982=DIRECTION('',(1.,0.,0.));
#32983=DIRECTION('',(0.,-1.,0.));
#32984=DIRECTION('',(-1.,0.,0.));
#32985=DIRECTION('center_axis',(0.,0.,-1.));
#32986=DIRECTION('ref_axis',(0.,-1.,0.));
#32987=DIRECTION('',(1.,0.,0.));
#32988=DIRECTION('center_axis',(0.,0.,-1.));
#32989=DIRECTION('ref_axis',(0.,1.,0.));
#32990=DIRECTION('center_axis',(0.,-0.707106781186529,-0.707106781186566));
#32991=DIRECTION('ref_axis',(-1.,0.,0.));
#32992=DIRECTION('',(-1.,0.,0.));
#32993=DIRECTION('',(-0.577350269189643,0.577350269189633,-0.577350269189602));
#32994=DIRECTION('',(-0.577350269189643,-0.577350269189633,0.577350269189602));
#32995=DIRECTION('center_axis',(-0.707106781186522,0.,-0.707106781186573));
#32996=DIRECTION('ref_axis',(-0.707106781186573,0.,0.707106781186522));
#32997=DIRECTION('',(-0.577350269189643,0.577350269189633,0.577350269189602));
#32998=DIRECTION('center_axis',(-0.707106781186541,-0.707106781186554,0.));
#32999=DIRECTION('ref_axis',(0.,0.,1.));
#33000=DIRECTION('',(0.,0.,1.));
#33001=DIRECTION('',(0.577350269189643,-0.577350269189633,-0.577350269189602));
#33002=DIRECTION('center_axis',(0.,-0.707106781186529,0.707106781186566));
#33003=DIRECTION('ref_axis',(1.,0.,0.));
#33004=DIRECTION('',(1.,0.,0.));
#33005=DIRECTION('',(-1.,0.,0.));
#33006=DIRECTION('center_axis',(0.,0.,1.));
#33007=DIRECTION('ref_axis',(0.,-1.,0.));
#33008=DIRECTION('',(1.,0.,0.));
#33009=DIRECTION('center_axis',(0.,0.,1.));
#33010=DIRECTION('ref_axis',(0.,1.,0.));
#33011=DIRECTION('',(-1.,0.,0.));
#33012=DIRECTION('center_axis',(0.,0.,1.));
#33013=DIRECTION('ref_axis',(0.,-1.,0.));
#33014=DIRECTION('center_axis',(0.,0.707106781186529,-0.707106781186566));
#33015=DIRECTION('ref_axis',(-1.,0.,0.));
#33016=DIRECTION('',(0.,-0.707106781186566,-0.707106781186529));
#33017=DIRECTION('',(0.,0.70710678118657,0.707106781186526));
#33018=DIRECTION('',(1.,0.,0.));
#33019=DIRECTION('center_axis',(0.,0.,-1.));
#33020=DIRECTION('ref_axis',(0.,-1.,0.));
#33021=DIRECTION('',(0.,0.70710678118657,-0.707106781186526));
#33022=DIRECTION('center_axis',(0.,0.,1.));
#33023=DIRECTION('ref_axis',(0.,-1.,0.));
#33024=DIRECTION('center_axis',(0.,-0.707106781186529,-0.707106781186566));
#33025=DIRECTION('ref_axis',(-1.,0.,0.));
#33026=DIRECTION('',(0.,0.707106781186566,-0.707106781186529));
#33027=DIRECTION('',(-1.,0.,0.));
#33028=DIRECTION('center_axis',(0.,0.,-1.));
#33029=DIRECTION('ref_axis',(0.,1.,0.));
#33030=DIRECTION('center_axis',(0.,0.,1.));
#33031=DIRECTION('ref_axis',(0.,1.,0.));
#33032=DIRECTION('center_axis',(0.,0.,-1.));
#33033=DIRECTION('ref_axis',(0.,-1.,0.));
#33034=DIRECTION('',(0.,0.,-1.));
#33035=DIRECTION('center_axis',(0.,0.,-1.));
#33036=DIRECTION('ref_axis',(0.,-1.,0.));
#33037=DIRECTION('',(0.,0.,-1.));
#33038=DIRECTION('center_axis',(0.,-1.,0.));
#33039=DIRECTION('ref_axis',(-1.,0.,0.));
#33040=DIRECTION('',(0.,0.,-1.));
#33041=DIRECTION('',(-1.,0.,0.));
#33042=DIRECTION('center_axis',(0.,0.707106781186532,0.707106781186563));
#33043=DIRECTION('ref_axis',(1.,0.,0.));
#33044=DIRECTION('',(0.,-0.707106781186566,0.707106781186529));
#33045=DIRECTION('',(0.,0.707106781186563,-0.707106781186532));
#33046=DIRECTION('center_axis',(0.,0.,1.));
#33047=DIRECTION('ref_axis',(0.,1.,0.));
#33048=DIRECTION('',(0.,0.707106781186566,0.707106781186529));
#33049=DIRECTION('center_axis',(0.,0.,-1.));
#33050=DIRECTION('ref_axis',(0.,1.,0.));
#33051=DIRECTION('center_axis',(0.,-0.707106781186529,0.707106781186566));
#33052=DIRECTION('ref_axis',(1.,0.,0.));
#33053=DIRECTION('',(0.,0.707106781186566,0.707106781186529));
#33054=DIRECTION('',(1.,0.,0.));
#33055=DIRECTION('center_axis',(0.,0.,1.));
#33056=DIRECTION('ref_axis',(0.,-1.,0.));
#33057=DIRECTION('center_axis',(0.,0.,-1.));
#33058=DIRECTION('ref_axis',(0.,1.,0.));
#33059=DIRECTION('',(0.,0.,-1.));
#33060=DIRECTION('center_axis',(0.,0.707106781186529,-0.707106781186566));
#33061=DIRECTION('ref_axis',(-1.,0.,0.));
#33062=DIRECTION('',(0.,-0.707106781186566,-0.707106781186529));
#33063=DIRECTION('',(0.,0.707106781186563,0.707106781186532));
#33064=DIRECTION('',(1.,0.,0.));
#33065=DIRECTION('center_axis',(0.,0.,-1.));
#33066=DIRECTION('ref_axis',(0.,-1.,0.));
#33067=DIRECTION('',(0.,0.707106781186563,-0.707106781186532));
#33068=DIRECTION('center_axis',(0.,0.,1.));
#33069=DIRECTION('ref_axis',(0.,-1.,0.));
#33070=DIRECTION('center_axis',(0.,-0.707106781186532,-0.707106781186563));
#33071=DIRECTION('ref_axis',(-1.,0.,0.));
#33072=DIRECTION('',(0.,0.707106781186563,-0.707106781186532));
#33073=DIRECTION('',(-1.,0.,0.));
#33074=DIRECTION('center_axis',(0.,0.,-1.));
#33075=DIRECTION('ref_axis',(0.,1.,0.));
#33076=DIRECTION('center_axis',(0.,0.,1.));
#33077=DIRECTION('ref_axis',(0.,1.,0.));
#33078=DIRECTION('center_axis',(0.,0.,-1.));
#33079=DIRECTION('ref_axis',(0.,-1.,0.));
#33080=DIRECTION('',(0.,0.,-1.));
#33081=DIRECTION('center_axis',(0.,0.,-1.));
#33082=DIRECTION('ref_axis',(0.,-1.,0.));
#33083=DIRECTION('',(0.,0.,-1.));
#33084=DIRECTION('center_axis',(0.,-1.,0.));
#33085=DIRECTION('ref_axis',(-1.,0.,0.));
#33086=DIRECTION('',(0.,0.,-1.));
#33087=DIRECTION('',(-1.,0.,0.));
#33088=DIRECTION('center_axis',(0.,0.707106781186529,0.707106781186566));
#33089=DIRECTION('ref_axis',(1.,0.,0.));
#33090=DIRECTION('',(0.,-0.707106781186563,0.707106781186532));
#33091=DIRECTION('',(0.,0.707106781186566,-0.707106781186529));
#33092=DIRECTION('center_axis',(0.,0.,1.));
#33093=DIRECTION('ref_axis',(0.,1.,0.));
#33094=DIRECTION('',(0.,0.707106781186566,0.707106781186529));
#33095=DIRECTION('center_axis',(0.,0.,-1.));
#33096=DIRECTION('ref_axis',(0.,1.,0.));
#33097=DIRECTION('center_axis',(0.,-0.707106781186532,0.707106781186563));
#33098=DIRECTION('ref_axis',(1.,0.,0.));
#33099=DIRECTION('',(0.,0.707106781186563,0.707106781186532));
#33100=DIRECTION('',(1.,0.,0.));
#33101=DIRECTION('center_axis',(0.,0.,1.));
#33102=DIRECTION('ref_axis',(0.,-1.,0.));
#33103=DIRECTION('center_axis',(0.,0.,-1.));
#33104=DIRECTION('ref_axis',(0.,1.,0.));
#33105=DIRECTION('',(0.,0.,-1.));
#33106=DIRECTION('center_axis',(0.,1.,0.));
#33107=DIRECTION('ref_axis',(1.,0.,0.));
#33108=DIRECTION('center_axis',(0.,1.,0.));
#33109=DIRECTION('ref_axis',(1.,0.,0.));
#33110=DIRECTION('center_axis',(0.,-1.,0.));
#33111=DIRECTION('ref_axis',(0.,0.,-1.));
#33112=DIRECTION('center_axis',(0.707106781186566,0.707106781186529,0.));
#33113=DIRECTION('ref_axis',(0.,0.,-1.));
#33114=DIRECTION('center_axis',(0.,1.,0.));
#33115=DIRECTION('ref_axis',(0.,0.,1.));
#33116=DIRECTION('center_axis',(0.,0.,-1.));
#33117=DIRECTION('ref_axis',(0.,1.,0.));
#33118=DIRECTION('axis',(0.,0.,1.));
#33119=DIRECTION('refdir',(1.,0.,0.));
#33120=DIRECTION('center_axis',(0.,0.707106781186548,0.707106781186548));
#33121=DIRECTION('ref_axis',(1.,0.,0.));
#33122=DIRECTION('',(-0.577350269189605,0.577350269189636,-0.577350269189636));
#33123=DIRECTION('',(-1.,0.,0.));
#33124=DIRECTION('',(-0.577350269189605,-0.577350269189636,0.577350269189636));
#33125=DIRECTION('',(0.577350269189598,-0.577350269189639,0.577350269189639));
#33126=DIRECTION('',(1.,0.,0.));
#33127=DIRECTION('',(0.577350269189598,0.577350269189639,-0.577350269189639));
#33128=DIRECTION('center_axis',(-0.707106781186566,0.707106781186529,0.));
#33129=DIRECTION('ref_axis',(0.,0.,1.));
#33130=DIRECTION('',(0.,0.,-1.));
#33131=DIRECTION('',(0.577350269189602,0.577350269189633,0.577350269189643));
#33132=DIRECTION('',(-0.577350269189602,-0.577350269189633,0.577350269189643));
#33133=DIRECTION('',(0.,0.,1.));
#33134=DIRECTION('',(0.577350269189602,0.577350269189633,0.577350269189643));
#33135=DIRECTION('center_axis',(0.,1.,0.));
#33136=DIRECTION('ref_axis',(0.,0.,1.));
#33137=DIRECTION('',(0.,0.,1.));
#33138=DIRECTION('',(1.,0.,0.));
#33139=DIRECTION('center_axis',(0.707106781186566,0.707106781186529,0.));
#33140=DIRECTION('ref_axis',(0.,0.,-1.));
#33141=DIRECTION('',(-0.577350269189602,0.577350269189633,0.577350269189643));
#33142=DIRECTION('',(0.,0.,-1.));
#33143=DIRECTION('',(-0.577350269189602,0.577350269189633,-0.577350269189643));
#33144=DIRECTION('',(0.577350269189602,-0.577350269189633,-0.577350269189643));
#33145=DIRECTION('center_axis',(0.,0.707106781186554,-0.707106781186541));
#33146=DIRECTION('ref_axis',(-1.,0.,0.));
#33147=DIRECTION('',(-0.577350269189602,-0.577350269189633,-0.577350269189643));
#33148=DIRECTION('',(-1.,0.,0.));
#33149=DIRECTION('',(-0.577350269189602,0.577350269189633,0.577350269189643));
#33150=DIRECTION('center_axis',(0.,0.707106781186554,0.707106781186541));
#33151=DIRECTION('ref_axis',(1.,0.,0.));
#33152=DIRECTION('',(-0.577350269189602,0.577350269189633,-0.577350269189643));
#33153=DIRECTION('',(-1.,0.,0.));
#33154=DIRECTION('',(-0.577350269189602,-0.577350269189633,0.577350269189643));
#33155=DIRECTION('',(0.577350269189602,-0.577350269189633,0.577350269189643));
#33156=DIRECTION('',(1.,0.,0.));
#33157=DIRECTION('',(0.577350269189602,0.577350269189633,-0.577350269189643));
#33158=DIRECTION('center_axis',(-0.707106781186573,0.,0.707106781186522));
#33159=DIRECTION('ref_axis',(0.707106781186522,0.,0.707106781186573));
#33160=DIRECTION('',(0.577350269189602,0.577350269189633,0.577350269189643));
#33161=DIRECTION('',(0.,-1.,0.));
#33162=DIRECTION('',(0.577350269189602,-0.577350269189633,0.577350269189643));
#33163=DIRECTION('',(-0.577350269189588,-0.57735026918966,-0.577350269189629));
#33164=DIRECTION('',(0.,1.,0.));
#33165=DIRECTION('center_axis',(-0.707106781186566,0.707106781186529,0.));
#33166=DIRECTION('ref_axis',(0.,0.,1.));
#33167=DIRECTION('',(0.,0.,-1.));
#33168=DIRECTION('',(0.577350269189602,0.577350269189633,0.577350269189643));
#33169=DIRECTION('',(0.,0.,1.));
#33170=DIRECTION('center_axis',(0.,1.,0.));
#33171=DIRECTION('ref_axis',(0.,0.,1.));
#33172=DIRECTION('',(0.,0.,1.));
#33173=DIRECTION('',(1.,0.,0.));
#33174=DIRECTION('center_axis',(0.,1.,0.));
#33175=DIRECTION('ref_axis',(1.,0.,0.));
#33176=DIRECTION('center_axis',(0.,1.,0.));
#33177=DIRECTION('ref_axis',(1.,0.,0.));
#33178=DIRECTION('center_axis',(0.,-0.707106781186554,-0.707106781186541));
#33179=DIRECTION('ref_axis',(-1.,0.,0.));
#33180=DIRECTION('',(-0.577350269189602,-0.577350269189633,0.577350269189643));
#33181=DIRECTION('',(-1.,0.,0.));
#33182=DIRECTION('',(-0.577350269189602,0.577350269189633,-0.577350269189643));
#33183=DIRECTION('',(0.577350269189602,0.577350269189633,-0.577350269189643));
#33184=DIRECTION('',(1.,0.,0.));
#33185=DIRECTION('',(0.577350269189602,-0.577350269189633,0.577350269189643));
#33186=DIRECTION('center_axis',(-0.707106781186566,-0.707106781186529,0.));
#33187=DIRECTION('ref_axis',(0.,0.,1.));
#33188=DIRECTION('',(0.,0.,1.));
#33189=DIRECTION('',(0.577350269189616,-0.577350269189646,-0.577350269189616));
#33190=DIRECTION('',(0.,0.,-1.));
#33191=DIRECTION('',(0.577350269189602,-0.577350269189633,-0.577350269189643));
#33192=DIRECTION('center_axis',(0.,-1.,0.));
#33193=DIRECTION('ref_axis',(0.,0.,-1.));
#33194=DIRECTION('',(0.,0.,-1.));
#33195=DIRECTION('',(1.,0.,0.));
#33196=DIRECTION('center_axis',(0.,-1.,0.));
#33197=DIRECTION('ref_axis',(1.,0.,0.));
#33198=DIRECTION('center_axis',(0.,-1.,0.));
#33199=DIRECTION('ref_axis',(1.,0.,0.));
#33200=DIRECTION('center_axis',(0.707106781186566,-0.707106781186529,0.));
#33201=DIRECTION('ref_axis',(0.,0.,-1.));
#33202=DIRECTION('',(-0.577350269189602,-0.577350269189633,-0.577350269189643));
#33203=DIRECTION('',(0.,0.,1.));
#33204=DIRECTION('',(-0.577350269189602,-0.577350269189633,0.577350269189643));
#33205=DIRECTION('',(0.577350269189616,0.577350269189646,0.577350269189616));
#33206=DIRECTION('center_axis',(0.,-0.707106781186529,0.707106781186566));
#33207=DIRECTION('ref_axis',(1.,0.,0.));
#33208=DIRECTION('',(-0.577350269189588,0.57735026918966,0.577350269189629));
#33209=DIRECTION('',(-1.,0.,0.));
#33210=DIRECTION('center_axis',(0.707106781186573,0.,0.707106781186522));
#33211=DIRECTION('ref_axis',(0.707106781186522,0.,-0.707106781186573));
#33212=DIRECTION('',(0.,-1.,0.));
#33213=DIRECTION('',(0.,1.,0.));
#33214=DIRECTION('',(-0.577350269189602,0.577350269189633,0.577350269189643));
#33215=DIRECTION('center_axis',(0.,1.,0.));
#33216=DIRECTION('ref_axis',(1.,0.,0.));
#33217=DIRECTION('',(0.707106781186554,-0.707106781186541,-8.65956056235501E-17));
#33218=DIRECTION('center_axis',(0.,-1.,0.));
#33219=DIRECTION('ref_axis',(1.,0.,0.));
#33220=DIRECTION('center_axis',(0.,1.,0.));
#33221=DIRECTION('ref_axis',(1.,0.,0.));
#33222=DIRECTION('center_axis',(0.,1.,0.));
#33223=DIRECTION('ref_axis',(1.,0.,0.));
#33224=DIRECTION('',(0.,1.,0.));
#33225=DIRECTION('center_axis',(0.,-1.,0.));
#33226=DIRECTION('ref_axis',(1.,0.,0.));
#33227=DIRECTION('',(0.707106781186554,0.707106781186541,8.65956056235501E-17));
#33228=DIRECTION('center_axis',(0.,1.,0.));
#33229=DIRECTION('ref_axis',(1.,0.,0.));
#33230=DIRECTION('',(0.707106781186554,-0.707106781186541,-8.65956056235501E-17));
#33231=DIRECTION('center_axis',(0.,-1.,0.));
#33232=DIRECTION('ref_axis',(1.,0.,0.));
#33233=DIRECTION('center_axis',(0.,1.,0.));
#33234=DIRECTION('ref_axis',(1.,0.,0.));
#33235=DIRECTION('center_axis',(0.,1.,0.));
#33236=DIRECTION('ref_axis',(1.,0.,0.));
#33237=DIRECTION('',(0.,1.,0.));
#33238=DIRECTION('center_axis',(0.,-1.,0.));
#33239=DIRECTION('ref_axis',(1.,0.,0.));
#33240=DIRECTION('',(0.707106781186554,0.707106781186541,8.65956056235501E-17));
#33241=DIRECTION('center_axis',(0.707106781186566,0.707106781186529,0.));
#33242=DIRECTION('ref_axis',(0.,0.,-1.));
#33243=DIRECTION('',(0.,0.,-1.));
#33244=DIRECTION('',(-0.577350269189602,0.577350269189633,0.577350269189643));
#33245=DIRECTION('center_axis',(0.707106781186573,0.,0.707106781186522));
#33246=DIRECTION('ref_axis',(0.707106781186522,0.,-0.707106781186573));
#33247=DIRECTION('',(0.,-1.,0.));
#33248=DIRECTION('',(0.,1.,0.));
#33249=DIRECTION('center_axis',(0.707106781186573,0.,-0.707106781186522));
#33250=DIRECTION('ref_axis',(-0.707106781186522,0.,-0.707106781186573));
#33251=DIRECTION('',(0.,-1.,0.));
#33252=DIRECTION('',(0.,1.,0.));
#33253=DIRECTION('center_axis',(0.,0.,1.));
#33254=DIRECTION('ref_axis',(0.,-1.,0.));
#33255=DIRECTION('center_axis',(1.,0.,0.));
#33256=DIRECTION('ref_axis',(0.,0.,-1.));
#33257=DIRECTION('center_axis',(-0.707106781186573,0.,-0.707106781186522));
#33258=DIRECTION('ref_axis',(-0.707106781186522,0.,0.707106781186573));
#33259=DIRECTION('',(0.,-1.,0.));
#33260=DIRECTION('',(0.,1.,0.));
#33261=DIRECTION('center_axis',(-0.707106781186573,0.,0.707106781186522));
#33262=DIRECTION('ref_axis',(0.707106781186522,0.,0.707106781186573));
#33263=DIRECTION('',(0.,-1.,0.));
#33264=DIRECTION('',(0.,1.,0.));
#33265=DIRECTION('center_axis',(0.,0.,-1.));
#33266=DIRECTION('ref_axis',(0.,1.,0.));
#33267=DIRECTION('center_axis',(1.,0.,0.));
#33268=DIRECTION('ref_axis',(0.,0.,-1.));
#33269=DIRECTION('center_axis',(0.,0.,1.));
#33270=DIRECTION('ref_axis',(0.,-1.,0.));
#33271=DIRECTION('axis',(0.,0.,1.));
#33272=DIRECTION('refdir',(1.,0.,0.));
#33273=DIRECTION('center_axis',(0.,0.,-1.));
#33274=DIRECTION('ref_axis',(-0.707106781186547,-0.707106781186547,0.));
#33275=DIRECTION('',(-0.92387953251128,0.,-0.382683432365106));
#33276=DIRECTION('center_axis',(0.,0.,1.));
#33277=DIRECTION('ref_axis',(-0.707106781186547,-0.707106781186547,0.));
#33278=DIRECTION('',(0.,0.92387953251128,0.382683432365106));
#33279=DIRECTION('center_axis',(0.,0.,-1.));
#33280=DIRECTION('ref_axis',(-0.707106781186547,-0.707106781186547,0.));
#33281=DIRECTION('center_axis',(-0.382683432365179,0.,0.92387953251125));
#33282=DIRECTION('ref_axis',(0.92387953251125,0.,0.382683432365179));
#33283=DIRECTION('',(-0.923879532511251,0.,-0.382683432365176));
#33284=DIRECTION('',(0.,-1.,0.));
#33285=DIRECTION('',(0.,1.,0.));
#33286=DIRECTION('center_axis',(0.,0.,-1.));
#33287=DIRECTION('ref_axis',(-0.707106781186547,0.707106781186547,0.));
#33288=DIRECTION('',(0.,0.923879532511307,-0.382683432365041));
#33289=DIRECTION('center_axis',(0.,0.,1.));
#33290=DIRECTION('ref_axis',(-0.707106781186547,0.707106781186547,0.));
#33291=DIRECTION('center_axis',(0.,0.,-1.));
#33292=DIRECTION('ref_axis',(-0.707106781186547,0.707106781186547,0.));
#33293=DIRECTION('center_axis',(0.,0.382683432365181,0.923879532511249));
#33294=DIRECTION('ref_axis',(1.,0.,0.));
#33295=DIRECTION('',(0.,0.923879532511251,-0.382683432365176));
#33296=DIRECTION('',(-1.,0.,0.));
#33297=DIRECTION('',(1.,0.,0.));
#33298=DIRECTION('center_axis',(0.,0.,-1.));
#33299=DIRECTION('ref_axis',(0.707106781186547,0.707106781186547,0.));
#33300=DIRECTION('',(0.92387953251128,0.,-0.382683432365106));
#33301=DIRECTION('center_axis',(0.,0.,1.));
#33302=DIRECTION('ref_axis',(0.707106781186547,0.707106781186547,0.));
#33303=DIRECTION('center_axis',(0.,0.,-1.));
#33304=DIRECTION('ref_axis',(0.707106781186547,0.707106781186547,0.));
#33305=DIRECTION('center_axis',(0.382683432365179,0.,0.92387953251125));
#33306=DIRECTION('ref_axis',(0.92387953251125,0.,-0.382683432365179));
#33307=DIRECTION('',(0.923879532511251,0.,-0.382683432365176));
#33308=DIRECTION('',(0.,1.,0.));
#33309=DIRECTION('',(0.,-1.,0.));
#33310=DIRECTION('center_axis',(0.,0.,-1.));
#33311=DIRECTION('ref_axis',(0.707106781186547,-0.707106781186547,0.));
#33312=DIRECTION('',(0.,-0.92387953251128,-0.382683432365106));
#33313=DIRECTION('center_axis',(0.,0.,1.));
#33314=DIRECTION('ref_axis',(0.707106781186547,-0.707106781186547,0.));
#33315=DIRECTION('center_axis',(0.,0.,-1.));
#33316=DIRECTION('ref_axis',(0.707106781186547,-0.707106781186547,0.));
#33317=DIRECTION('center_axis',(0.,-0.382683432365179,0.92387953251125));
#33318=DIRECTION('ref_axis',(1.,0.,0.));
#33319=DIRECTION('',(1.,0.,0.));
#33320=DIRECTION('',(-1.,0.,0.));
#33321=DIRECTION('center_axis',(0.70710678118656,0.,0.707106781186535));
#33322=DIRECTION('ref_axis',(0.707106781186535,0.,-0.70710678118656));
#33323=DIRECTION('',(0.707106781186535,0.,-0.70710678118656));
#33324=DIRECTION('',(0.,-1.,0.));
#33325=DIRECTION('',(0.707106781186552,0.,-0.707106781186543));
#33326=DIRECTION('center_axis',(0.,0.,-1.));
#33327=DIRECTION('ref_axis',(0.707106781186548,-0.707106781186548,0.));
#33328=DIRECTION('',(0.,-0.707106781186552,-0.707106781186543));
#33329=DIRECTION('center_axis',(0.,0.,-1.));
#33330=DIRECTION('ref_axis',(0.707106781186548,-0.707106781186548,0.));
#33331=DIRECTION('center_axis',(0.,-0.70710678118656,0.707106781186535));
#33332=DIRECTION('ref_axis',(1.,0.,0.));
#33333=DIRECTION('',(0.,0.707106781186552,0.707106781186543));
#33334=DIRECTION('',(-1.,0.,0.));
#33335=DIRECTION('center_axis',(0.,0.,-1.));
#33336=DIRECTION('ref_axis',(-0.707106781186548,-0.707106781186548,0.));
#33337=DIRECTION('',(-0.707106781186552,0.,-0.707106781186543));
#33338=DIRECTION('center_axis',(0.,0.,-1.));
#33339=DIRECTION('ref_axis',(-0.707106781186548,-0.707106781186548,0.));
#33340=DIRECTION('center_axis',(0.,0.,1.));
#33341=DIRECTION('ref_axis',(1.,0.,0.));
#33342=DIRECTION('center_axis',(0.,0.,1.));
#33343=DIRECTION('ref_axis',(1.,0.,0.));
#33344=DIRECTION('center_axis',(0.,0.,-1.));
#33345=DIRECTION('ref_axis',(1.,0.,0.));
#33346=DIRECTION('center_axis',(0.,0.,-1.));
#33347=DIRECTION('ref_axis',(1.,0.,0.));
#33348=DIRECTION('center_axis',(0.490712016224176,-0.871321821793305,0.));
#33349=DIRECTION('ref_axis',(0.,0.,-1.));
#33350=DIRECTION('',(0.871321821793305,0.490712016224176,0.));
#33351=DIRECTION('',(0.,0.,-1.));
#33352=DIRECTION('',(-0.871321821793305,-0.490712016224176,0.));
#33353=DIRECTION('',(0.,0.,1.));
#33354=DIRECTION('center_axis',(0.,0.,1.));
#33355=DIRECTION('ref_axis',(-1.,1.22464679914735E-16,0.));
#33356=DIRECTION('center_axis',(0.,0.,1.));
#33357=DIRECTION('ref_axis',(1.,0.,0.));
#33358=DIRECTION('',(0.,0.,1.));
#33359=DIRECTION('center_axis',(0.,0.,1.));
#33360=DIRECTION('ref_axis',(1.,0.,0.));
#33361=DIRECTION('center_axis',(0.490712016224176,0.871321821793305,0.));
#33362=DIRECTION('ref_axis',(0.,0.,1.));
#33363=DIRECTION('',(0.871321821793305,-0.490712016224176,0.));
#33364=DIRECTION('',(-0.871321821793305,0.490712016224176,0.));
#33365=DIRECTION('',(0.,0.,-1.));
#33366=DIRECTION('center_axis',(0.,-0.923879532511285,0.382683432365094));
#33367=DIRECTION('ref_axis',(0.,-0.382683432365094,-0.923879532511285));
#33368=DIRECTION('',(0.,0.382683432365069,0.923879532511296));
#33369=DIRECTION('',(0.,-0.382683432365069,-0.923879532511296));
#33370=DIRECTION('',(1.,0.,0.));
#33371=DIRECTION('center_axis',(0.,0.,-1.));
#33372=DIRECTION('ref_axis',(0.707106781186548,-0.707106781186548,0.));
#33373=DIRECTION('',(-0.38268343236511,0.,0.923879532511279));
#33374=DIRECTION('center_axis',(0.,0.,1.));
#33375=DIRECTION('ref_axis',(0.707106781186548,-0.707106781186548,0.));
#33376=DIRECTION('center_axis',(0.923879532511285,0.,0.382683432365094));
#33377=DIRECTION('ref_axis',(0.382683432365094,0.,-0.923879532511285));
#33378=DIRECTION('',(-0.382683432365069,0.,0.923879532511296));
#33379=DIRECTION('',(0.,1.,0.));
#33380=DIRECTION('center_axis',(0.,0.,-1.));
#33381=DIRECTION('ref_axis',(0.707106781186548,0.707106781186547,0.));
#33382=DIRECTION('',(0.,-0.382683432365139,0.923879532511267));
#33383=DIRECTION('center_axis',(0.,0.,-1.));
#33384=DIRECTION('ref_axis',(0.707106781186548,0.707106781186547,0.));
#33385=DIRECTION('center_axis',(0.,0.,1.));
#33386=DIRECTION('ref_axis',(0.707106781186548,0.707106781186548,0.));
#33387=DIRECTION('center_axis',(0.,0.923879532511284,0.382683432365098));
#33388=DIRECTION('ref_axis',(0.,-0.382683432365098,0.923879532511284));
#33389=DIRECTION('',(0.,-0.382683432365073,0.923879532511294));
#33390=DIRECTION('',(1.,0.,0.));
#33391=DIRECTION('',(-1.,0.,0.));
#33392=DIRECTION('center_axis',(0.,0.,-1.));
#33393=DIRECTION('ref_axis',(-0.707106781186548,0.707106781186547,0.));
#33394=DIRECTION('',(0.382683432365135,0.,0.923879532511268));
#33395=DIRECTION('center_axis',(0.,0.,-1.));
#33396=DIRECTION('ref_axis',(-0.707106781186548,0.707106781186547,0.));
#33397=DIRECTION('center_axis',(0.,0.,1.));
#33398=DIRECTION('ref_axis',(-0.707106781186548,0.707106781186548,0.));
#33399=DIRECTION('center_axis',(-0.923879532511285,0.,0.382683432365094));
#33400=DIRECTION('ref_axis',(0.382683432365094,0.,0.923879532511285));
#33401=DIRECTION('',(0.382683432365069,0.,0.923879532511296));
#33402=DIRECTION('',(0.,1.,0.));
#33403=DIRECTION('',(0.,-1.,0.));
#33404=DIRECTION('center_axis',(0.,0.,-1.));
#33405=DIRECTION('ref_axis',(-0.707106781186548,-0.707106781186548,0.));
#33406=DIRECTION('center_axis',(0.,0.,1.));
#33407=DIRECTION('ref_axis',(-0.707106781186548,-0.707106781186548,0.));
#33408=DIRECTION('center_axis',(0.,0.,1.));
#33409=DIRECTION('ref_axis',(0.707106781186548,0.707106781186548,0.));
#33410=DIRECTION('',(0.,0.,-1.));
#33411=DIRECTION('center_axis',(0.,0.,-1.));
#33412=DIRECTION('ref_axis',(0.707106781186548,0.707106781186548,0.));
#33413=DIRECTION('',(0.,0.,1.));
#33414=DIRECTION('center_axis',(1.,0.,0.));
#33415=DIRECTION('ref_axis',(0.,1.,0.));
#33416=DIRECTION('',(0.,0.,1.));
#33417=DIRECTION('',(0.,-1.,0.));
#33418=DIRECTION('center_axis',(0.,0.,1.));
#33419=DIRECTION('ref_axis',(0.707106781186548,-0.707106781186548,0.));
#33420=DIRECTION('',(0.,0.,-1.));
#33421=DIRECTION('center_axis',(0.,0.,-1.));
#33422=DIRECTION('ref_axis',(0.707106781186548,-0.707106781186548,0.));
#33423=DIRECTION('center_axis',(0.,-1.,0.));
#33424=DIRECTION('ref_axis',(1.,0.,0.));
#33425=DIRECTION('',(0.,0.,1.));
#33426=DIRECTION('',(-1.,0.,0.));
#33427=DIRECTION('center_axis',(0.,-1.,0.));
#33428=DIRECTION('ref_axis',(0.,0.,1.));
#33429=DIRECTION('center_axis',(0.,0.,-1.));
#33430=DIRECTION('ref_axis',(-0.707106781186548,0.707106781186548,0.));
#33431=DIRECTION('',(0.,0.70710678118655,-0.707106781186545));
#33432=DIRECTION('',(-0.707106781186535,0.,-0.70710678118656));
#33433=DIRECTION('center_axis',(-0.70710678118656,0.,0.707106781186535));
#33434=DIRECTION('ref_axis',(0.707106781186535,0.,0.70710678118656));
#33435=DIRECTION('center_axis',(0.707106781186541,0.707106781186554,0.));
#33436=DIRECTION('ref_axis',(0.,0.,-1.));
#33437=DIRECTION('',(-0.707106781186554,0.707106781186541,0.));
#33438=DIRECTION('',(0.,0.,1.));
#33439=DIRECTION('',(0.707106781186554,-0.707106781186541,0.));
#33440=DIRECTION('',(0.,0.,-1.));
#33441=DIRECTION('center_axis',(0.,-1.,0.));
#33442=DIRECTION('ref_axis',(0.707106781186547,0.,0.707106781186547));
#33443=DIRECTION('',(0.,-0.707106781186667,0.707106781186428));
#33444=DIRECTION('center_axis',(0.,1.,0.));
#33445=DIRECTION('ref_axis',(0.707106781186548,0.,0.707106781186548));
#33446=DIRECTION('center_axis',(0.,-1.,0.));
#33447=DIRECTION('ref_axis',(0.707106781186548,0.,0.707106781186548));
#33448=DIRECTION('center_axis',(0.,0.707106781186529,0.707106781186566));
#33449=DIRECTION('ref_axis',(1.,0.,0.));
#33450=DIRECTION('',(0.,-0.707106781186566,0.707106781186529));
#33451=DIRECTION('',(1.,0.,0.));
#33452=DIRECTION('',(-1.,0.,0.));
#33453=DIRECTION('center_axis',(0.,-1.,0.));
#33454=DIRECTION('ref_axis',(-0.707106781186547,0.,0.707106781186547));
#33455=DIRECTION('',(-0.707106781186504,-0.707106781186592,0.));
#33456=DIRECTION('center_axis',(0.,1.,0.));
#33457=DIRECTION('ref_axis',(-0.707106781186548,0.,0.707106781186548));
#33458=DIRECTION('center_axis',(0.,-1.,0.));
#33459=DIRECTION('ref_axis',(-0.707106781186548,0.,0.707106781186548));
#33460=DIRECTION('center_axis',(-0.707106781186548,0.707106781186548,0.));
#33461=DIRECTION('ref_axis',(0.,0.,1.));
#33462=DIRECTION('',(-0.707106781186548,-0.707106781186548,0.));
#33463=DIRECTION('',(0.,0.,1.));
#33464=DIRECTION('',(0.,0.,-1.));
#33465=DIRECTION('center_axis',(0.,0.,1.));
#33466=DIRECTION('ref_axis',(1.,0.,0.));
#33467=DIRECTION('',(-1.,0.,0.));
#33468=DIRECTION('center_axis',(0.,0.,-1.));
#33469=DIRECTION('ref_axis',(1.,0.,0.));
#33470=DIRECTION('',(0.,-1.,0.));
#33471=DIRECTION('center_axis',(0.,1.,0.));
#33472=DIRECTION('ref_axis',(-1.,0.,0.));
#33473=DIRECTION('',(-1.,0.,0.));
#33474=DIRECTION('',(1.,0.,0.));
#33475=DIRECTION('center_axis',(-0.707106781186548,-0.707106781186548,0.));
#33476=DIRECTION('ref_axis',(0.,0.,1.));
#33477=DIRECTION('',(-0.707106781186548,0.707106781186548,0.));
#33478=DIRECTION('',(0.,0.,1.));
#33479=DIRECTION('',(-0.707106781186548,0.707106781186548,0.));
#33480=DIRECTION('',(0.,0.,-1.));
#33481=DIRECTION('center_axis',(0.,1.,0.));
#33482=DIRECTION('ref_axis',(-0.707106781186547,0.,0.707106781186547));
#33483=DIRECTION('',(0.,0.707106781186667,0.707106781186428));
#33484=DIRECTION('center_axis',(0.,-1.,0.));
#33485=DIRECTION('ref_axis',(-0.707106781186548,0.,0.707106781186548));
#33486=DIRECTION('center_axis',(0.,1.,0.));
#33487=DIRECTION('ref_axis',(-0.707106781186548,0.,0.707106781186548));
#33488=DIRECTION('center_axis',(0.,-0.707106781186529,0.707106781186566));
#33489=DIRECTION('ref_axis',(1.,0.,0.));
#33490=DIRECTION('',(0.,0.707106781186566,0.707106781186529));
#33491=DIRECTION('',(-1.,0.,0.));
#33492=DIRECTION('',(1.,0.,0.));
#33493=DIRECTION('center_axis',(0.,1.,0.));
#33494=DIRECTION('ref_axis',(0.707106781186547,0.,0.707106781186547));
#33495=DIRECTION('',(0.70710678118651,0.707106781186585,0.));
#33496=DIRECTION('center_axis',(0.,-1.,0.));
#33497=DIRECTION('ref_axis',(0.707106781186548,0.,0.707106781186548));
#33498=DIRECTION('center_axis',(0.,1.,0.));
#33499=DIRECTION('ref_axis',(0.707106781186548,0.,0.707106781186548));
#33500=DIRECTION('center_axis',(0.707106781186548,-0.707106781186548,0.));
#33501=DIRECTION('ref_axis',(0.,0.,-1.));
#33502=DIRECTION('',(-0.707106781186548,-0.707106781186548,0.));
#33503=DIRECTION('',(0.,0.,1.));
#33504=DIRECTION('',(0.,0.,-1.));
#33505=DIRECTION('center_axis',(0.,-1.,0.));
#33506=DIRECTION('ref_axis',(1.,0.,0.));
#33507=DIRECTION('',(-1.,0.,0.));
#33508=DIRECTION('center_axis',(0.,1.,0.));
#33509=DIRECTION('ref_axis',(1.,0.,0.));
#33510=DIRECTION('center_axis',(0.707106781186541,0.707106781186554,0.));
#33511=DIRECTION('ref_axis',(0.,0.,-1.));
#33512=DIRECTION('',(0.707106781186554,-0.707106781186541,0.));
#33513=DIRECTION('',(0.,0.,1.));
#33514=DIRECTION('',(0.707106781186554,-0.707106781186541,0.));
#33515=DIRECTION('',(0.,0.,-1.));
#33516=DIRECTION('center_axis',(0.,-1.,0.));
#33517=DIRECTION('ref_axis',(0.707106781186547,0.,0.707106781186547));
#33518=DIRECTION('',(0.,-0.707106781186667,0.707106781186428));
#33519=DIRECTION('center_axis',(0.,1.,0.));
#33520=DIRECTION('ref_axis',(0.707106781186548,0.,0.707106781186548));
#33521=DIRECTION('center_axis',(0.,-1.,0.));
#33522=DIRECTION('ref_axis',(0.707106781186548,0.,0.707106781186548));
#33523=DIRECTION('center_axis',(0.,0.707106781186529,0.707106781186566));
#33524=DIRECTION('ref_axis',(1.,0.,0.));
#33525=DIRECTION('',(0.,-0.707106781186566,0.707106781186529));
#33526=DIRECTION('',(1.,0.,0.));
#33527=DIRECTION('',(-1.,0.,0.));
#33528=DIRECTION('center_axis',(0.,-1.,0.));
#33529=DIRECTION('ref_axis',(-0.707106781186547,0.,0.707106781186547));
#33530=DIRECTION('',(-0.707106781186504,-0.707106781186592,0.));
#33531=DIRECTION('center_axis',(0.,1.,0.));
#33532=DIRECTION('ref_axis',(-0.707106781186548,0.,0.707106781186548));
#33533=DIRECTION('center_axis',(0.,-1.,0.));
#33534=DIRECTION('ref_axis',(-0.707106781186548,0.,0.707106781186548));
#33535=DIRECTION('center_axis',(-0.707106781186554,0.707106781186541,0.));
#33536=DIRECTION('ref_axis',(0.,0.,1.));
#33537=DIRECTION('',(0.707106781186541,0.707106781186554,0.));
#33538=DIRECTION('',(0.,0.,1.));
#33539=DIRECTION('',(0.,0.,-1.));
#33540=DIRECTION('center_axis',(0.,1.,0.));
#33541=DIRECTION('ref_axis',(-1.,0.,0.));
#33542=DIRECTION('',(1.,0.,0.));
#33543=DIRECTION('center_axis',(0.,-1.,0.));
#33544=DIRECTION('ref_axis',(1.,0.,0.));
#33545=DIRECTION('center_axis',(-0.707106781186548,-0.707106781186548,0.));
#33546=DIRECTION('ref_axis',(0.,0.,1.));
#33547=DIRECTION('',(0.707106781186548,-0.707106781186548,0.));
#33548=DIRECTION('',(0.,0.,1.));
#33549=DIRECTION('',(-0.707106781186548,0.707106781186548,0.));
#33550=DIRECTION('',(0.,0.,-1.));
#33551=DIRECTION('center_axis',(0.,1.,0.));
#33552=DIRECTION('ref_axis',(-0.707106781186547,0.,0.707106781186547));
#33553=DIRECTION('',(0.,0.707106781186667,0.707106781186428));
#33554=DIRECTION('center_axis',(0.,-1.,0.));
#33555=DIRECTION('ref_axis',(-0.707106781186548,0.,0.707106781186548));
#33556=DIRECTION('center_axis',(0.,1.,0.));
#33557=DIRECTION('ref_axis',(-0.707106781186548,0.,0.707106781186548));
#33558=DIRECTION('center_axis',(0.,-0.707106781186529,0.707106781186566));
#33559=DIRECTION('ref_axis',(1.,0.,0.));
#33560=DIRECTION('',(0.,0.707106781186566,0.707106781186529));
#33561=DIRECTION('',(-1.,0.,0.));
#33562=DIRECTION('',(1.,0.,0.));
#33563=DIRECTION('center_axis',(0.,1.,0.));
#33564=DIRECTION('ref_axis',(0.707106781186547,0.,0.707106781186547));
#33565=DIRECTION('',(0.70710678118651,0.707106781186585,0.));
#33566=DIRECTION('center_axis',(0.,-1.,0.));
#33567=DIRECTION('ref_axis',(0.707106781186548,0.,0.707106781186548));
#33568=DIRECTION('center_axis',(0.,1.,0.));
#33569=DIRECTION('ref_axis',(0.707106781186548,0.,0.707106781186548));
#33570=DIRECTION('center_axis',(0.707106781186548,-0.707106781186548,0.));
#33571=DIRECTION('ref_axis',(0.,0.,-1.));
#33572=DIRECTION('',(0.707106781186548,0.707106781186548,0.));
#33573=DIRECTION('',(0.,0.,1.));
#33574=DIRECTION('',(0.,0.,-1.));
#33575=DIRECTION('center_axis',(-1.,0.,0.));
#33576=DIRECTION('ref_axis',(0.,-1.,0.));
#33577=DIRECTION('',(0.,1.,0.));
#33578=DIRECTION('',(0.,-1.,0.));
#33579=DIRECTION('',(0.,-1.,0.));
#33580=DIRECTION('center_axis',(0.,-1.,0.));
#33581=DIRECTION('ref_axis',(-0.707106781186548,0.,0.707106781186548));
#33582=DIRECTION('',(0.,1.,0.));
#33583=DIRECTION('center_axis',(0.,0.,1.));
#33584=DIRECTION('ref_axis',(1.,0.,0.));
#33585=DIRECTION('',(0.,-1.,0.));
#33586=DIRECTION('center_axis',(0.,1.,0.));
#33587=DIRECTION('ref_axis',(0.707106781186548,0.,0.707106781186548));
#33588=DIRECTION('',(0.,1.,0.));
#33589=DIRECTION('center_axis',(1.,0.,0.));
#33590=DIRECTION('ref_axis',(0.,1.,0.));
#33591=DIRECTION('',(0.,1.,0.));
#33592=DIRECTION('',(0.,-1.,0.));
#33593=DIRECTION('center_axis',(0.,0.,1.));
#33594=DIRECTION('ref_axis',(1.,0.,0.));
#33595=DIRECTION('',(1.,0.,0.));
#33596=DIRECTION('center_axis',(0.,0.,-1.));
#33597=DIRECTION('ref_axis',(1.,0.,0.));
#33598=DIRECTION('center_axis',(0.,0.,-1.));
#33599=DIRECTION('ref_axis',(1.,0.,0.));
#33600=DIRECTION('center_axis',(0.,0.,-1.));
#33601=DIRECTION('ref_axis',(1.,0.,0.));
#33602=DIRECTION('',(-0.707106781186566,-8.65956056235516E-17,-0.707106781186529));
#33603=DIRECTION('center_axis',(0.,0.,1.));
#33604=DIRECTION('ref_axis',(1.,0.,0.));
#33605=DIRECTION('center_axis',(0.,0.,1.));
#33606=DIRECTION('ref_axis',(1.,0.,0.));
#33607=DIRECTION('center_axis',(0.,0.,1.));
#33608=DIRECTION('ref_axis',(1.,0.,0.));
#33609=DIRECTION('center_axis',(0.,0.,1.));
#33610=DIRECTION('ref_axis',(1.,0.,0.));
#33611=DIRECTION('',(0.,0.,-1.));
#33612=DIRECTION('center_axis',(0.,0.,1.));
#33613=DIRECTION('ref_axis',(1.,0.,0.));
#33614=DIRECTION('',(0.707106781186566,8.65956056235517E-17,-0.707106781186529));
#33615=DIRECTION('center_axis',(0.,0.,-1.));
#33616=DIRECTION('ref_axis',(1.,0.,0.));
#33617=DIRECTION('center_axis',(0.,0.,1.));
#33618=DIRECTION('ref_axis',(1.,0.,0.));
#33619=DIRECTION('center_axis',(0.,0.,1.));
#33620=DIRECTION('ref_axis',(1.,0.,0.));
#33621=DIRECTION('',(0.,0.,1.));
#33622=DIRECTION('center_axis',(0.,-1.,0.));
#33623=DIRECTION('ref_axis',(0.,0.,1.));
#33624=DIRECTION('',(-8.6595605623547E-17,0.707106781186566,0.707106781186529));
#33625=DIRECTION('center_axis',(0.,1.,0.));
#33626=DIRECTION('ref_axis',(0.,0.,1.));
#33627=DIRECTION('center_axis',(0.,1.,0.));
#33628=DIRECTION('ref_axis',(0.,0.,1.));
#33629=DIRECTION('',(0.,1.,0.));
#33630=DIRECTION('center_axis',(0.,1.,0.));
#33631=DIRECTION('ref_axis',(1.,0.,0.));
#33632=DIRECTION('center_axis',(0.,-1.,0.));
#33633=DIRECTION('ref_axis',(0.,0.,1.));
#33634=DIRECTION('',(1.04972719113862E-16,0.515038074910053,0.857167300702113));
#33635=DIRECTION('center_axis',(0.,0.,1.));
#33636=DIRECTION('ref_axis',(1.,0.,0.));
#33637=DIRECTION('',(-0.857167300702114,-1.04972719113862E-16,0.515038074910051));
#33638=DIRECTION('center_axis',(0.,1.,0.));
#33639=DIRECTION('ref_axis',(1.,0.,0.));
#33640=DIRECTION('',(0.,-1.,0.));
#33641=DIRECTION('center_axis',(0.,-1.,0.));
#33642=DIRECTION('ref_axis',(-0.707106781186548,0.,0.707106781186548));
#33643=DIRECTION('',(0.,-1.,0.));
#33644=DIRECTION('',(0.,1.,0.));
#33645=DIRECTION('center_axis',(0.,0.,1.));
#33646=DIRECTION('ref_axis',(1.,0.,0.));
#33647=DIRECTION('',(0.,-1.,0.));
#33648=DIRECTION('center_axis',(0.,1.,0.));
#33649=DIRECTION('ref_axis',(0.707106781186548,0.,0.707106781186548));
#33650=DIRECTION('',(0.,1.,0.));
#33651=DIRECTION('center_axis',(0.,0.,1.));
#33652=DIRECTION('ref_axis',(1.,0.,0.));
#33653=DIRECTION('',(0.,1.,0.));
#33654=DIRECTION('center_axis',(0.,0.,-1.));
#33655=DIRECTION('ref_axis',(1.,0.,0.));
#33656=DIRECTION('center_axis',(1.,0.,0.));
#33657=DIRECTION('ref_axis',(0.,1.,0.));
#33658=DIRECTION('',(0.,-1.,0.));
#33659=DIRECTION('center_axis',(-1.,0.,0.));
#33660=DIRECTION('ref_axis',(0.,-1.,0.));
#33661=DIRECTION('',(0.,1.,0.));
#33662=DIRECTION('center_axis',(0.,0.,1.));
#33663=DIRECTION('ref_axis',(1.,0.,0.));
#33664=DIRECTION('center_axis',(0.,0.,-1.));
#33665=DIRECTION('ref_axis',(1.,0.,0.));
#33666=DIRECTION('center_axis',(0.,0.,1.));
#33667=DIRECTION('ref_axis',(1.,0.,0.));
#33668=DIRECTION('center_axis',(0.,0.,-1.));
#33669=DIRECTION('ref_axis',(1.,0.,0.));
#33670=DIRECTION('',(1.,0.,0.));
#33671=DIRECTION('center_axis',(0.,-1.,0.));
#33672=DIRECTION('ref_axis',(1.,0.,0.));
#33673=DIRECTION('',(-1.,0.,0.));
#33674=DIRECTION('center_axis',(0.,0.,1.));
#33675=DIRECTION('ref_axis',(1.,0.,0.));
#33676=DIRECTION('center_axis',(0.,0.,-1.));
#33677=DIRECTION('ref_axis',(1.,0.,0.));
#33678=DIRECTION('center_axis',(0.,0.,1.));
#33679=DIRECTION('ref_axis',(1.,0.,0.));
#33680=DIRECTION('center_axis',(0.,0.,-1.));
#33681=DIRECTION('ref_axis',(1.,0.,0.));
#33682=DIRECTION('center_axis',(0.,0.,-1.));
#33683=DIRECTION('ref_axis',(1.,0.,0.));
#33684=DIRECTION('center_axis',(0.,0.,-1.));
#33685=DIRECTION('ref_axis',(1.,0.,0.));
#33686=DIRECTION('center_axis',(0.,0.,-1.));
#33687=DIRECTION('ref_axis',(1.,0.,0.));
#33688=DIRECTION('',(-0.707106781186535,-8.65956056235478E-17,-0.70710678118656));
#33689=DIRECTION('center_axis',(0.,0.,1.));
#33690=DIRECTION('ref_axis',(1.,0.,0.));
#33691=DIRECTION('center_axis',(0.,0.,1.));
#33692=DIRECTION('ref_axis',(1.,0.,0.));
#33693=DIRECTION('',(0.,0.,-1.));
#33694=DIRECTION('center_axis',(0.,0.,1.));
#33695=DIRECTION('ref_axis',(1.,0.,0.));
#33696=DIRECTION('center_axis',(0.,0.,1.));
#33697=DIRECTION('ref_axis',(1.,0.,0.));
#33698=DIRECTION('',(0.707106781186568,8.65956056235518E-17,-0.707106781186527));
#33699=DIRECTION('center_axis',(0.,0.,-1.));
#33700=DIRECTION('ref_axis',(1.,0.,0.));
#33701=DIRECTION('center_axis',(0.,0.,1.));
#33702=DIRECTION('ref_axis',(1.,0.,0.));
#33703=DIRECTION('center_axis',(0.,0.,1.));
#33704=DIRECTION('ref_axis',(1.,0.,0.));
#33705=DIRECTION('',(0.,0.,1.));
#33706=DIRECTION('center_axis',(0.,0.,1.));
#33707=DIRECTION('ref_axis',(1.,0.,0.));
#33708=DIRECTION('center_axis',(0.,0.,1.));
#33709=DIRECTION('ref_axis',(1.,0.,0.));
#33710=DIRECTION('center_axis',(0.,0.,1.));
#33711=DIRECTION('ref_axis',(1.,0.,0.));
#33712=DIRECTION('center_axis',(0.,0.,1.));
#33713=DIRECTION('ref_axis',(1.,0.,0.));
#33714=DIRECTION('center_axis',(0.,0.,-1.));
#33715=DIRECTION('ref_axis',(-1.,0.,0.));
#33716=DIRECTION('center_axis',(0.,0.,-1.));
#33717=DIRECTION('ref_axis',(1.,0.,0.));
#33718=DIRECTION('center_axis',(0.,0.,-1.));
#33719=DIRECTION('ref_axis',(-1.,0.,0.));
#33720=DIRECTION('center_axis',(0.,0.,-1.));
#33721=DIRECTION('ref_axis',(-1.,0.,0.));
#33722=DIRECTION('center_axis',(0.,0.,-1.));
#33723=DIRECTION('ref_axis',(1.,0.,0.));
#33724=DIRECTION('center_axis',(-1.22464679914735E-16,-1.,0.));
#33725=DIRECTION('ref_axis',(1.,-1.22464679914735E-16,0.));
#33726=DIRECTION('center_axis',(0.,0.,-1.));
#33727=DIRECTION('ref_axis',(1.,0.,0.));
#33728=DIRECTION('center_axis',(0.,0.,1.));
#33729=DIRECTION('ref_axis',(1.,0.,0.));
#33730=DIRECTION('center_axis',(0.,0.,1.));
#33731=DIRECTION('ref_axis',(1.,0.,0.));
#33732=DIRECTION('',(0.,0.,-1.));
#33733=DIRECTION('center_axis',(0.,0.,-1.));
#33734=DIRECTION('ref_axis',(-1.,0.,0.));
#33735=DIRECTION('center_axis',(0.,0.,1.));
#33736=DIRECTION('ref_axis',(1.,0.,0.));
#33737=DIRECTION('center_axis',(0.,0.,1.));
#33738=DIRECTION('ref_axis',(1.,0.,0.));
#33739=DIRECTION('center_axis',(0.,0.,1.));
#33740=DIRECTION('ref_axis',(1.,0.,0.));
#33741=DIRECTION('',(0.70710678118657,8.6595605623552E-17,-0.707106781186525));
#33742=DIRECTION('center_axis',(0.,0.,1.));
#33743=DIRECTION('ref_axis',(1.,0.,0.));
#33744=DIRECTION('center_axis',(0.,0.,1.));
#33745=DIRECTION('ref_axis',(1.,0.,0.));
#33746=DIRECTION('',(0.,0.,-1.));
#33747=DIRECTION('center_axis',(0.,0.,-1.));
#33748=DIRECTION('ref_axis',(1.,0.,0.));
#33749=DIRECTION('',(-0.70710678118657,-8.6595605623552E-17,-0.707106781186525));
#33750=DIRECTION('center_axis',(0.707106781186529,0.,-0.707106781186566));
#33751=DIRECTION('ref_axis',(-0.707106781186566,0.,-0.707106781186529));
#33752=DIRECTION('',(0.707106781186566,0.,0.707106781186529));
#33753=DIRECTION('',(-0.707106781186566,0.,-0.707106781186529));
#33754=DIRECTION('',(0.,1.,0.));
#33755=DIRECTION('center_axis',(0.,0.,1.));
#33756=DIRECTION('ref_axis',(0.707106781186547,0.707106781186547,0.));
#33757=DIRECTION('',(0.,0.707106781186566,0.707106781186529));
#33758=DIRECTION('center_axis',(0.,0.,1.));
#33759=DIRECTION('ref_axis',(0.707106781186548,0.707106781186548,0.));
#33760=DIRECTION('center_axis',(0.,0.707106781186529,-0.707106781186566));
#33761=DIRECTION('ref_axis',(-1.,0.,0.));
#33762=DIRECTION('',(0.,0.707106781186566,0.707106781186529));
#33763=DIRECTION('',(1.,0.,0.));
#33764=DIRECTION('',(-1.,0.,0.));
#33765=DIRECTION('center_axis',(0.,0.,1.));
#33766=DIRECTION('ref_axis',(-0.707106781186547,0.707106781186547,0.));
#33767=DIRECTION('',(-0.707106781186573,0.,0.707106781186522));
#33768=DIRECTION('center_axis',(0.,0.,-1.));
#33769=DIRECTION('ref_axis',(-0.707106781186548,0.707106781186548,0.));
#33770=DIRECTION('center_axis',(0.,0.,1.));
#33771=DIRECTION('ref_axis',(-0.707106781186548,0.707106781186548,0.));
#33772=DIRECTION('center_axis',(-0.707106781186529,0.,-0.707106781186566));
#33773=DIRECTION('ref_axis',(-0.707106781186566,0.,0.707106781186529));
#33774=DIRECTION('',(-0.707106781186566,0.,0.707106781186529));
#33775=DIRECTION('',(0.,1.,0.));
#33776=DIRECTION('',(0.,-1.,0.));
#33777=DIRECTION('center_axis',(0.,0.,1.));
#33778=DIRECTION('ref_axis',(-0.707106781186547,-0.707106781186547,0.));
#33779=DIRECTION('',(0.,-0.707106781186573,0.707106781186522));
#33780=DIRECTION('center_axis',(0.,0.,-1.));
#33781=DIRECTION('ref_axis',(-0.707106781186548,-0.707106781186548,0.));
#33782=DIRECTION('center_axis',(0.,0.,1.));
#33783=DIRECTION('ref_axis',(-0.707106781186548,-0.707106781186548,0.));
#33784=DIRECTION('center_axis',(0.,-0.707106781186529,-0.707106781186566));
#33785=DIRECTION('ref_axis',(-1.,0.,0.));
#33786=DIRECTION('',(0.,-0.707106781186566,0.707106781186529));
#33787=DIRECTION('',(1.,0.,0.));
#33788=DIRECTION('center_axis',(0.,0.,1.));
#33789=DIRECTION('ref_axis',(0.707106781186547,-0.707106781186547,0.));
#33790=DIRECTION('center_axis',(0.,0.,1.));
#33791=DIRECTION('ref_axis',(0.707106781186548,-0.707106781186548,0.));
#33792=DIRECTION('center_axis',(0.,0.,1.));
#33793=DIRECTION('ref_axis',(-0.707106781186548,-0.707106781186548,0.));
#33794=DIRECTION('',(0.,0.,-1.));
#33795=DIRECTION('center_axis',(0.,0.,1.));
#33796=DIRECTION('ref_axis',(1.,0.,0.));
#33797=DIRECTION('center_axis',(0.,0.707106781186561,0.707106781186534));
#33798=DIRECTION('ref_axis',(1.,0.,0.));
#33799=DIRECTION('',(0.,0.707106781186534,-0.707106781186561));
#33800=DIRECTION('center_axis',(0.,0.,-1.));
#33801=DIRECTION('ref_axis',(0.707106781186548,0.707106781186548,0.));
#33802=DIRECTION('center_axis',(-1.,0.,0.));
#33803=DIRECTION('ref_axis',(0.,-1.,0.));
#33804=DIRECTION('',(0.,0.,1.));
#33805=DIRECTION('center_axis',(0.,0.,1.));
#33806=DIRECTION('ref_axis',(-0.707106781186548,0.707106781186548,0.));
#33807=DIRECTION('',(0.,0.,-1.));
#33808=DIRECTION('center_axis',(0.,1.,0.));
#33809=DIRECTION('ref_axis',(-1.,0.,0.));
#33810=DIRECTION('axis',(0.,0.,1.));
#33811=DIRECTION('refdir',(1.,0.,0.));
#33812=DIRECTION('center_axis',(0.,0.,1.));
#33813=DIRECTION('ref_axis',(-0.532340283278114,0.846530461826022,0.));
#33814=DIRECTION('',(0.,0.,-1.));
#33815=DIRECTION('center_axis',(0.,0.,-1.));
#33816=DIRECTION('ref_axis',(1.,0.,0.));
#33817=DIRECTION('center_axis',(0.,0.,1.));
#33818=DIRECTION('ref_axis',(1.,0.,0.));
#33819=DIRECTION('',(0.,0.,-1.));
#33820=DIRECTION('center_axis',(0.,0.,1.));
#33821=DIRECTION('ref_axis',(1.,0.,0.));
#33822=DIRECTION('',(0.,0.,-1.));
#33823=DIRECTION('center_axis',(0.,0.,1.));
#33824=DIRECTION('ref_axis',(1.,0.,0.));
#33825=DIRECTION('',(0.,0.,-1.));
#33826=DIRECTION('center_axis',(0.,0.,1.));
#33827=DIRECTION('ref_axis',(1.,0.,0.));
#33828=DIRECTION('',(0.,0.,-1.));
#33829=DIRECTION('center_axis',(0.,0.,1.));
#33830=DIRECTION('ref_axis',(1.,0.,0.));
#33831=DIRECTION('center_axis',(0.,0.,1.));
#33832=DIRECTION('ref_axis',(0.409460327591604,-0.91232792357166,0.));
#33833=DIRECTION('',(0.,0.,1.));
#33834=DIRECTION('center_axis',(0.,0.,1.));
#33835=DIRECTION('ref_axis',(1.,-5.87495706799284E-15,0.));
#33836=DIRECTION('center_axis',(0.,0.,1.));
#33837=DIRECTION('ref_axis',(1.,-5.87495706799284E-15,0.));
#33838=DIRECTION('',(0.,0.,1.));
#33839=DIRECTION('center_axis',(0.,0.,1.));
#33840=DIRECTION('ref_axis',(1.,-5.87495706799284E-15,0.));
#33841=DIRECTION('',(0.,0.,1.));
#33842=DIRECTION('center_axis',(0.,0.,1.));
#33843=DIRECTION('ref_axis',(1.,-5.87495706799284E-15,0.));
#33844=DIRECTION('',(0.,0.,1.));
#33845=DIRECTION('center_axis',(-0.993575558391583,-0.113170710728767,0.));
#33846=DIRECTION('ref_axis',(-0.113170710728767,0.993575558391583,0.));
#33847=DIRECTION('',(0.,0.,1.));
#33848=DIRECTION('',(-0.113170710728767,0.993575558391583,0.));
#33849=DIRECTION('',(0.,0.,-1.));
#33850=DIRECTION('center_axis',(-0.398779068740344,0.917047029510801,0.));
#33851=DIRECTION('ref_axis',(0.917047029510801,0.398779068740344,0.));
#33852=DIRECTION('',(0.917047029510801,0.398779068740344,0.));
#33853=DIRECTION('',(0.,0.,-1.));
#33854=DIRECTION('center_axis',(0.,0.,-1.));
#33855=DIRECTION('ref_axis',(-1.,0.,0.));
#33856=DIRECTION('center_axis',(0.,0.,1.));
#33857=DIRECTION('ref_axis',(1.,0.,0.));
#33858=DIRECTION('center_axis',(-0.917047029510801,0.398779068740345,0.));
#33859=DIRECTION('ref_axis',(0.398779068740345,0.917047029510801,0.));
#33860=DIRECTION('',(0.,0.,1.));
#33861=DIRECTION('',(0.398779068740345,0.917047029510801,0.));
#33862=DIRECTION('',(0.,0.,-1.));
#33863=DIRECTION('center_axis',(0.113170710728767,0.993575558391583,0.));
#33864=DIRECTION('ref_axis',(0.993575558391583,-0.113170710728767,0.));
#33865=DIRECTION('',(0.993575558391583,-0.113170710728767,0.));
#33866=DIRECTION('',(0.,0.,-1.));
#33867=DIRECTION('center_axis',(0.,0.,-1.));
#33868=DIRECTION('ref_axis',(-1.,0.,0.));
#33869=DIRECTION('center_axis',(0.,0.,1.));
#33870=DIRECTION('ref_axis',(1.,0.,0.));
#33871=DIRECTION('center_axis',(-0.594796489651244,0.803876318782036,0.));
#33872=DIRECTION('ref_axis',(0.803876318782036,0.594796489651244,0.));
#33873=DIRECTION('',(0.,0.,1.));
#33874=DIRECTION('',(0.803876318782036,0.594796489651244,0.));
#33875=DIRECTION('',(0.,0.,-1.));
#33876=DIRECTION('center_axis',(0.594796489651239,0.803876318782039,0.));
#33877=DIRECTION('ref_axis',(0.803876318782039,-0.594796489651239,0.));
#33878=DIRECTION('',(0.803876318782039,-0.594796489651239,0.));
#33879=DIRECTION('',(0.,0.,-1.));
#33880=DIRECTION('center_axis',(0.,0.,-1.));
#33881=DIRECTION('ref_axis',(-1.,0.,0.));
#33882=DIRECTION('center_axis',(0.,0.,1.));
#33883=DIRECTION('ref_axis',(1.,0.,0.));
#33884=DIRECTION('center_axis',(-0.113170710728767,0.993575558391583,0.));
#33885=DIRECTION('ref_axis',(0.993575558391583,0.113170710728767,0.));
#33886=DIRECTION('',(0.,0.,1.));
#33887=DIRECTION('',(0.993575558391583,0.113170710728767,0.));
#33888=DIRECTION('',(0.,0.,-1.));
#33889=DIRECTION('center_axis',(0.917047029510801,0.398779068740344,0.));
#33890=DIRECTION('ref_axis',(0.398779068740344,-0.917047029510801,0.));
#33891=DIRECTION('',(0.398779068740344,-0.917047029510801,0.));
#33892=DIRECTION('',(0.,0.,-1.));
#33893=DIRECTION('center_axis',(0.,0.,-1.));
#33894=DIRECTION('ref_axis',(-1.,0.,0.));
#33895=DIRECTION('center_axis',(0.,0.,1.));
#33896=DIRECTION('ref_axis',(1.,0.,0.));
#33897=DIRECTION('center_axis',(0.398779068740341,0.917047029510803,0.));
#33898=DIRECTION('ref_axis',(0.917047029510803,-0.398779068740341,0.));
#33899=DIRECTION('',(0.,0.,1.));
#33900=DIRECTION('',(0.917047029510803,-0.398779068740341,0.));
#33901=DIRECTION('',(0.,0.,-1.));
#33902=DIRECTION('center_axis',(0.993575558391583,-0.113170710728765,0.));
#33903=DIRECTION('ref_axis',(-0.113170710728765,-0.993575558391583,0.));
#33904=DIRECTION('',(-0.113170710728765,-0.993575558391583,0.));
#33905=DIRECTION('',(0.,0.,-1.));
#33906=DIRECTION('center_axis',(0.,0.,-1.));
#33907=DIRECTION('ref_axis',(-1.,0.,0.));
#33908=DIRECTION('center_axis',(0.,0.,1.));
#33909=DIRECTION('ref_axis',(1.,0.,0.));
#33910=DIRECTION('center_axis',(0.803876318782038,0.594796489651242,0.));
#33911=DIRECTION('ref_axis',(0.594796489651242,-0.803876318782038,0.));
#33912=DIRECTION('',(0.,0.,1.));
#33913=DIRECTION('',(0.594796489651242,-0.803876318782038,0.));
#33914=DIRECTION('',(0.,0.,-1.));
#33915=DIRECTION('center_axis',(0.803876318782038,-0.594796489651242,0.));
#33916=DIRECTION('ref_axis',(-0.594796489651242,-0.803876318782038,0.));
#33917=DIRECTION('',(-0.594796489651242,-0.803876318782038,0.));
#33918=DIRECTION('',(0.,0.,-1.));
#33919=DIRECTION('center_axis',(0.,0.,-1.));
#33920=DIRECTION('ref_axis',(-1.,0.,0.));
#33921=DIRECTION('center_axis',(0.,0.,1.));
#33922=DIRECTION('ref_axis',(1.,0.,0.));
#33923=DIRECTION('center_axis',(0.,0.,1.));
#33924=DIRECTION('ref_axis',(1.,0.,0.));
#33925=DIRECTION('center_axis',(0.930429556935621,0.366470789532515,0.));
#33926=DIRECTION('ref_axis',(0.366470789532515,-0.930429556935621,0.));
#33927=DIRECTION('',(0.,0.,1.));
#33928=DIRECTION('',(0.366470789532515,-0.930429556935621,0.));
#33929=DIRECTION('',(0.,0.,-1.));
#33930=DIRECTION('center_axis',(0.622540237971889,-0.782587791947909,0.));
#33931=DIRECTION('ref_axis',(-0.782587791947909,-0.622540237971889,0.));
#33932=DIRECTION('',(-0.782587791947909,-0.622540237971889,0.));
#33933=DIRECTION('',(0.,0.,-1.));
#33934=DIRECTION('center_axis',(0.,0.,-1.));
#33935=DIRECTION('ref_axis',(-1.,0.,0.));
#33936=DIRECTION('center_axis',(0.,0.,1.));
#33937=DIRECTION('ref_axis',(1.,0.,0.));
#33938=DIRECTION('center_axis',(0.989011027504405,-0.147841764987712,0.));
#33939=DIRECTION('ref_axis',(-0.147841764987712,-0.989011027504405,0.));
#33940=DIRECTION('',(0.,0.,1.));
#33941=DIRECTION('',(-0.147841764987712,-0.989011027504405,0.));
#33942=DIRECTION('',(0.,0.,-1.));
#33943=DIRECTION('center_axis',(0.14784176498771,-0.989011027504405,0.));
#33944=DIRECTION('ref_axis',(-0.989011027504405,-0.14784176498771,0.));
#33945=DIRECTION('',(-0.989011027504405,-0.14784176498771,0.));
#33946=DIRECTION('',(0.,0.,-1.));
#33947=DIRECTION('center_axis',(0.,0.,-1.));
#33948=DIRECTION('ref_axis',(-1.,0.,0.));
#33949=DIRECTION('center_axis',(0.,0.,1.));
#33950=DIRECTION('ref_axis',(1.,0.,0.));
#33951=DIRECTION('center_axis',(0.782587791947909,-0.622540237971889,0.));
#33952=DIRECTION('ref_axis',(-0.622540237971889,-0.782587791947909,0.));
#33953=DIRECTION('',(0.,0.,1.));
#33954=DIRECTION('',(-0.622540237971889,-0.782587791947909,0.));
#33955=DIRECTION('',(0.,0.,-1.));
#33956=DIRECTION('center_axis',(-0.366470789532515,-0.930429556935621,0.));
#33957=DIRECTION('ref_axis',(-0.930429556935621,0.366470789532515,0.));
#33958=DIRECTION('',(-0.930429556935621,0.366470789532515,0.));
#33959=DIRECTION('',(0.,0.,-1.));
#33960=DIRECTION('center_axis',(0.,0.,-1.));
#33961=DIRECTION('ref_axis',(-1.,0.,0.));
#33962=DIRECTION('center_axis',(0.,0.,1.));
#33963=DIRECTION('ref_axis',(1.,0.,0.));
#33964=DIRECTION('center_axis',(0.366470789532517,-0.93042955693562,0.));
#33965=DIRECTION('ref_axis',(-0.93042955693562,-0.366470789532517,0.));
#33966=DIRECTION('',(0.,0.,1.));
#33967=DIRECTION('',(-0.93042955693562,-0.366470789532517,0.));
#33968=DIRECTION('',(0.,0.,-1.));
#33969=DIRECTION('center_axis',(-0.782587791947909,-0.622540237971889,0.));
#33970=DIRECTION('ref_axis',(-0.622540237971889,0.782587791947909,0.));
#33971=DIRECTION('',(-0.622540237971889,0.782587791947909,0.));
#33972=DIRECTION('',(0.,0.,-1.));
#33973=DIRECTION('center_axis',(0.,0.,-1.));
#33974=DIRECTION('ref_axis',(-1.,0.,0.));
#33975=DIRECTION('center_axis',(0.,0.,1.));
#33976=DIRECTION('ref_axis',(1.,0.,0.));
#33977=DIRECTION('center_axis',(-0.147841764987711,-0.989011027504405,0.));
#33978=DIRECTION('ref_axis',(-0.989011027504405,0.147841764987711,0.));
#33979=DIRECTION('',(0.,0.,1.));
#33980=DIRECTION('',(-0.989011027504405,0.147841764987711,0.));
#33981=DIRECTION('',(0.,0.,-1.));
#33982=DIRECTION('center_axis',(-0.989011027504405,-0.147841764987711,0.));
#33983=DIRECTION('ref_axis',(-0.147841764987711,0.989011027504405,0.));
#33984=DIRECTION('',(-0.147841764987711,0.989011027504405,0.));
#33985=DIRECTION('',(0.,0.,-1.));
#33986=DIRECTION('center_axis',(0.,0.,-1.));
#33987=DIRECTION('ref_axis',(-1.,0.,0.));
#33988=DIRECTION('center_axis',(0.,0.,1.));
#33989=DIRECTION('ref_axis',(1.,0.,0.));
#33990=DIRECTION('center_axis',(-0.622540237971888,-0.78258779194791,0.));
#33991=DIRECTION('ref_axis',(-0.78258779194791,0.622540237971888,0.));
#33992=DIRECTION('',(0.,0.,1.));
#33993=DIRECTION('',(-0.78258779194791,0.622540237971888,0.));
#33994=DIRECTION('',(0.,0.,-1.));
#33995=DIRECTION('center_axis',(-0.93042955693562,0.366470789532517,0.));
#33996=DIRECTION('ref_axis',(0.366470789532517,0.93042955693562,0.));
#33997=DIRECTION('',(0.366470789532517,0.93042955693562,0.));
#33998=DIRECTION('',(0.,0.,-1.));
#33999=DIRECTION('center_axis',(0.,0.,-1.));
#34000=DIRECTION('ref_axis',(-1.,0.,0.));
#34001=DIRECTION('center_axis',(0.,0.,1.));
#34002=DIRECTION('ref_axis',(1.,0.,0.));
#34003=DIRECTION('center_axis',(-0.398779068740341,-0.917047029510803,0.));
#34004=DIRECTION('ref_axis',(-0.917047029510803,0.398779068740341,0.));
#34005=DIRECTION('',(0.,0.,1.));
#34006=DIRECTION('',(-0.917047029510803,0.398779068740341,0.));
#34007=DIRECTION('',(0.,0.,-1.));
#34008=DIRECTION('center_axis',(-0.993575558391583,0.113170710728763,0.));
#34009=DIRECTION('ref_axis',(0.113170710728763,0.993575558391583,0.));
#34010=DIRECTION('',(0.113170710728763,0.993575558391583,0.));
#34011=DIRECTION('',(0.,0.,-1.));
#34012=DIRECTION('center_axis',(0.,0.,-1.));
#34013=DIRECTION('ref_axis',(-1.,0.,0.));
#34014=DIRECTION('center_axis',(0.,0.,1.));
#34015=DIRECTION('ref_axis',(1.,0.,0.));
#34016=DIRECTION('center_axis',(0.113170710728765,-0.993575558391583,0.));
#34017=DIRECTION('ref_axis',(-0.993575558391583,-0.113170710728765,0.));
#34018=DIRECTION('',(0.,0.,1.));
#34019=DIRECTION('',(-0.993575558391583,-0.113170710728765,0.));
#34020=DIRECTION('',(0.,0.,-1.));
#34021=DIRECTION('center_axis',(-0.917047029510802,-0.398779068740342,0.));
#34022=DIRECTION('ref_axis',(-0.398779068740342,0.917047029510802,0.));
#34023=DIRECTION('',(-0.398779068740342,0.917047029510802,0.));
#34024=DIRECTION('',(0.,0.,-1.));
#34025=DIRECTION('center_axis',(0.,0.,-1.));
#34026=DIRECTION('ref_axis',(-1.,0.,0.));
#34027=DIRECTION('center_axis',(0.,0.,1.));
#34028=DIRECTION('ref_axis',(1.,0.,0.));
#34029=DIRECTION('center_axis',(0.594796489651242,-0.803876318782038,0.));
#34030=DIRECTION('ref_axis',(-0.803876318782038,-0.594796489651242,0.));
#34031=DIRECTION('',(0.,0.,1.));
#34032=DIRECTION('',(-0.803876318782038,-0.594796489651242,0.));
#34033=DIRECTION('',(0.,0.,-1.));
#34034=DIRECTION('center_axis',(-0.594796489651242,-0.803876318782038,0.));
#34035=DIRECTION('ref_axis',(-0.803876318782038,0.594796489651242,0.));
#34036=DIRECTION('',(-0.803876318782038,0.594796489651242,0.));
#34037=DIRECTION('',(0.,0.,-1.));
#34038=DIRECTION('center_axis',(0.,0.,-1.));
#34039=DIRECTION('ref_axis',(-1.,0.,0.));
#34040=DIRECTION('center_axis',(0.,0.,1.));
#34041=DIRECTION('ref_axis',(1.,0.,0.));
#34042=DIRECTION('center_axis',(0.917047029510802,-0.398779068740341,0.));
#34043=DIRECTION('ref_axis',(-0.398779068740341,-0.917047029510802,0.));
#34044=DIRECTION('',(0.,0.,1.));
#34045=DIRECTION('',(-0.398779068740341,-0.917047029510802,0.));
#34046=DIRECTION('',(0.,0.,-1.));
#34047=DIRECTION('center_axis',(-0.113170710728766,-0.993575558391583,0.));
#34048=DIRECTION('ref_axis',(-0.993575558391583,0.113170710728766,0.));
#34049=DIRECTION('',(-0.993575558391583,0.113170710728766,0.));
#34050=DIRECTION('',(0.,0.,-1.));
#34051=DIRECTION('center_axis',(0.,0.,-1.));
#34052=DIRECTION('ref_axis',(-1.,0.,0.));
#34053=DIRECTION('center_axis',(0.,0.,1.));
#34054=DIRECTION('ref_axis',(1.,0.,0.));
#34055=DIRECTION('center_axis',(0.993575558391583,0.113170710728763,0.));
#34056=DIRECTION('ref_axis',(0.113170710728763,-0.993575558391583,0.));
#34057=DIRECTION('',(0.,0.,1.));
#34058=DIRECTION('',(0.113170710728763,-0.993575558391583,0.));
#34059=DIRECTION('',(0.,0.,-1.));
#34060=DIRECTION('center_axis',(0.398779068740342,-0.917047029510802,0.));
#34061=DIRECTION('ref_axis',(-0.917047029510802,-0.398779068740342,0.));
#34062=DIRECTION('',(-0.917047029510802,-0.398779068740342,0.));
#34063=DIRECTION('',(0.,0.,-1.));
#34064=DIRECTION('center_axis',(0.,0.,-1.));
#34065=DIRECTION('ref_axis',(-1.,0.,0.));
#34066=DIRECTION('center_axis',(0.,0.,1.));
#34067=DIRECTION('ref_axis',(1.,0.,0.));
#34068=DIRECTION('center_axis',(-0.803876318782038,-0.594796489651242,0.));
#34069=DIRECTION('ref_axis',(-0.594796489651242,0.803876318782038,0.));
#34070=DIRECTION('',(0.,0.,1.));
#34071=DIRECTION('',(-0.594796489651242,0.803876318782038,0.));
#34072=DIRECTION('',(0.,0.,-1.));
#34073=DIRECTION('center_axis',(-0.803876318782038,0.594796489651242,0.));
#34074=DIRECTION('ref_axis',(0.594796489651242,0.803876318782038,0.));
#34075=DIRECTION('',(0.594796489651242,0.803876318782038,0.));
#34076=DIRECTION('',(0.,0.,-1.));
#34077=DIRECTION('center_axis',(0.,0.,-1.));
#34078=DIRECTION('ref_axis',(-1.,0.,0.));
#34079=DIRECTION('center_axis',(0.,0.,1.));
#34080=DIRECTION('ref_axis',(1.,0.,0.));
#34081=DIRECTION('center_axis',(0.622540237971889,0.782587791947909,0.));
#34082=DIRECTION('ref_axis',(0.782587791947909,-0.622540237971889,0.));
#34083=DIRECTION('',(0.,0.,1.));
#34084=DIRECTION('',(0.782587791947909,-0.622540237971889,0.));
#34085=DIRECTION('',(0.,0.,-1.));
#34086=DIRECTION('center_axis',(0.93042955693562,-0.366470789532517,0.));
#34087=DIRECTION('ref_axis',(-0.366470789532517,-0.93042955693562,0.));
#34088=DIRECTION('',(-0.366470789532517,-0.93042955693562,0.));
#34089=DIRECTION('',(0.,0.,-1.));
#34090=DIRECTION('center_axis',(0.,0.,-1.));
#34091=DIRECTION('ref_axis',(-1.,0.,0.));
#34092=DIRECTION('center_axis',(0.,0.,1.));
#34093=DIRECTION('ref_axis',(1.,0.,0.));
#34094=DIRECTION('center_axis',(0.147841764987712,0.989011027504405,0.));
#34095=DIRECTION('ref_axis',(0.989011027504405,-0.147841764987712,0.));
#34096=DIRECTION('',(0.,0.,1.));
#34097=DIRECTION('',(0.989011027504405,-0.147841764987712,0.));
#34098=DIRECTION('',(0.,0.,-1.));
#34099=DIRECTION('center_axis',(0.989011027504404,0.147841764987713,0.));
#34100=DIRECTION('ref_axis',(0.147841764987713,-0.989011027504404,0.));
#34101=DIRECTION('',(0.147841764987713,-0.989011027504404,0.));
#34102=DIRECTION('',(0.,0.,-1.));
#34103=DIRECTION('center_axis',(0.,0.,-1.));
#34104=DIRECTION('ref_axis',(-1.,0.,0.));
#34105=DIRECTION('center_axis',(0.,0.,1.));
#34106=DIRECTION('ref_axis',(1.,0.,0.));
#34107=DIRECTION('center_axis',(-0.366470789532514,0.930429556935621,0.));
#34108=DIRECTION('ref_axis',(0.930429556935621,0.366470789532514,0.));
#34109=DIRECTION('',(0.,0.,1.));
#34110=DIRECTION('',(0.930429556935621,0.366470789532514,0.));
#34111=DIRECTION('',(0.,0.,-1.));
#34112=DIRECTION('center_axis',(0.782587791947912,0.622540237971886,0.));
#34113=DIRECTION('ref_axis',(0.622540237971886,-0.782587791947912,0.));
#34114=DIRECTION('',(0.622540237971886,-0.782587791947912,0.));
#34115=DIRECTION('',(0.,0.,-1.));
#34116=DIRECTION('center_axis',(0.,0.,-1.));
#34117=DIRECTION('ref_axis',(-1.,0.,0.));
#34118=DIRECTION('center_axis',(0.,0.,1.));
#34119=DIRECTION('ref_axis',(1.,0.,0.));
#34120=DIRECTION('center_axis',(-0.782587791947911,0.622540237971887,0.));
#34121=DIRECTION('ref_axis',(0.622540237971887,0.782587791947911,0.));
#34122=DIRECTION('',(0.,0.,1.));
#34123=DIRECTION('',(0.622540237971887,0.782587791947911,0.));
#34124=DIRECTION('',(0.,0.,-1.));
#34125=DIRECTION('center_axis',(0.366470789532514,0.930429556935621,0.));
#34126=DIRECTION('ref_axis',(0.930429556935621,-0.366470789532514,0.));
#34127=DIRECTION('',(0.930429556935621,-0.366470789532514,0.));
#34128=DIRECTION('',(0.,0.,-1.));
#34129=DIRECTION('center_axis',(0.,0.,-1.));
#34130=DIRECTION('ref_axis',(-1.,0.,0.));
#34131=DIRECTION('center_axis',(0.,0.,1.));
#34132=DIRECTION('ref_axis',(1.,0.,0.));
#34133=DIRECTION('center_axis',(-0.989011027504405,0.147841764987707,0.));
#34134=DIRECTION('ref_axis',(0.147841764987707,0.989011027504405,0.));
#34135=DIRECTION('',(0.,0.,1.));
#34136=DIRECTION('',(0.147841764987707,0.989011027504405,0.));
#34137=DIRECTION('',(0.,0.,-1.));
#34138=DIRECTION('center_axis',(-0.147841764987713,0.989011027504404,0.));
#34139=DIRECTION('ref_axis',(0.989011027504404,0.147841764987713,0.));
#34140=DIRECTION('',(0.989011027504404,0.147841764987713,0.));
#34141=DIRECTION('',(0.,0.,-1.));
#34142=DIRECTION('center_axis',(0.,0.,-1.));
#34143=DIRECTION('ref_axis',(-1.,0.,0.));
#34144=DIRECTION('center_axis',(0.,0.,1.));
#34145=DIRECTION('ref_axis',(1.,0.,0.));
#34146=DIRECTION('center_axis',(-0.930429556935621,-0.366470789532514,0.));
#34147=DIRECTION('ref_axis',(-0.366470789532514,0.930429556935621,0.));
#34148=DIRECTION('',(0.,0.,1.));
#34149=DIRECTION('',(-0.366470789532514,0.930429556935621,0.));
#34150=DIRECTION('',(0.,0.,-1.));
#34151=DIRECTION('center_axis',(-0.622540237971886,0.782587791947912,0.));
#34152=DIRECTION('ref_axis',(0.782587791947912,0.622540237971886,0.));
#34153=DIRECTION('',(0.782587791947912,0.622540237971886,0.));
#34154=DIRECTION('',(0.,0.,-1.));
#34155=DIRECTION('center_axis',(0.,0.,-1.));
#34156=DIRECTION('ref_axis',(-1.,0.,0.));
#34157=DIRECTION('center_axis',(0.,0.,1.));
#34158=DIRECTION('ref_axis',(1.,0.,0.));
#34159=DIRECTION('center_axis',(0.,0.,-1.));
#34160=DIRECTION('ref_axis',(1.,0.,0.));
#34161=DIRECTION('center_axis',(0.,0.,1.));
#34162=DIRECTION('ref_axis',(1.,0.,0.));
#34163=DIRECTION('',(-0.707106781186534,-8.65956056235477E-17,-0.707106781186561));
#34164=DIRECTION('center_axis',(0.,0.,1.));
#34165=DIRECTION('ref_axis',(1.,0.,0.));
#34166=DIRECTION('center_axis',(0.,0.,1.));
#34167=DIRECTION('ref_axis',(1.,0.,0.));
#34168=DIRECTION('center_axis',(0.,0.,1.));
#34169=DIRECTION('ref_axis',(1.,0.,0.));
#34170=DIRECTION('center_axis',(0.,0.,1.));
#34171=DIRECTION('ref_axis',(1.,0.,0.));
#34172=DIRECTION('center_axis',(0.,0.,1.));
#34173=DIRECTION('ref_axis',(1.,0.,0.));
#34174=DIRECTION('center_axis',(0.,0.,1.));
#34175=DIRECTION('ref_axis',(1.,0.,0.));
#34176=DIRECTION('center_axis',(0.,0.,1.));
#34177=DIRECTION('ref_axis',(1.,0.,0.));
#34178=DIRECTION('center_axis',(0.,0.,1.));
#34179=DIRECTION('ref_axis',(1.,0.,0.));
#34180=DIRECTION('center_axis',(0.,0.,1.));
#34181=DIRECTION('ref_axis',(1.,0.,0.));
#34182=DIRECTION('center_axis',(0.,0.,1.));
#34183=DIRECTION('ref_axis',(1.,0.,0.));
#34184=DIRECTION('center_axis',(0.,0.,1.));
#34185=DIRECTION('ref_axis',(1.,0.,0.));
#34186=DIRECTION('center_axis',(0.,0.,1.));
#34187=DIRECTION('ref_axis',(1.,0.,0.));
#34188=DIRECTION('center_axis',(0.,0.,1.));
#34189=DIRECTION('ref_axis',(1.,0.,0.));
#34190=DIRECTION('center_axis',(0.,0.,1.));
#34191=DIRECTION('ref_axis',(1.,0.,0.));
#34192=DIRECTION('center_axis',(0.,0.,1.));
#34193=DIRECTION('ref_axis',(1.,0.,0.));
#34194=DIRECTION('center_axis',(0.,0.,1.));
#34195=DIRECTION('ref_axis',(1.,0.,0.));
#34196=DIRECTION('center_axis',(0.,0.,1.));
#34197=DIRECTION('ref_axis',(1.,0.,0.));
#34198=DIRECTION('center_axis',(0.,0.,1.));
#34199=DIRECTION('ref_axis',(1.,0.,0.));
#34200=DIRECTION('center_axis',(0.,0.,1.));
#34201=DIRECTION('ref_axis',(1.,0.,0.));
#34202=DIRECTION('center_axis',(0.,0.,1.));
#34203=DIRECTION('ref_axis',(1.,0.,0.));
#34204=DIRECTION('center_axis',(0.,0.,1.));
#34205=DIRECTION('ref_axis',(1.,0.,0.));
#34206=DIRECTION('center_axis',(0.,0.,1.));
#34207=DIRECTION('ref_axis',(1.,0.,0.));
#34208=DIRECTION('center_axis',(0.,0.,1.));
#34209=DIRECTION('ref_axis',(1.,0.,0.));
#34210=DIRECTION('center_axis',(0.,0.,1.));
#34211=DIRECTION('ref_axis',(1.,0.,0.));
#34212=DIRECTION('center_axis',(0.,0.,1.));
#34213=DIRECTION('ref_axis',(1.,0.,0.));
#34214=DIRECTION('center_axis',(0.,0.,1.));
#34215=DIRECTION('ref_axis',(1.,0.,0.));
#34216=DIRECTION('center_axis',(0.,0.,1.));
#34217=DIRECTION('ref_axis',(1.,0.,0.));
#34218=DIRECTION('center_axis',(0.,0.,1.));
#34219=DIRECTION('ref_axis',(1.,0.,0.));
#34220=DIRECTION('center_axis',(0.,0.,1.));
#34221=DIRECTION('ref_axis',(1.,0.,0.));
#34222=DIRECTION('center_axis',(0.,0.,1.));
#34223=DIRECTION('ref_axis',(1.,0.,0.));
#34224=DIRECTION('center_axis',(0.,0.,1.));
#34225=DIRECTION('ref_axis',(1.,0.,0.));
#34226=DIRECTION('center_axis',(0.,0.,1.));
#34227=DIRECTION('ref_axis',(1.,0.,0.));
#34228=DIRECTION('center_axis',(0.,0.,1.));
#34229=DIRECTION('ref_axis',(1.,0.,0.));
#34230=DIRECTION('center_axis',(0.,0.,1.));
#34231=DIRECTION('ref_axis',(1.,0.,0.));
#34232=DIRECTION('center_axis',(0.,0.,1.));
#34233=DIRECTION('ref_axis',(1.,0.,0.));
#34234=DIRECTION('center_axis',(0.,0.,1.));
#34235=DIRECTION('ref_axis',(1.,0.,0.));
#34236=DIRECTION('center_axis',(0.,0.,1.));
#34237=DIRECTION('ref_axis',(1.,0.,0.));
#34238=DIRECTION('center_axis',(0.,0.,1.));
#34239=DIRECTION('ref_axis',(1.,0.,0.));
#34240=DIRECTION('center_axis',(0.,0.,1.));
#34241=DIRECTION('ref_axis',(1.,0.,0.));
#34242=DIRECTION('center_axis',(0.,0.,1.));
#34243=DIRECTION('ref_axis',(1.,0.,0.));
#34244=DIRECTION('center_axis',(0.,0.,1.));
#34245=DIRECTION('ref_axis',(1.,0.,0.));
#34246=DIRECTION('center_axis',(0.,0.,1.));
#34247=DIRECTION('ref_axis',(1.,0.,0.));
#34248=DIRECTION('center_axis',(0.,0.,1.));
#34249=DIRECTION('ref_axis',(1.,0.,0.));
#34250=DIRECTION('center_axis',(0.,0.,1.));
#34251=DIRECTION('ref_axis',(1.,0.,0.));
#34252=DIRECTION('center_axis',(0.,0.,1.));
#34253=DIRECTION('ref_axis',(1.,0.,0.));
#34254=DIRECTION('center_axis',(0.,0.,1.));
#34255=DIRECTION('ref_axis',(1.,0.,0.));
#34256=DIRECTION('center_axis',(0.,0.,1.));
#34257=DIRECTION('ref_axis',(1.,0.,0.));
#34258=DIRECTION('center_axis',(0.,0.,1.));
#34259=DIRECTION('ref_axis',(1.,0.,0.));
#34260=DIRECTION('center_axis',(0.,0.,1.));
#34261=DIRECTION('ref_axis',(1.,0.,0.));
#34262=DIRECTION('center_axis',(0.,0.,1.));
#34263=DIRECTION('ref_axis',(1.,0.,0.));
#34264=DIRECTION('center_axis',(0.,0.,1.));
#34265=DIRECTION('ref_axis',(1.,0.,0.));
#34266=DIRECTION('center_axis',(0.,0.,1.));
#34267=DIRECTION('ref_axis',(1.,0.,0.));
#34268=DIRECTION('center_axis',(0.,0.,1.));
#34269=DIRECTION('ref_axis',(1.,0.,0.));
#34270=DIRECTION('center_axis',(0.,0.,1.));
#34271=DIRECTION('ref_axis',(1.,0.,0.));
#34272=DIRECTION('center_axis',(0.,0.,1.));
#34273=DIRECTION('ref_axis',(1.,0.,0.));
#34274=DIRECTION('center_axis',(0.,0.,1.));
#34275=DIRECTION('ref_axis',(1.,0.,0.));
#34276=DIRECTION('center_axis',(0.,0.,1.));
#34277=DIRECTION('ref_axis',(1.,0.,0.));
#34278=DIRECTION('center_axis',(0.,0.,1.));
#34279=DIRECTION('ref_axis',(1.,0.,0.));
#34280=DIRECTION('center_axis',(0.,0.,1.));
#34281=DIRECTION('ref_axis',(1.,0.,0.));
#34282=DIRECTION('center_axis',(0.,0.,1.));
#34283=DIRECTION('ref_axis',(1.,0.,0.));
#34284=DIRECTION('center_axis',(0.,0.,1.));
#34285=DIRECTION('ref_axis',(1.,0.,0.));
#34286=DIRECTION('center_axis',(0.,0.,1.));
#34287=DIRECTION('ref_axis',(1.,0.,0.));
#34288=DIRECTION('center_axis',(0.,0.,1.));
#34289=DIRECTION('ref_axis',(1.,0.,0.));
#34290=DIRECTION('center_axis',(0.,0.,1.));
#34291=DIRECTION('ref_axis',(1.,0.,0.));
#34292=DIRECTION('center_axis',(0.,0.,1.));
#34293=DIRECTION('ref_axis',(1.,0.,0.));
#34294=DIRECTION('center_axis',(0.,0.,1.));
#34295=DIRECTION('ref_axis',(1.,0.,0.));
#34296=DIRECTION('center_axis',(0.,0.,1.));
#34297=DIRECTION('ref_axis',(1.,0.,0.));
#34298=DIRECTION('center_axis',(0.,0.,1.));
#34299=DIRECTION('ref_axis',(1.,0.,0.));
#34300=DIRECTION('center_axis',(0.,0.,1.));
#34301=DIRECTION('ref_axis',(1.,0.,0.));
#34302=DIRECTION('center_axis',(0.,0.,1.));
#34303=DIRECTION('ref_axis',(1.,0.,0.));
#34304=DIRECTION('center_axis',(0.,0.,1.));
#34305=DIRECTION('ref_axis',(1.,-5.87495706799284E-15,0.));
#34306=DIRECTION('center_axis',(0.,0.,-1.));
#34307=DIRECTION('ref_axis',(1.,-5.87495706799284E-15,0.));
#34308=DIRECTION('center_axis',(0.,0.,1.));
#34309=DIRECTION('ref_axis',(-0.944006790271089,-0.329926021892902,0.));
#34310=DIRECTION('center_axis',(0.,0.,1.));
#34311=DIRECTION('ref_axis',(1.,0.,0.));
#34312=DIRECTION('center_axis',(0.,0.,-1.));
#34313=DIRECTION('ref_axis',(-1.,0.,0.));
#34314=DIRECTION('center_axis',(0.,0.,1.));
#34315=DIRECTION('ref_axis',(1.,0.,0.));
#34316=DIRECTION('center_axis',(0.,0.,1.));
#34317=DIRECTION('ref_axis',(1.,0.,0.));
#34318=DIRECTION('center_axis',(0.,0.,1.));
#34319=DIRECTION('ref_axis',(1.,0.,0.));
#34320=DIRECTION('',(0.707106781186568,8.65956056235518E-17,-0.707106781186527));
#34321=DIRECTION('center_axis',(0.,0.,1.));
#34322=DIRECTION('ref_axis',(1.,0.,0.));
#34323=DIRECTION('center_axis',(0.,0.,1.));
#34324=DIRECTION('ref_axis',(1.,0.,0.));
#34325=DIRECTION('',(0.,0.,-1.));
#34326=DIRECTION('center_axis',(0.,0.,-1.));
#34327=DIRECTION('ref_axis',(1.,0.,0.));
#34328=DIRECTION('center_axis',(0.,0.,1.));
#34329=DIRECTION('ref_axis',(1.,0.,0.));
#34330=DIRECTION('',(-0.707106781186534,-8.65956056235477E-17,-0.707106781186561));
#34331=DIRECTION('center_axis',(0.,0.,1.));
#34332=DIRECTION('ref_axis',(1.,0.,0.));
#34333=DIRECTION('center_axis',(0.,0.,-1.));
#34334=DIRECTION('ref_axis',(-1.,0.,0.));
#34335=DIRECTION('center_axis',(0.,0.,1.));
#34336=DIRECTION('ref_axis',(1.,0.,0.));
#34337=DIRECTION('center_axis',(0.,0.,1.));
#34338=DIRECTION('ref_axis',(1.,0.,0.));
#34339=DIRECTION('center_axis',(0.,0.,1.));
#34340=DIRECTION('ref_axis',(1.,0.,0.));
#34341=DIRECTION('',(0.707106781186568,8.65956056235518E-17,-0.707106781186527));
#34342=DIRECTION('center_axis',(0.,0.,1.));
#34343=DIRECTION('ref_axis',(1.,0.,0.));
#34344=DIRECTION('center_axis',(0.,0.,1.));
#34345=DIRECTION('ref_axis',(1.,0.,0.));
#34346=DIRECTION('axis',(0.,0.,1.));
#34347=DIRECTION('refdir',(1.,0.,0.));
#34348=DIRECTION('center_axis',(0.,-1.,0.));
#34349=DIRECTION('ref_axis',(1.,0.,0.));
#34350=DIRECTION('',(0.,1.,0.));
#34351=DIRECTION('center_axis',(0.,-1.,0.));
#34352=DIRECTION('ref_axis',(1.,0.,0.));
#34353=DIRECTION('center_axis',(0.,-1.,0.));
#34354=DIRECTION('ref_axis',(1.,0.,0.));
#34355=DIRECTION('',(0.,1.,0.));
#34356=DIRECTION('center_axis',(0.,-1.,0.));
#34357=DIRECTION('ref_axis',(1.,0.,0.));
#34358=DIRECTION('',(0.,1.,0.));
#34359=DIRECTION('center_axis',(0.,-1.,0.));
#34360=DIRECTION('ref_axis',(1.,0.,0.));
#34361=DIRECTION('',(0.,1.,0.));
#34362=DIRECTION('center_axis',(0.,-1.,0.));
#34363=DIRECTION('ref_axis',(1.,0.,0.));
#34364=DIRECTION('',(0.,1.,0.));
#34365=DIRECTION('center_axis',(0.,-1.,0.));
#34366=DIRECTION('ref_axis',(1.,0.,0.));
#34367=DIRECTION('',(0.,1.,0.));
#34368=DIRECTION('center_axis',(0.,-1.,0.));
#34369=DIRECTION('ref_axis',(1.,0.,0.));
#34370=DIRECTION('',(0.,1.,0.));
#34371=DIRECTION('center_axis',(0.,-1.,0.));
#34372=DIRECTION('ref_axis',(1.,0.,0.));
#34373=DIRECTION('',(0.,1.,0.));
#34374=DIRECTION('center_axis',(0.,-1.,0.));
#34375=DIRECTION('ref_axis',(1.,0.,0.));
#34376=DIRECTION('',(0.,1.,0.));
#34377=DIRECTION('center_axis',(0.,-1.,0.));
#34378=DIRECTION('ref_axis',(1.,0.,0.));
#34379=DIRECTION('',(0.,1.,0.));
#34380=DIRECTION('center_axis',(0.,-1.,0.));
#34381=DIRECTION('ref_axis',(1.,0.,0.));
#34382=DIRECTION('',(0.,1.,0.));
#34383=DIRECTION('center_axis',(0.,-1.,0.));
#34384=DIRECTION('ref_axis',(1.,0.,0.));
#34385=DIRECTION('',(0.,1.,0.));
#34386=DIRECTION('center_axis',(0.,-1.,0.));
#34387=DIRECTION('ref_axis',(1.,0.,0.));
#34388=DIRECTION('',(0.,1.,0.));
#34389=DIRECTION('center_axis',(0.,-1.,0.));
#34390=DIRECTION('ref_axis',(1.,0.,0.));
#34391=DIRECTION('',(0.,1.,0.));
#34392=DIRECTION('center_axis',(0.,-1.,0.));
#34393=DIRECTION('ref_axis',(1.,0.,0.));
#34394=DIRECTION('',(0.,1.,0.));
#34395=DIRECTION('center_axis',(0.,-1.,0.));
#34396=DIRECTION('ref_axis',(1.,0.,8.81908600741727E-14));
#34397=DIRECTION('',(0.,-1.,0.));
#34398=DIRECTION('center_axis',(0.,-1.,0.));
#34399=DIRECTION('ref_axis',(1.,0.,8.81908600741727E-14));
#34400=DIRECTION('center_axis',(0.,-1.,0.));
#34401=DIRECTION('ref_axis',(1.,0.,8.81908600741727E-14));
#34402=DIRECTION('',(0.,-1.,0.));
#34403=DIRECTION('center_axis',(0.,-1.,0.));
#34404=DIRECTION('ref_axis',(1.,0.,8.81908600741727E-14));
#34405=DIRECTION('',(0.,-1.,0.));
#34406=DIRECTION('center_axis',(0.,-1.,0.));
#34407=DIRECTION('ref_axis',(1.,0.,8.81908600741727E-14));
#34408=DIRECTION('',(0.,-1.,0.));
#34409=DIRECTION('center_axis',(0.,-1.,0.));
#34410=DIRECTION('ref_axis',(1.,0.,8.81908600741727E-14));
#34411=DIRECTION('',(0.,-1.,0.));
#34412=DIRECTION('center_axis',(0.,-1.,0.));
#34413=DIRECTION('ref_axis',(1.,0.,8.81908600741727E-14));
#34414=DIRECTION('',(0.,-1.,0.));
#34415=DIRECTION('center_axis',(0.,-1.,0.));
#34416=DIRECTION('ref_axis',(1.,0.,8.81908600741727E-14));
#34417=DIRECTION('',(0.,-1.,0.));
#34418=DIRECTION('center_axis',(0.,-1.,0.));
#34419=DIRECTION('ref_axis',(1.,0.,8.81908600741727E-14));
#34420=DIRECTION('',(0.,-1.,0.));
#34421=DIRECTION('center_axis',(0.,-1.,0.));
#34422=DIRECTION('ref_axis',(1.,0.,8.81908600741727E-14));
#34423=DIRECTION('',(0.,-1.,0.));
#34424=DIRECTION('center_axis',(0.,-1.,0.));
#34425=DIRECTION('ref_axis',(1.,0.,8.81908600741727E-14));
#34426=DIRECTION('',(0.,-1.,0.));
#34427=DIRECTION('center_axis',(0.,-1.,0.));
#34428=DIRECTION('ref_axis',(1.,0.,8.81908600741727E-14));
#34429=DIRECTION('',(0.,-1.,0.));
#34430=DIRECTION('center_axis',(0.,-1.,0.));
#34431=DIRECTION('ref_axis',(1.,0.,8.81908600741727E-14));
#34432=DIRECTION('',(0.,-1.,0.));
#34433=DIRECTION('center_axis',(0.,-1.,0.));
#34434=DIRECTION('ref_axis',(1.,0.,8.81908600741727E-14));
#34435=DIRECTION('',(0.,-1.,0.));
#34436=DIRECTION('center_axis',(0.,-1.,0.));
#34437=DIRECTION('ref_axis',(1.,0.,8.81908600741727E-14));
#34438=DIRECTION('',(0.,-1.,0.));
#34439=DIRECTION('center_axis',(0.,-1.,0.));
#34440=DIRECTION('ref_axis',(1.,0.,8.81908600741727E-14));
#34441=DIRECTION('',(0.,-1.,0.));
#34442=DIRECTION('center_axis',(-0.0386781209882463,0.,0.999251721518066));
#34443=DIRECTION('ref_axis',(0.999251721518066,0.,0.0386781209882463));
#34444=DIRECTION('',(0.,1.,0.));
#34445=DIRECTION('',(0.999251721518066,0.,0.0386781209882463));
#34446=DIRECTION('',(0.,1.,0.));
#34447=DIRECTION('center_axis',(0.,1.,0.));
#34448=DIRECTION('ref_axis',(0.,0.,1.));
#34449=DIRECTION('center_axis',(0.,1.,0.));
#34450=DIRECTION('ref_axis',(1.,0.,0.));
#34451=DIRECTION('',(-0.135427727050936,0.,0.990787227786984));
#34452=DIRECTION('center_axis',(-0.990787227786984,0.,-0.135427727050936));
#34453=DIRECTION('ref_axis',(-0.135427727050936,0.,0.990787227786984));
#34454=DIRECTION('',(0.,-1.,0.));
#34455=DIRECTION('center_axis',(0.612677465896384,0.,0.790333045483222));
#34456=DIRECTION('ref_axis',(0.790333045483222,0.,-0.612677465896384));
#34457=DIRECTION('',(0.,1.,0.));
#34458=DIRECTION('',(0.790333045483222,0.,-0.612677465896384));
#34459=DIRECTION('',(0.,1.,0.));
#34460=DIRECTION('center_axis',(0.,1.,0.));
#34461=DIRECTION('ref_axis',(0.,0.,1.));
#34462=DIRECTION('center_axis',(0.,1.,0.));
#34463=DIRECTION('ref_axis',(1.,0.,0.));
#34464=DIRECTION('',(0.53312209610552,0.,0.846038315115844));
#34465=DIRECTION('center_axis',(-0.846038315115844,0.,0.53312209610552));
#34466=DIRECTION('ref_axis',(0.53312209610552,0.,0.846038315115844));
#34467=DIRECTION('',(0.,-1.,0.));
#34468=DIRECTION('center_axis',(0.97735445733659,0.,0.211608753893357));
#34469=DIRECTION('ref_axis',(0.211608753893357,0.,-0.97735445733659));
#34470=DIRECTION('',(0.,1.,0.));
#34471=DIRECTION('',(0.211608753893357,0.,-0.97735445733659));
#34472=DIRECTION('',(0.,1.,0.));
#34473=DIRECTION('center_axis',(0.,1.,0.));
#34474=DIRECTION('ref_axis',(0.,0.,1.));
#34475=DIRECTION('center_axis',(0.,1.,0.));
#34476=DIRECTION('ref_axis',(1.,0.,0.));
#34477=DIRECTION('',(0.952218165502102,0.,0.305418672133534));
#34478=DIRECTION('center_axis',(-0.305418672133534,0.,0.952218165502102));
#34479=DIRECTION('ref_axis',(0.952218165502102,0.,0.305418672133534));
#34480=DIRECTION('',(0.,-1.,0.));
#34481=DIRECTION('center_axis',(0.884716436104133,0.,-0.466129625412504));
#34482=DIRECTION('ref_axis',(-0.466129625412504,0.,-0.884716436104133));
#34483=DIRECTION('',(0.,1.,0.));
#34484=DIRECTION('',(-0.466129625412504,0.,-0.884716436104133));
#34485=DIRECTION('',(0.,1.,0.));
#34486=DIRECTION('center_axis',(0.,1.,0.));
#34487=DIRECTION('ref_axis',(0.,0.,1.));
#34488=DIRECTION('center_axis',(0.,1.,0.));
#34489=DIRECTION('ref_axis',(1.,0.,0.));
#34490=DIRECTION('',(0.92576077253418,0.,-0.378109761890538));
#34491=DIRECTION('center_axis',(0.378109761890538,0.,0.92576077253418));
#34492=DIRECTION('ref_axis',(0.92576077253418,0.,-0.378109761890538));
#34493=DIRECTION('',(0.,-1.,0.));
#34494=DIRECTION('center_axis',(-0.671935785203098,0.,0.740609411608775));
#34495=DIRECTION('ref_axis',(0.740609411608775,0.,0.671935785203098));
#34496=DIRECTION('',(0.,1.,0.));
#34497=DIRECTION('',(0.740609411608775,0.,0.671935785203098));
#34498=DIRECTION('',(0.,1.,0.));
#34499=DIRECTION('center_axis',(0.,1.,0.));
#34500=DIRECTION('ref_axis',(0.,0.,1.));
#34501=DIRECTION('center_axis',(0.,1.,0.));
#34502=DIRECTION('ref_axis',(1.,0.,0.));
#34503=DIRECTION('',(-0.740609411608775,0.,0.671935785203098));
#34504=DIRECTION('center_axis',(-0.671935785203098,0.,-0.740609411608775));
#34505=DIRECTION('ref_axis',(-0.740609411608775,0.,0.671935785203098));
#34506=DIRECTION('',(0.,-1.,0.));
#34507=DIRECTION('center_axis',(0.0386781209882463,0.,-0.999251721518066));
#34508=DIRECTION('ref_axis',(-0.999251721518066,0.,-0.0386781209882463));
#34509=DIRECTION('',(0.,1.,0.));
#34510=DIRECTION('',(-0.999251721518066,0.,-0.0386781209882463));
#34511=DIRECTION('',(0.,1.,0.));
#34512=DIRECTION('center_axis',(0.,1.,0.));
#34513=DIRECTION('ref_axis',(0.,0.,1.));
#34514=DIRECTION('center_axis',(0.,1.,0.));
#34515=DIRECTION('ref_axis',(1.,0.,0.));
#34516=DIRECTION('',(0.135427727050939,0.,-0.990787227786984));
#34517=DIRECTION('center_axis',(0.990787227786984,0.,0.135427727050939));
#34518=DIRECTION('ref_axis',(0.135427727050939,0.,-0.990787227786984));
#34519=DIRECTION('',(0.,-1.,0.));
#34520=DIRECTION('center_axis',(-0.612677465896387,0.,-0.79033304548322));
#34521=DIRECTION('ref_axis',(-0.79033304548322,0.,0.612677465896387));
#34522=DIRECTION('',(0.,1.,0.));
#34523=DIRECTION('',(-0.79033304548322,0.,0.612677465896387));
#34524=DIRECTION('',(0.,1.,0.));
#34525=DIRECTION('center_axis',(0.,1.,0.));
#34526=DIRECTION('ref_axis',(0.,0.,1.));
#34527=DIRECTION('center_axis',(0.,1.,0.));
#34528=DIRECTION('ref_axis',(1.,0.,0.));
#34529=DIRECTION('',(-0.533122096105522,0.,-0.846038315115843));
#34530=DIRECTION('center_axis',(0.846038315115843,0.,-0.533122096105522));
#34531=DIRECTION('ref_axis',(-0.533122096105522,0.,-0.846038315115843));
#34532=DIRECTION('',(0.,-1.,0.));
#34533=DIRECTION('center_axis',(-0.977354457336591,0.,-0.211608753893355));
#34534=DIRECTION('ref_axis',(-0.211608753893355,0.,0.977354457336591));
#34535=DIRECTION('',(0.,1.,0.));
#34536=DIRECTION('',(-0.211608753893355,0.,0.977354457336591));
#34537=DIRECTION('',(0.,1.,0.));
#34538=DIRECTION('center_axis',(0.,1.,0.));
#34539=DIRECTION('ref_axis',(0.,0.,1.));
#34540=DIRECTION('center_axis',(0.,1.,0.));
#34541=DIRECTION('ref_axis',(1.,0.,0.));
#34542=DIRECTION('',(-0.952218165502102,0.,-0.305418672133534));
#34543=DIRECTION('center_axis',(0.305418672133534,0.,-0.952218165502102));
#34544=DIRECTION('ref_axis',(-0.952218165502102,0.,-0.305418672133534));
#34545=DIRECTION('',(0.,-1.,0.));
#34546=DIRECTION('center_axis',(-0.884716436104133,0.,0.466129625412504));
#34547=DIRECTION('ref_axis',(0.466129625412504,0.,0.884716436104133));
#34548=DIRECTION('',(0.,1.,0.));
#34549=DIRECTION('',(0.466129625412503,0.,0.884716436104133));
#34550=DIRECTION('',(0.,1.,0.));
#34551=DIRECTION('center_axis',(0.,1.,0.));
#34552=DIRECTION('ref_axis',(0.,0.,1.));
#34553=DIRECTION('center_axis',(0.,1.,0.));
#34554=DIRECTION('ref_axis',(1.,0.,0.));
#34555=DIRECTION('',(-0.925760772534179,0.,0.378109761890538));
#34556=DIRECTION('center_axis',(-0.378109761890538,0.,-0.925760772534179));
#34557=DIRECTION('ref_axis',(-0.925760772534179,0.,0.378109761890538));
#34558=DIRECTION('',(0.,-1.,0.));
#34559=DIRECTION('center_axis',(-0.990787227786984,0.,0.135427727050936));
#34560=DIRECTION('ref_axis',(0.135427727050936,0.,0.990787227786984));
#34561=DIRECTION('',(0.,1.,0.));
#34562=DIRECTION('',(0.135427727050936,0.,0.990787227786984));
#34563=DIRECTION('',(0.,1.,0.));
#34564=DIRECTION('center_axis',(0.,1.,0.));
#34565=DIRECTION('ref_axis',(0.,0.,1.));
#34566=DIRECTION('center_axis',(0.,1.,0.));
#34567=DIRECTION('ref_axis',(1.,0.,0.));
#34568=DIRECTION('',(-0.999251721518066,0.,0.0386781209882463));
#34569=DIRECTION('center_axis',(-0.0386781209882463,0.,-0.999251721518066));
#34570=DIRECTION('ref_axis',(-0.999251721518066,0.,0.0386781209882463));
#34571=DIRECTION('',(0.,-1.,0.));
#34572=DIRECTION('center_axis',(-0.846038315115843,0.,-0.533122096105522));
#34573=DIRECTION('ref_axis',(-0.533122096105522,0.,0.846038315115843));
#34574=DIRECTION('',(0.,1.,0.));
#34575=DIRECTION('',(-0.533122096105522,0.,0.846038315115843));
#34576=DIRECTION('',(0.,1.,0.));
#34577=DIRECTION('center_axis',(0.,1.,0.));
#34578=DIRECTION('ref_axis',(0.,0.,1.));
#34579=DIRECTION('center_axis',(0.,1.,0.));
#34580=DIRECTION('ref_axis',(1.,0.,0.));
#34581=DIRECTION('',(-0.790333045483219,0.,-0.612677465896388));
#34582=DIRECTION('center_axis',(0.612677465896388,0.,-0.790333045483219));
#34583=DIRECTION('ref_axis',(-0.790333045483219,0.,-0.612677465896388));
#34584=DIRECTION('',(0.,-1.,0.));
#34585=DIRECTION('center_axis',(-0.305418672133533,0.,-0.952218165502102));
#34586=DIRECTION('ref_axis',(-0.952218165502102,0.,0.305418672133533));
#34587=DIRECTION('',(0.,1.,0.));
#34588=DIRECTION('',(-0.952218165502102,0.,0.305418672133533));
#34589=DIRECTION('',(0.,1.,0.));
#34590=DIRECTION('center_axis',(0.,1.,0.));
#34591=DIRECTION('ref_axis',(0.,0.,1.));
#34592=DIRECTION('center_axis',(0.,1.,0.));
#34593=DIRECTION('ref_axis',(1.,0.,0.));
#34594=DIRECTION('',(-0.211608753893352,0.,-0.977354457336591));
#34595=DIRECTION('center_axis',(0.977354457336591,0.,-0.211608753893352));
#34596=DIRECTION('ref_axis',(-0.211608753893352,0.,-0.977354457336591));
#34597=DIRECTION('',(0.,-1.,0.));
#34598=DIRECTION('center_axis',(0.378109761890538,0.,-0.92576077253418));
#34599=DIRECTION('ref_axis',(-0.92576077253418,0.,-0.378109761890538));
#34600=DIRECTION('',(0.,1.,0.));
#34601=DIRECTION('',(-0.92576077253418,0.,-0.378109761890538));
#34602=DIRECTION('',(0.,1.,0.));
#34603=DIRECTION('center_axis',(0.,1.,0.));
#34604=DIRECTION('ref_axis',(0.,0.,1.));
#34605=DIRECTION('center_axis',(0.,1.,0.));
#34606=DIRECTION('ref_axis',(1.,0.,0.));
#34607=DIRECTION('',(0.466129625412504,0.,-0.884716436104133));
#34608=DIRECTION('center_axis',(0.884716436104133,0.,0.466129625412504));
#34609=DIRECTION('ref_axis',(0.466129625412504,0.,-0.884716436104133));
#34610=DIRECTION('',(0.,-1.,0.));
#34611=DIRECTION('center_axis',(0.671935785203096,0.,-0.740609411608777));
#34612=DIRECTION('ref_axis',(-0.740609411608777,0.,-0.671935785203096));
#34613=DIRECTION('',(0.,1.,0.));
#34614=DIRECTION('',(-0.740609411608777,0.,-0.671935785203096));
#34615=DIRECTION('',(0.,1.,0.));
#34616=DIRECTION('center_axis',(0.,1.,0.));
#34617=DIRECTION('ref_axis',(0.,0.,1.));
#34618=DIRECTION('center_axis',(0.,1.,0.));
#34619=DIRECTION('ref_axis',(1.,0.,0.));
#34620=DIRECTION('',(0.740609411608777,0.,-0.671935785203096));
#34621=DIRECTION('center_axis',(0.,1.,0.));
#34622=DIRECTION('ref_axis',(1.,0.,0.));
#34623=DIRECTION('center_axis',(0.671935785203096,0.,0.740609411608777));
#34624=DIRECTION('ref_axis',(0.740609411608777,0.,-0.671935785203096));
#34625=DIRECTION('',(0.,-1.,0.));
#34626=DIRECTION('center_axis',(0.990787227786984,0.,-0.135427727050936));
#34627=DIRECTION('ref_axis',(-0.135427727050936,0.,-0.990787227786984));
#34628=DIRECTION('',(0.,1.,0.));
#34629=DIRECTION('',(-0.135427727050936,0.,-0.990787227786984));
#34630=DIRECTION('',(0.,1.,0.));
#34631=DIRECTION('center_axis',(0.,1.,0.));
#34632=DIRECTION('ref_axis',(0.,0.,1.));
#34633=DIRECTION('center_axis',(0.,1.,0.));
#34634=DIRECTION('ref_axis',(1.,0.,0.));
#34635=DIRECTION('',(0.999251721518066,0.,-0.0386781209882463));
#34636=DIRECTION('center_axis',(0.0386781209882463,0.,0.999251721518066));
#34637=DIRECTION('ref_axis',(0.999251721518066,0.,-0.0386781209882463));
#34638=DIRECTION('',(0.,-1.,0.));
#34639=DIRECTION('center_axis',(0.846038315115844,0.,0.53312209610552));
#34640=DIRECTION('ref_axis',(0.53312209610552,0.,-0.846038315115844));
#34641=DIRECTION('',(0.,1.,0.));
#34642=DIRECTION('',(0.53312209610552,0.,-0.846038315115844));
#34643=DIRECTION('',(0.,1.,0.));
#34644=DIRECTION('center_axis',(0.,1.,0.));
#34645=DIRECTION('ref_axis',(0.,0.,1.));
#34646=DIRECTION('center_axis',(0.,1.,0.));
#34647=DIRECTION('ref_axis',(1.,0.,0.));
#34648=DIRECTION('',(0.790333045483219,0.,0.612677465896388));
#34649=DIRECTION('center_axis',(-0.612677465896388,0.,0.790333045483219));
#34650=DIRECTION('ref_axis',(0.790333045483219,0.,0.612677465896388));
#34651=DIRECTION('',(0.,-1.,0.));
#34652=DIRECTION('center_axis',(0.305418672133534,0.,0.952218165502102));
#34653=DIRECTION('ref_axis',(0.952218165502102,0.,-0.305418672133534));
#34654=DIRECTION('',(0.,1.,0.));
#34655=DIRECTION('',(0.952218165502102,0.,-0.305418672133534));
#34656=DIRECTION('',(0.,1.,0.));
#34657=DIRECTION('center_axis',(0.,1.,0.));
#34658=DIRECTION('ref_axis',(0.,0.,1.));
#34659=DIRECTION('center_axis',(0.,1.,0.));
#34660=DIRECTION('ref_axis',(1.,0.,0.));
#34661=DIRECTION('',(0.211608753893355,0.,0.977354457336591));
#34662=DIRECTION('center_axis',(-0.977354457336591,0.,0.211608753893355));
#34663=DIRECTION('ref_axis',(0.211608753893355,0.,0.977354457336591));
#34664=DIRECTION('',(0.,-1.,0.));
#34665=DIRECTION('center_axis',(-0.378109761890538,0.,0.925760772534179));
#34666=DIRECTION('ref_axis',(0.925760772534179,0.,0.378109761890538));
#34667=DIRECTION('',(0.,1.,0.));
#34668=DIRECTION('',(0.925760772534179,0.,0.378109761890538));
#34669=DIRECTION('',(0.,1.,0.));
#34670=DIRECTION('center_axis',(0.,1.,0.));
#34671=DIRECTION('ref_axis',(0.,0.,1.));
#34672=DIRECTION('center_axis',(0.,1.,0.));
#34673=DIRECTION('ref_axis',(1.,0.,0.));
#34674=DIRECTION('',(-0.4661296254125,0.,0.884716436104135));
#34675=DIRECTION('center_axis',(-0.884716436104135,0.,-0.4661296254125));
#34676=DIRECTION('ref_axis',(-0.4661296254125,0.,0.884716436104135));
#34677=DIRECTION('',(0.,-1.,0.));
#34678=DIRECTION('center_axis',(0.,-1.,0.));
#34679=DIRECTION('ref_axis',(1.,0.,0.));
#34680=DIRECTION('center_axis',(0.,-1.,0.));
#34681=DIRECTION('ref_axis',(1.,0.,0.));
#34682=DIRECTION('center_axis',(0.,-1.,0.));
#34683=DIRECTION('ref_axis',(1.,0.,0.));
#34684=DIRECTION('center_axis',(0.,-1.,0.));
#34685=DIRECTION('ref_axis',(1.,0.,0.));
#34686=DIRECTION('center_axis',(0.,-1.,0.));
#34687=DIRECTION('ref_axis',(1.,0.,0.));
#34688=DIRECTION('center_axis',(0.,-1.,0.));
#34689=DIRECTION('ref_axis',(1.,0.,0.));
#34690=DIRECTION('center_axis',(0.,-1.,0.));
#34691=DIRECTION('ref_axis',(1.,0.,0.));
#34692=DIRECTION('center_axis',(0.,-1.,0.));
#34693=DIRECTION('ref_axis',(1.,0.,0.));
#34694=DIRECTION('',(0.,1.,0.));
#34695=DIRECTION('center_axis',(0.,-1.,0.));
#34696=DIRECTION('ref_axis',(1.,0.,0.));
#34697=DIRECTION('center_axis',(0.,-1.,0.));
#34698=DIRECTION('ref_axis',(1.,0.,0.));
#34699=DIRECTION('center_axis',(0.,-1.,0.));
#34700=DIRECTION('ref_axis',(1.,0.,0.));
#34701=DIRECTION('center_axis',(0.,-1.,0.));
#34702=DIRECTION('ref_axis',(1.,0.,0.));
#34703=DIRECTION('center_axis',(0.,-1.,0.));
#34704=DIRECTION('ref_axis',(1.,0.,0.));
#34705=DIRECTION('center_axis',(0.,-1.,0.));
#34706=DIRECTION('ref_axis',(1.,0.,0.));
#34707=DIRECTION('center_axis',(0.,-1.,0.));
#34708=DIRECTION('ref_axis',(1.,0.,0.));
#34709=DIRECTION('center_axis',(0.,-1.,0.));
#34710=DIRECTION('ref_axis',(1.,0.,0.));
#34711=DIRECTION('center_axis',(0.,-1.,0.));
#34712=DIRECTION('ref_axis',(1.,0.,0.));
#34713=DIRECTION('center_axis',(0.,-1.,0.));
#34714=DIRECTION('ref_axis',(1.,0.,0.));
#34715=DIRECTION('center_axis',(0.,-1.,0.));
#34716=DIRECTION('ref_axis',(1.,0.,0.));
#34717=DIRECTION('center_axis',(0.,-1.,0.));
#34718=DIRECTION('ref_axis',(1.,0.,0.));
#34719=DIRECTION('center_axis',(0.,1.,0.));
#34720=DIRECTION('ref_axis',(0.,0.,1.));
#34721=DIRECTION('center_axis',(0.,-1.,0.));
#34722=DIRECTION('ref_axis',(1.,0.,0.));
#34723=DIRECTION('center_axis',(0.,-1.,0.));
#34724=DIRECTION('ref_axis',(1.,0.,0.));
#34725=DIRECTION('center_axis',(0.,1.,0.));
#34726=DIRECTION('ref_axis',(1.,0.,8.81908600741727E-14));
#34727=DIRECTION('center_axis',(0.,-1.,0.));
#34728=DIRECTION('ref_axis',(1.,0.,8.81908600741727E-14));
#34729=DIRECTION('center_axis',(0.,1.,0.));
#34730=DIRECTION('ref_axis',(0.,0.,1.));
#34731=DIRECTION('center_axis',(0.,-1.,0.));
#34732=DIRECTION('ref_axis',(1.,0.,0.));
#34733=DIRECTION('center_axis',(0.,-1.,0.));
#34734=DIRECTION('ref_axis',(1.,0.,0.));
#34735=DIRECTION('',(0.707106781186547,0.707106781186547,8.65956056235493E-17));
#34736=DIRECTION('center_axis',(0.,-1.,0.));
#34737=DIRECTION('ref_axis',(1.,0.,0.));
#34738=DIRECTION('center_axis',(0.,-1.,0.));
#34739=DIRECTION('ref_axis',(1.,0.,0.));
#34740=DIRECTION('center_axis',(0.,1.,0.));
#34741=DIRECTION('ref_axis',(0.,0.,1.));
#34742=DIRECTION('center_axis',(0.,-1.,0.));
#34743=DIRECTION('ref_axis',(1.,0.,0.));
#34744=DIRECTION('center_axis',(0.,-1.,0.));
#34745=DIRECTION('ref_axis',(1.,0.,0.));
#34746=DIRECTION('',(0.707106781186545,0.70710678118655,8.6595605623549E-17));
#34747=DIRECTION('center_axis',(0.,1.,0.));
#34748=DIRECTION('ref_axis',(1.,0.,0.));
#34749=DIRECTION('center_axis',(0.,-1.,0.));
#34750=DIRECTION('ref_axis',(1.,0.,0.));
#34751=DIRECTION('',(-0.447213595499958,0.894427190999916,-5.47678698264203E-17));
#34752=DIRECTION('center_axis',(0.,-1.,0.));
#34753=DIRECTION('ref_axis',(0.,0.,-1.));
#34754=DIRECTION('axis',(0.,0.,1.));
#34755=DIRECTION('refdir',(1.,0.,0.));
#34756=DIRECTION('center_axis',(0.,0.,1.));
#34757=DIRECTION('ref_axis',(1.,0.,0.));
#34758=DIRECTION('center_axis',(0.,0.,1.));
#34759=DIRECTION('ref_axis',(1.,0.,0.));
#34760=DIRECTION('',(0.,0.,-1.));
#34761=DIRECTION('center_axis',(0.,0.,1.));
#34762=DIRECTION('ref_axis',(1.,0.,0.));
#34763=DIRECTION('center_axis',(0.,0.,1.));
#34764=DIRECTION('ref_axis',(1.,0.,0.));
#34765=DIRECTION('center_axis',(0.,0.,1.));
#34766=DIRECTION('ref_axis',(1.,0.,0.));
#34767=DIRECTION('',(0.499999999999999,0.866025403784439,0.));
#34768=DIRECTION('',(-0.499999999999999,0.866025403784439,0.));
#34769=DIRECTION('',(-1.,1.37354477598826E-16,0.));
#34770=DIRECTION('',(-0.5,-0.866025403784439,0.));
#34771=DIRECTION('',(0.499999999999998,-0.86602540378444,0.));
#34772=DIRECTION('',(1.,-1.37354477598826E-16,0.));
#34773=DIRECTION('center_axis',(0.,0.,1.));
#34774=DIRECTION('ref_axis',(1.,0.,0.));
#34775=DIRECTION('center_axis',(-1.37354477598826E-16,-1.,0.));
#34776=DIRECTION('ref_axis',(1.,-1.37354477598826E-16,0.));
#34777=DIRECTION('',(1.,-1.37354477598826E-16,0.));
#34778=DIRECTION('',(0.,0.,1.));
#34779=DIRECTION('',(0.,0.,1.));
#34780=DIRECTION('center_axis',(-0.86602540378444,-0.499999999999998,0.));
#34781=DIRECTION('ref_axis',(0.499999999999998,-0.86602540378444,0.));
#34782=DIRECTION('',(0.499999999999998,-0.86602540378444,0.));
#34783=DIRECTION('',(0.,0.,1.));
#34784=DIRECTION('center_axis',(-0.866025403784439,0.5,0.));
#34785=DIRECTION('ref_axis',(-0.5,-0.866025403784439,0.));
#34786=DIRECTION('',(-0.5,-0.866025403784439,0.));
#34787=DIRECTION('',(0.,0.,1.));
#34788=DIRECTION('center_axis',(1.37354477598826E-16,1.,0.));
#34789=DIRECTION('ref_axis',(-1.,1.37354477598826E-16,0.));
#34790=DIRECTION('',(-1.,1.37354477598826E-16,0.));
#34791=DIRECTION('',(0.,0.,1.));
#34792=DIRECTION('center_axis',(0.866025403784439,0.499999999999999,0.));
#34793=DIRECTION('ref_axis',(-0.499999999999999,0.866025403784439,0.));
#34794=DIRECTION('',(-0.499999999999999,0.866025403784439,0.));
#34795=DIRECTION('',(0.,0.,1.));
#34796=DIRECTION('center_axis',(0.866025403784439,-0.499999999999999,0.));
#34797=DIRECTION('ref_axis',(0.499999999999999,0.866025403784439,0.));
#34798=DIRECTION('',(0.499999999999999,0.866025403784439,0.));
#34799=DIRECTION('center_axis',(0.,0.,1.));
#34800=DIRECTION('ref_axis',(1.,0.,0.));
#34801=DIRECTION('center_axis',(0.,0.,1.));
#34802=DIRECTION('ref_axis',(1.,0.,0.));
#34803=DIRECTION('',(0.,1.,0.));
#34804=DIRECTION('center_axis',(0.,0.,1.));
#34805=DIRECTION('ref_axis',(1.,0.,0.));
#34806=DIRECTION('center_axis',(0.,0.,1.));
#34807=DIRECTION('ref_axis',(1.,0.,0.));
#34808=DIRECTION('',(0.,-1.,0.));
#34809=DIRECTION('center_axis',(0.,0.,1.));
#34810=DIRECTION('ref_axis',(1.,0.,0.));
#34811=DIRECTION('center_axis',(0.,0.,1.));
#34812=DIRECTION('ref_axis',(1.,0.,0.));
#34813=DIRECTION('center_axis',(0.,0.,1.));
#34814=DIRECTION('ref_axis',(1.,0.,0.));
#34815=DIRECTION('',(0.,0.,-1.));
#34816=DIRECTION('center_axis',(0.,-1.,0.));
#34817=DIRECTION('ref_axis',(1.,0.,0.));
#34818=DIRECTION('center_axis',(0.,1.,0.));
#34819=DIRECTION('ref_axis',(1.,0.,0.));
#34820=DIRECTION('',(0.,-1.,0.));
#34821=DIRECTION('center_axis',(0.,-1.,0.));
#34822=DIRECTION('ref_axis',(1.,0.,0.));
#34823=DIRECTION('',(0.,-1.,0.));
#34824=DIRECTION('center_axis',(0.452956278458863,0.,0.89153273064128));
#34825=DIRECTION('ref_axis',(-0.89153273064128,0.,0.452956278458863));
#34826=DIRECTION('',(0.89153273064128,0.,-0.452956278458863));
#34827=DIRECTION('',(-0.89153273064128,0.,0.452956278458863));
#34828=DIRECTION('',(0.,-1.,0.));
#34829=DIRECTION('center_axis',(0.866025403784419,0.,-0.500000000000034));
#34830=DIRECTION('ref_axis',(0.500000000000034,0.,0.866025403784419));
#34831=DIRECTION('',(-0.500000000000034,0.,-0.866025403784419));
#34832=DIRECTION('',(0.500000000000034,0.,0.866025403784419));
#34833=DIRECTION('',(0.,-1.,0.));
#34834=DIRECTION('center_axis',(-0.54561185381123,0.,-0.838038009269671));
#34835=DIRECTION('ref_axis',(0.838038009269671,0.,-0.54561185381123));
#34836=DIRECTION('',(-0.838038009269671,0.,0.54561185381123));
#34837=DIRECTION('',(0.838038009269671,0.,-0.54561185381123));
#34838=DIRECTION('',(0.,-1.,0.));
#34839=DIRECTION('center_axis',(0.,-1.,0.));
#34840=DIRECTION('ref_axis',(-0.545611853811243,0.,-0.838038009269663));
#34841=DIRECTION('center_axis',(0.,1.,0.));
#34842=DIRECTION('ref_axis',(1.,0.,0.));
#34843=DIRECTION('center_axis',(0.,-1.,0.));
#34844=DIRECTION('ref_axis',(1.,0.,0.));
#34845=DIRECTION('',(0.,-1.,0.));
#34846=DIRECTION('center_axis',(-0.54561185381123,0.,-0.838038009269671));
#34847=DIRECTION('ref_axis',(0.838038009269671,0.,-0.54561185381123));
#34848=DIRECTION('',(-0.838038009269671,0.,0.54561185381123));
#34849=DIRECTION('',(0.838038009269671,0.,-0.54561185381123));
#34850=DIRECTION('',(0.,-1.,0.));
#34851=DIRECTION('center_axis',(0.452956278458863,0.,0.89153273064128));
#34852=DIRECTION('ref_axis',(-0.89153273064128,0.,0.452956278458863));
#34853=DIRECTION('',(0.89153273064128,0.,-0.452956278458863));
#34854=DIRECTION('',(-0.89153273064128,0.,0.452956278458863));
#34855=DIRECTION('center_axis',(0.,1.,0.));
#34856=DIRECTION('ref_axis',(1.,0.,0.));
#34857=DIRECTION('center_axis',(-0.309016994374968,0.,-0.951056516295147));
#34858=DIRECTION('ref_axis',(-0.951056516295147,0.,0.309016994374968));
#34859=DIRECTION('',(-0.951056516295147,0.,0.309016994374968));
#34860=DIRECTION('',(0.,1.,0.));
#34861=DIRECTION('',(-0.951056516295147,0.,0.309016994374968));
#34862=DIRECTION('',(0.,1.,0.));
#34863=DIRECTION('center_axis',(0.951056516295164,0.,-0.309016994374916));
#34864=DIRECTION('ref_axis',(-0.309016994374916,0.,-0.951056516295164));
#34865=DIRECTION('',(-0.309016994374916,0.,-0.951056516295164));
#34866=DIRECTION('',(0.,1.,0.));
#34867=DIRECTION('',(-0.309016994374916,0.,-0.951056516295164));
#34868=DIRECTION('center_axis',(0.30901699437493,0.,0.951056516295159));
#34869=DIRECTION('ref_axis',(0.951056516295159,0.,-0.30901699437493));
#34870=DIRECTION('',(0.951056516295159,0.,-0.30901699437493));
#34871=DIRECTION('',(0.,1.,0.));
#34872=DIRECTION('',(0.951056516295159,0.,-0.30901699437493));
#34873=DIRECTION('center_axis',(-0.951056516295155,0.,0.309016994374944));
#34874=DIRECTION('ref_axis',(0.309016994374944,0.,0.951056516295155));
#34875=DIRECTION('',(0.309016994374944,0.,0.951056516295155));
#34876=DIRECTION('',(0.309016994374944,0.,0.951056516295155));
#34877=DIRECTION('center_axis',(0.,1.,0.));
#34878=DIRECTION('ref_axis',(0.,0.,1.));
#34879=DIRECTION('center_axis',(0.587785252292488,0.,-0.809016994374936));
#34880=DIRECTION('ref_axis',(-0.809016994374936,0.,-0.587785252292488));
#34881=DIRECTION('',(-0.809016994374936,0.,-0.587785252292488));
#34882=DIRECTION('',(0.,1.,0.));
#34883=DIRECTION('',(-0.809016994374936,0.,-0.587785252292488));
#34884=DIRECTION('',(0.,1.,0.));
#34885=DIRECTION('center_axis',(0.809016994374974,0.,0.587785252292436));
#34886=DIRECTION('ref_axis',(0.587785252292436,0.,-0.809016994374974));
#34887=DIRECTION('',(0.587785252292436,0.,-0.809016994374974));
#34888=DIRECTION('',(0.,1.,0.));
#34889=DIRECTION('',(0.587785252292436,0.,-0.809016994374974));
#34890=DIRECTION('center_axis',(-0.587785252292486,0.,0.809016994374938));
#34891=DIRECTION('ref_axis',(0.809016994374938,0.,0.587785252292486));
#34892=DIRECTION('',(0.809016994374938,0.,0.587785252292486));
#34893=DIRECTION('',(0.,1.,0.));
#34894=DIRECTION('',(0.809016994374938,0.,0.587785252292486));
#34895=DIRECTION('center_axis',(-0.809016994374967,0.,-0.587785252292446));
#34896=DIRECTION('ref_axis',(-0.587785252292446,0.,0.809016994374967));
#34897=DIRECTION('',(-0.587785252292446,0.,0.809016994374967));
#34898=DIRECTION('',(-0.587785252292446,0.,0.809016994374967));
#34899=DIRECTION('center_axis',(0.,1.,0.));
#34900=DIRECTION('ref_axis',(0.,0.,1.));
#34901=DIRECTION('center_axis',(-0.707106781186552,0.,0.707106781186543));
#34902=DIRECTION('ref_axis',(0.707106781186543,0.,0.707106781186552));
#34903=DIRECTION('',(0.707106781186543,0.,0.707106781186552));
#34904=DIRECTION('',(0.,1.,0.));
#34905=DIRECTION('',(0.707106781186543,0.,0.707106781186552));
#34906=DIRECTION('',(0.,1.,0.));
#34907=DIRECTION('center_axis',(-0.707106781186488,0.,-0.707106781186607));
#34908=DIRECTION('ref_axis',(-0.707106781186607,0.,0.707106781186488));
#34909=DIRECTION('',(-0.707106781186607,0.,0.707106781186488));
#34910=DIRECTION('',(0.,1.,0.));
#34911=DIRECTION('',(-0.707106781186607,0.,0.707106781186488));
#34912=DIRECTION('center_axis',(0.707106781186552,0.,-0.707106781186543));
#34913=DIRECTION('ref_axis',(-0.707106781186543,0.,-0.707106781186552));
#34914=DIRECTION('',(-0.707106781186543,0.,-0.707106781186552));
#34915=DIRECTION('',(0.,1.,0.));
#34916=DIRECTION('',(-0.707106781186543,0.,-0.707106781186552));
#34917=DIRECTION('center_axis',(0.707106781186488,0.,0.707106781186607));
#34918=DIRECTION('ref_axis',(0.707106781186607,0.,-0.707106781186488));
#34919=DIRECTION('',(0.707106781186607,0.,-0.707106781186488));
#34920=DIRECTION('',(0.707106781186607,0.,-0.707106781186488));
#34921=DIRECTION('center_axis',(0.,1.,0.));
#34922=DIRECTION('ref_axis',(0.,0.,1.));
#34923=DIRECTION('center_axis',(0.891006524188366,0.,0.45399049973955));
#34924=DIRECTION('ref_axis',(0.45399049973955,0.,-0.891006524188366));
#34925=DIRECTION('',(0.45399049973955,0.,-0.891006524188366));
#34926=DIRECTION('',(0.,1.,0.));
#34927=DIRECTION('',(0.45399049973955,0.,-0.891006524188366));
#34928=DIRECTION('',(0.,1.,0.));
#34929=DIRECTION('center_axis',(-0.453990499739501,0.,0.891006524188391));
#34930=DIRECTION('ref_axis',(0.891006524188391,0.,0.453990499739501));
#34931=DIRECTION('',(0.891006524188391,0.,0.453990499739501));
#34932=DIRECTION('',(0.,1.,0.));
#34933=DIRECTION('',(0.891006524188391,0.,0.453990499739501));
#34934=DIRECTION('center_axis',(-0.891006524188366,0.,-0.45399049973955));
#34935=DIRECTION('ref_axis',(-0.45399049973955,0.,0.891006524188366));
#34936=DIRECTION('',(-0.45399049973955,0.,0.891006524188366));
#34937=DIRECTION('',(0.,1.,0.));
#34938=DIRECTION('',(-0.45399049973955,0.,0.891006524188366));
#34939=DIRECTION('center_axis',(0.453990499739501,0.,-0.891006524188391));
#34940=DIRECTION('ref_axis',(-0.891006524188391,0.,-0.453990499739501));
#34941=DIRECTION('',(-0.891006524188391,0.,-0.453990499739501));
#34942=DIRECTION('',(-0.891006524188391,0.,-0.453990499739501));
#34943=DIRECTION('center_axis',(0.,1.,0.));
#34944=DIRECTION('ref_axis',(0.,0.,1.));
#34945=DIRECTION('center_axis',(0.156434465040221,0.,0.987688340595139));
#34946=DIRECTION('ref_axis',(0.987688340595139,0.,-0.156434465040221));
#34947=DIRECTION('',(0.987688340595139,0.,-0.156434465040221));
#34948=DIRECTION('',(0.,1.,0.));
#34949=DIRECTION('',(0.987688340595139,0.,-0.156434465040221));
#34950=DIRECTION('',(0.,1.,0.));
#34951=DIRECTION('center_axis',(-0.987688340595144,0.,0.156434465040192));
#34952=DIRECTION('ref_axis',(0.156434465040192,0.,0.987688340595144));
#34953=DIRECTION('',(0.156434465040192,0.,0.987688340595144));
#34954=DIRECTION('',(0.,1.,0.));
#34955=DIRECTION('',(0.156434465040192,0.,0.987688340595144));
#34956=DIRECTION('center_axis',(-0.156434465040198,0.,-0.987688340595143));
#34957=DIRECTION('ref_axis',(-0.987688340595143,0.,0.156434465040198));
#34958=DIRECTION('',(-0.987688340595143,0.,0.156434465040198));
#34959=DIRECTION('',(0.,1.,0.));
#34960=DIRECTION('',(-0.987688340595143,0.,0.156434465040198));
#34961=DIRECTION('center_axis',(0.987688340595141,0.,-0.15643446504021));
#34962=DIRECTION('ref_axis',(-0.15643446504021,0.,-0.987688340595141));
#34963=DIRECTION('',(-0.15643446504021,0.,-0.987688340595141));
#34964=DIRECTION('',(-0.15643446504021,0.,-0.987688340595141));
#34965=DIRECTION('center_axis',(0.,1.,0.));
#34966=DIRECTION('ref_axis',(0.,0.,1.));
#34967=DIRECTION('center_axis',(-0.309016994374931,0.,0.951056516295159));
#34968=DIRECTION('ref_axis',(0.951056516295159,0.,0.309016994374931));
#34969=DIRECTION('',(0.951056516295159,0.,0.309016994374931));
#34970=DIRECTION('',(0.,1.,0.));
#34971=DIRECTION('',(0.951056516295159,0.,0.309016994374931));
#34972=DIRECTION('',(0.,1.,0.));
#34973=DIRECTION('center_axis',(-0.951056516295164,0.,-0.309016994374916));
#34974=DIRECTION('ref_axis',(-0.309016994374916,0.,0.951056516295164));
#34975=DIRECTION('',(-0.309016994374916,0.,0.951056516295164));
#34976=DIRECTION('',(0.,1.,0.));
#34977=DIRECTION('',(-0.309016994374916,0.,0.951056516295164));
#34978=DIRECTION('center_axis',(0.309016994374968,0.,-0.951056516295147));
#34979=DIRECTION('ref_axis',(-0.951056516295147,0.,-0.309016994374968));
#34980=DIRECTION('',(-0.951056516295147,0.,-0.309016994374968));
#34981=DIRECTION('',(0.,1.,0.));
#34982=DIRECTION('',(-0.951056516295147,0.,-0.309016994374968));
#34983=DIRECTION('center_axis',(0.951056516295153,0.,0.309016994374951));
#34984=DIRECTION('ref_axis',(0.309016994374951,0.,-0.951056516295153));
#34985=DIRECTION('',(0.309016994374951,0.,-0.951056516295153));
#34986=DIRECTION('',(0.309016994374951,0.,-0.951056516295153));
#34987=DIRECTION('center_axis',(0.,1.,0.));
#34988=DIRECTION('ref_axis',(0.,0.,1.));
#34989=DIRECTION('center_axis',(0.587785252292488,0.,0.809016994374936));
#34990=DIRECTION('ref_axis',(0.809016994374936,0.,-0.587785252292488));
#34991=DIRECTION('',(0.809016994374936,0.,-0.587785252292488));
#34992=DIRECTION('',(0.,1.,0.));
#34993=DIRECTION('',(0.809016994374936,0.,-0.587785252292488));
#34994=DIRECTION('',(0.,1.,0.));
#34995=DIRECTION('center_axis',(-0.809016994374971,0.,0.587785252292441));
#34996=DIRECTION('ref_axis',(0.587785252292441,0.,0.809016994374971));
#34997=DIRECTION('',(0.587785252292441,0.,0.809016994374971));
#34998=DIRECTION('',(0.,1.,0.));
#34999=DIRECTION('',(0.587785252292441,0.,0.809016994374971));
#35000=DIRECTION('center_axis',(-0.587785252292491,0.,-0.809016994374935));
#35001=DIRECTION('ref_axis',(-0.809016994374935,0.,0.587785252292491));
#35002=DIRECTION('',(-0.809016994374935,0.,0.587785252292491));
#35003=DIRECTION('',(0.,1.,0.));
#35004=DIRECTION('',(-0.809016994374935,0.,0.587785252292491));
#35005=DIRECTION('center_axis',(0.809016994374964,0.,-0.587785252292451));
#35006=DIRECTION('ref_axis',(-0.587785252292451,0.,-0.809016994374964));
#35007=DIRECTION('',(-0.587785252292451,0.,-0.809016994374964));
#35008=DIRECTION('',(-0.587785252292451,0.,-0.809016994374964));
#35009=DIRECTION('center_axis',(0.,1.,0.));
#35010=DIRECTION('ref_axis',(0.,0.,1.));
#35011=DIRECTION('center_axis',(1.,0.,0.));
#35012=DIRECTION('ref_axis',(0.,0.,-1.));
#35013=DIRECTION('',(0.,0.,-1.));
#35014=DIRECTION('',(0.,1.,0.));
#35015=DIRECTION('',(0.,0.,-1.));
#35016=DIRECTION('',(0.,1.,0.));
#35017=DIRECTION('center_axis',(0.,0.,1.));
#35018=DIRECTION('ref_axis',(1.,0.,0.));
#35019=DIRECTION('',(1.,0.,0.));
#35020=DIRECTION('',(0.,1.,0.));
#35021=DIRECTION('',(1.,0.,0.));
#35022=DIRECTION('center_axis',(-1.,0.,0.));
#35023=DIRECTION('ref_axis',(0.,0.,1.));
#35024=DIRECTION('',(0.,0.,1.));
#35025=DIRECTION('',(0.,1.,0.));
#35026=DIRECTION('',(0.,0.,1.));
#35027=DIRECTION('center_axis',(0.,0.,-1.));
#35028=DIRECTION('ref_axis',(-1.,0.,0.));
#35029=DIRECTION('',(-1.,0.,0.));
#35030=DIRECTION('',(-1.,0.,0.));
#35031=DIRECTION('center_axis',(0.,1.,0.));
#35032=DIRECTION('ref_axis',(0.,0.,1.));
#35033=DIRECTION('center_axis',(0.891006524188366,0.,-0.453990499739551));
#35034=DIRECTION('ref_axis',(-0.453990499739551,0.,-0.891006524188366));
#35035=DIRECTION('',(-0.453990499739551,0.,-0.891006524188366));
#35036=DIRECTION('',(0.,1.,0.));
#35037=DIRECTION('',(-0.453990499739551,0.,-0.891006524188366));
#35038=DIRECTION('',(0.,1.,0.));
#35039=DIRECTION('center_axis',(0.453990499739501,0.,0.891006524188391));
#35040=DIRECTION('ref_axis',(0.891006524188391,0.,-0.453990499739501));
#35041=DIRECTION('',(0.891006524188391,0.,-0.453990499739501));
#35042=DIRECTION('',(0.,1.,0.));
#35043=DIRECTION('',(0.891006524188391,0.,-0.453990499739501));
#35044=DIRECTION('center_axis',(-0.891006524188366,0.,0.453990499739551));
#35045=DIRECTION('ref_axis',(0.453990499739551,0.,0.891006524188366));
#35046=DIRECTION('',(0.453990499739551,0.,0.891006524188366));
#35047=DIRECTION('',(0.,1.,0.));
#35048=DIRECTION('',(0.453990499739551,0.,0.891006524188366));
#35049=DIRECTION('center_axis',(-0.453990499739501,0.,-0.891006524188391));
#35050=DIRECTION('ref_axis',(-0.891006524188391,0.,0.453990499739501));
#35051=DIRECTION('',(-0.891006524188391,0.,0.453990499739501));
#35052=DIRECTION('',(-0.891006524188391,0.,0.453990499739501));
#35053=DIRECTION('center_axis',(0.,1.,0.));
#35054=DIRECTION('ref_axis',(0.,0.,1.));
#35055=DIRECTION('center_axis',(0.156434465040197,0.,-0.987688340595143));
#35056=DIRECTION('ref_axis',(-0.987688340595143,0.,-0.156434465040197));
#35057=DIRECTION('',(-0.987688340595143,0.,-0.156434465040197));
#35058=DIRECTION('',(0.,1.,0.));
#35059=DIRECTION('',(-0.987688340595143,0.,-0.156434465040197));
#35060=DIRECTION('',(0.,1.,0.));
#35061=DIRECTION('center_axis',(0.987688340595143,0.,0.156434465040199));
#35062=DIRECTION('ref_axis',(0.156434465040199,0.,-0.987688340595143));
#35063=DIRECTION('',(0.156434465040199,0.,-0.987688340595143));
#35064=DIRECTION('',(0.,1.,0.));
#35065=DIRECTION('',(0.156434465040199,0.,-0.987688340595143));
#35066=DIRECTION('center_axis',(-0.156434465040221,0.,0.987688340595139));
#35067=DIRECTION('ref_axis',(0.987688340595139,0.,0.156434465040221));
#35068=DIRECTION('',(0.987688340595139,0.,0.156434465040221));
#35069=DIRECTION('',(0.,1.,0.));
#35070=DIRECTION('',(0.987688340595139,0.,0.156434465040221));
#35071=DIRECTION('center_axis',(-0.987688340595141,0.,-0.15643446504021));
#35072=DIRECTION('ref_axis',(-0.15643446504021,0.,0.987688340595141));
#35073=DIRECTION('',(-0.15643446504021,0.,0.987688340595141));
#35074=DIRECTION('',(-0.15643446504021,0.,0.987688340595141));
#35075=DIRECTION('center_axis',(0.,1.,0.));
#35076=DIRECTION('ref_axis',(0.,0.,1.));
#35077=DIRECTION('center_axis',(-0.707106781186553,0.,-0.707106781186542));
#35078=DIRECTION('ref_axis',(-0.707106781186542,0.,0.707106781186553));
#35079=DIRECTION('',(-0.707106781186542,0.,0.707106781186553));
#35080=DIRECTION('',(0.,1.,0.));
#35081=DIRECTION('',(-0.707106781186542,0.,0.707106781186553));
#35082=DIRECTION('',(0.,1.,0.));
#35083=DIRECTION('center_axis',(0.707106781186488,0.,-0.707106781186607));
#35084=DIRECTION('ref_axis',(-0.707106781186607,0.,-0.707106781186488));
#35085=DIRECTION('',(-0.707106781186607,0.,-0.707106781186488));
#35086=DIRECTION('',(0.,1.,0.));
#35087=DIRECTION('',(-0.707106781186607,0.,-0.707106781186488));
#35088=DIRECTION('center_axis',(0.707106781186553,0.,0.707106781186542));
#35089=DIRECTION('ref_axis',(0.707106781186542,0.,-0.707106781186553));
#35090=DIRECTION('',(0.707106781186542,0.,-0.707106781186553));
#35091=DIRECTION('',(0.,1.,0.));
#35092=DIRECTION('',(0.707106781186542,0.,-0.707106781186553));
#35093=DIRECTION('center_axis',(-0.707106781186488,0.,0.707106781186607));
#35094=DIRECTION('ref_axis',(0.707106781186607,0.,0.707106781186488));
#35095=DIRECTION('',(0.707106781186607,0.,0.707106781186488));
#35096=DIRECTION('',(0.707106781186607,0.,0.707106781186488));
#35097=DIRECTION('center_axis',(0.,1.,0.));
#35098=DIRECTION('ref_axis',(0.,0.,1.));
#35099=DIRECTION('center_axis',(0.,1.,0.));
#35100=DIRECTION('ref_axis',(0.,0.,1.));
#35101=DIRECTION('center_axis',(0.,-1.,0.));
#35102=DIRECTION('ref_axis',(1.,0.,0.));
#35103=DIRECTION('center_axis',(0.,-1.,0.));
#35104=DIRECTION('ref_axis',(1.,0.,0.));
#35105=DIRECTION('',(0.,-1.,0.));
#35106=DIRECTION('center_axis',(0.,1.,0.));
#35107=DIRECTION('ref_axis',(1.,0.,0.));
#35108=DIRECTION('center_axis',(0.,1.,0.));
#35109=DIRECTION('ref_axis',(0.,0.,1.));
#35110=DIRECTION('center_axis',(0.,-1.,0.));
#35111=DIRECTION('ref_axis',(1.,0.,0.));
#35112=DIRECTION('center_axis',(0.,-1.,0.));
#35113=DIRECTION('ref_axis',(1.,0.,0.));
#35114=DIRECTION('center_axis',(0.,-1.,0.));
#35115=DIRECTION('ref_axis',(1.,0.,0.));
#35116=DIRECTION('',(0.707106781186548,0.707106781186547,8.65956056235494E-17));
#35117=DIRECTION('center_axis',(0.,-1.,0.));
#35118=DIRECTION('ref_axis',(1.,0.,0.));
#35119=DIRECTION('center_axis',(0.,-1.,0.));
#35120=DIRECTION('ref_axis',(1.,0.,0.));
#35121=DIRECTION('',(0.,1.,0.));
#35122=DIRECTION('center_axis',(0.,1.,0.));
#35123=DIRECTION('ref_axis',(0.,0.,1.));
#35124=DIRECTION('center_axis',(0.,-1.,0.));
#35125=DIRECTION('ref_axis',(1.,0.,0.));
#35126=DIRECTION('center_axis',(0.,-1.,0.));
#35127=DIRECTION('ref_axis',(1.,0.,0.));
#35128=DIRECTION('center_axis',(0.,-1.,0.));
#35129=DIRECTION('ref_axis',(1.,0.,0.));
#35130=DIRECTION('',(0.,1.,0.));
#35131=DIRECTION('center_axis',(0.,1.,0.));
#35132=DIRECTION('ref_axis',(1.,0.,0.));
#35133=DIRECTION('center_axis',(0.,-1.,0.));
#35134=DIRECTION('ref_axis',(1.,0.,0.));
#35135=DIRECTION('',(-0.707106781186547,0.707106781186548,-8.65956056235492E-17));
#35136=DIRECTION('center_axis',(0.,-1.,0.));
#35137=DIRECTION('ref_axis',(0.,0.,-1.));
#35138=DIRECTION('axis',(0.,0.,1.));
#35139=DIRECTION('refdir',(1.,0.,0.));
#35140=DIRECTION('',(0.616833943686132,1.43989874226525E-14,0.787093314618168));
#35141=DIRECTION('center_axis',(1.,0.,0.));
#35142=DIRECTION('ref_axis',(0.,0.,-1.));
#35143=DIRECTION('',(1.,0.,0.));
#35144=DIRECTION('center_axis',(0.,1.,0.));
#35145=DIRECTION('ref_axis',(0.,0.,1.));
#35146=DIRECTION('center_axis',(0.,1.,0.));
#35147=DIRECTION('ref_axis',(1.,0.,0.));
#35148=DIRECTION('',(0.,-1.,0.));
#35149=DIRECTION('center_axis',(0.,1.,0.));
#35150=DIRECTION('ref_axis',(1.,0.,0.));
#35151=DIRECTION('',(-0.616833943686132,0.,0.787093314618168));
#35152=DIRECTION('center_axis',(0.,1.,0.));
#35153=DIRECTION('ref_axis',(0.,0.,1.));
#35154=DIRECTION('center_axis',(-1.,0.,0.));
#35155=DIRECTION('ref_axis',(0.,0.,-1.));
#35156=DIRECTION('center_axis',(0.,-1.,0.));
#35157=DIRECTION('ref_axis',(0.,0.,1.));
#35158=DIRECTION('center_axis',(0.,1.,0.));
#35159=DIRECTION('ref_axis',(0.,0.,1.));
#35160=DIRECTION('center_axis',(0.,1.,0.));
#35161=DIRECTION('ref_axis',(0.,0.,1.));
#35162=DIRECTION('',(0.,-1.,0.));
#35163=DIRECTION('',(0.,-1.,0.));
#35164=DIRECTION('center_axis',(0.,1.,0.));
#35165=DIRECTION('ref_axis',(1.,0.,0.));
#35166=DIRECTION('center_axis',(0.,-1.,0.));
#35167=DIRECTION('ref_axis',(0.,0.,-1.));
#35168=DIRECTION('center_axis',(0.,1.,0.));
#35169=DIRECTION('ref_axis',(1.,0.,0.));
#35170=DIRECTION('center_axis',(0.,1.,0.));
#35171=DIRECTION('ref_axis',(0.,0.,1.));
#35172=DIRECTION('',(8.6595605623547E-17,-0.707106781186566,0.707106781186529));
#35173=DIRECTION('center_axis',(0.,-1.,0.));
#35174=DIRECTION('ref_axis',(0.,0.,-1.));
#35175=DIRECTION('center_axis',(0.,1.,0.));
#35176=DIRECTION('ref_axis',(1.,0.,0.));
#35177=DIRECTION('center_axis',(0.,1.,0.));
#35178=DIRECTION('ref_axis',(0.,0.,1.));
#35179=DIRECTION('center_axis',(0.,1.,0.));
#35180=DIRECTION('ref_axis',(1.,0.,0.));
#35181=DIRECTION('',(8.65956056235532E-17,-0.707106781186516,0.707106781186579));
#35182=DIRECTION('center_axis',(0.,1.,0.));
#35183=DIRECTION('ref_axis',(0.,0.,1.));
#35184=DIRECTION('center_axis',(0.,1.,0.));
#35185=DIRECTION('ref_axis',(1.,0.,0.));
#35186=DIRECTION('',(0.,-1.,0.));
#35187=DIRECTION('center_axis',(0.,-1.,0.));
#35188=DIRECTION('ref_axis',(0.,0.,1.));
#35189=DIRECTION('center_axis',(0.,1.,0.));
#35190=DIRECTION('ref_axis',(1.,0.,0.));
#35191=DIRECTION('',(-8.65956056235524E-17,-0.707106781186522,-0.707106781186573));
#35192=DIRECTION('center_axis',(0.,1.,0.));
#35193=DIRECTION('ref_axis',(0.,0.,1.));
#35194=DIRECTION('center_axis',(0.,-1.,0.));
#35195=DIRECTION('ref_axis',(0.,0.,1.));
#35196=DIRECTION('center_axis',(0.,1.,0.));
#35197=DIRECTION('ref_axis',(1.,0.,0.));
#35198=DIRECTION('',(-8.65956056235509E-17,-0.707106781186535,-0.70710678118656));
#35199=DIRECTION('center_axis',(0.,1.,0.));
#35200=DIRECTION('ref_axis',(0.,0.,1.));
#35201=DIRECTION('axis',(0.,0.,1.));
#35202=DIRECTION('refdir',(1.,0.,0.));
#35203=DIRECTION('center_axis',(-0.99999684852218,9.62964972193618E-35,
0.00251056680999716));
#35204=DIRECTION('ref_axis',(3.0745576079086E-19,1.,1.22464293970013E-16));
#35205=DIRECTION('center_axis',(0.496743222852577,9.62964972193618E-35,
-0.867897557635712));
#35206=DIRECTION('ref_axis',(-1.06286796594638E-16,1.,-6.08334997864549E-17));
#35207=DIRECTION('center_axis',(0.496743222852577,9.62964972193618E-35,
-0.867897557635712));
#35208=DIRECTION('ref_axis',(-1.06286796594638E-16,1.,-6.08334997864549E-17));
#35209=DIRECTION('center_axis',(-0.99999684852218,9.62964972193618E-35,
0.00251056680999716));
#35210=DIRECTION('ref_axis',(3.0745576079086E-19,1.,1.22464293970013E-16));
#35211=DIRECTION('axis',(0.,0.,1.));
#35212=DIRECTION('refdir',(1.,0.,0.));
#35213=DIRECTION('center_axis',(0.707106781186547,-0.542827373086154,-0.453142850576268));
#35214=DIRECTION('ref_axis',(-0.53955578700857,0.,-0.841949851657189));
#35215=DIRECTION('',(0.53955578700857,0.,0.841949851657189));
#35216=DIRECTION('',(0.,0.640840764977362,-0.767673833045799));
#35217=DIRECTION('',(-0.608934580549686,-0.793220446414978,0.));
#35218=DIRECTION('',(0.,-0.640840764977362,0.767673833045799));
#35219=DIRECTION('center_axis',(0.,-0.767673833045799,-0.640840764977362));
#35220=DIRECTION('ref_axis',(0.,0.640840764977362,-0.767673833045799));
#35221=DIRECTION('',(1.,0.,0.));
#35222=DIRECTION('',(0.,-0.640840764977362,0.767673833045799));
#35223=DIRECTION('',(-1.,0.,0.));
#35224=DIRECTION('center_axis',(-0.707106781186547,-0.542827373086154,-0.453142850576268));
#35225=DIRECTION('ref_axis',(-0.53955578700857,0.,0.841949851657189));
#35226=DIRECTION('',(-0.608934580549686,0.793220446414978,0.));
#35227=DIRECTION('',(0.53955578700857,0.,-0.841949851657189));
#35228=DIRECTION('',(0.,0.640840764977362,-0.767673833045799));
#35229=DIRECTION('center_axis',(0.707106781186545,0.542827373086156,-0.453142850576269));
#35230=DIRECTION('ref_axis',(-0.539555787008572,0.,-0.841949851657188));
#35231=DIRECTION('',(0.608934580549689,-0.793220446414977,0.));
#35232=DIRECTION('',(0.,0.640840764977362,0.767673833045799));
#35233=DIRECTION('',(-0.539555787008572,0.,-0.841949851657188));
#35234=DIRECTION('',(0.,-0.640840764977362,-0.767673833045799));
#35235=DIRECTION('center_axis',(0.,0.767673833045799,-0.640840764977362));
#35236=DIRECTION('ref_axis',(0.,0.640840764977362,0.767673833045799));
#35237=DIRECTION('',(1.,0.,0.));
#35238=DIRECTION('',(0.,-0.640840764977362,-0.767673833045799));
#35239=DIRECTION('',(-1.,0.,0.));
#35240=DIRECTION('center_axis',(-0.707106781186545,0.542827373086156,-0.453142850576269));
#35241=DIRECTION('ref_axis',(-0.539555787008572,0.,0.841949851657188));
#35242=DIRECTION('',(-0.539555787008572,0.,0.841949851657188));
#35243=DIRECTION('',(0.608934580549689,0.793220446414977,0.));
#35244=DIRECTION('',(0.,0.640840764977362,0.767673833045799));
#35245=DIRECTION('center_axis',(0.707106781186551,-0.5337451437584,0.463806124921093));
#35246=DIRECTION('ref_axis',(0.548464086412375,0.,-0.836174112201423));
#35247=DIRECTION('',(0.602464182205077,0.798145919716418,0.));
#35248=DIRECTION('',(0.,0.655920912175122,0.75482962115391));
#35249=DIRECTION('',(0.548464086412375,0.,-0.836174112201423));
#35250=DIRECTION('',(-0.383127220471085,-0.840492156934374,-0.383127220471092));
#35251=DIRECTION('',(0.,-0.655920912175122,-0.75482962115391));
#35252=DIRECTION('center_axis',(0.,-0.414776498746543,0.909923324290327));
#35253=DIRECTION('ref_axis',(1.,0.,0.));
#35254=DIRECTION('',(-1.,0.,0.));
#35255=DIRECTION('',(0.,0.909923324290327,0.414776498746543));
#35256=DIRECTION('',(-1.,0.,0.));
#35257=DIRECTION('',(0.,-0.909923324290327,-0.414776498746543));
#35258=DIRECTION('',(-1.,0.,0.));
#35259=DIRECTION('',(-0.383127220471085,0.840492156934374,0.383127220471092));
#35260=DIRECTION('',(1.,0.,0.));
#35261=DIRECTION('center_axis',(1.,0.,0.));
#35262=DIRECTION('ref_axis',(0.,0.,-1.));
#35263=DIRECTION('',(0.,0.,1.));
#35264=DIRECTION('',(0.,0.707106781186541,0.707106781186554));
#35265=DIRECTION('center_axis',(-0.707106781186551,-0.5337451437584,0.463806124921093));
#35266=DIRECTION('ref_axis',(0.548464086412375,0.,0.836174112201423));
#35267=DIRECTION('',(0.548464086412375,0.,0.836174112201423));
#35268=DIRECTION('',(0.,-0.655920912175122,-0.75482962115391));
#35269=DIRECTION('',(0.602464182205077,-0.798145919716418,0.));
#35270=DIRECTION('',(0.,0.655920912175122,0.75482962115391));
#35271=DIRECTION('center_axis',(-1.,0.,0.));
#35272=DIRECTION('ref_axis',(0.,0.,1.));
#35273=DIRECTION('',(0.,0.,-1.));
#35274=DIRECTION('',(0.,-0.707106781186541,-0.707106781186554));
#35275=DIRECTION('center_axis',(-1.,0.,0.));
#35276=DIRECTION('ref_axis',(0.,0.,1.));
#35277=DIRECTION('',(0.,1.,0.));
#35278=DIRECTION('',(0.,-0.923879532511279,-0.382683432365109));
#35279=DIRECTION('',(0.,0.707106781186546,0.707106781186549));
#35280=DIRECTION('',(0.,-1.,0.));
#35281=DIRECTION('',(0.,0.,1.));
#35282=DIRECTION('center_axis',(0.,0.,1.));
#35283=DIRECTION('ref_axis',(1.,0.,0.));
#35284=DIRECTION('',(-1.,0.,0.));
#35285=DIRECTION('',(0.,-1.,0.));
#35286=DIRECTION('',(1.,0.,0.));
#35287=DIRECTION('',(0.,1.,0.));
#35288=DIRECTION('',(-1.,0.,0.));
#35289=DIRECTION('center_axis',(0.707106781186548,0.,0.707106781186548));
#35290=DIRECTION('ref_axis',(0.707106781186548,0.,-0.707106781186548));
#35291=DIRECTION('',(-0.577350269189629,-0.577350269189619,0.577350269189629));
#35292=DIRECTION('',(0.577350269189629,-0.577350269189619,-0.577350269189629));
#35293=DIRECTION('',(0.577350269189629,0.577350269189619,-0.577350269189629));
#35294=DIRECTION('',(0.,1.,0.));
#35295=DIRECTION('',(-0.577350269189616,0.577350269189646,0.577350269189616));
#35296=DIRECTION('center_axis',(0.,0.707106781186554,0.707106781186541));
#35297=DIRECTION('ref_axis',(1.,0.,0.));
#35298=DIRECTION('',(0.577350269189602,-0.577350269189633,0.577350269189643));
#35299=DIRECTION('',(-1.,0.,0.));
#35300=DIRECTION('',(0.577350269189629,0.577350269189619,-0.577350269189629));
#35301=DIRECTION('',(-0.577350269189629,0.577350269189619,-0.577350269189629));
#35302=DIRECTION('center_axis',(0.707106781186566,0.707106781186529,0.));
#35303=DIRECTION('ref_axis',(0.,0.,-1.));
#35304=DIRECTION('',(0.,0.,-1.));
#35305=DIRECTION('',(0.707106781186529,-0.707106781186566,0.));
#35306=DIRECTION('',(0.,0.,1.));
#35307=DIRECTION('center_axis',(-0.707106781186548,0.,0.707106781186548));
#35308=DIRECTION('ref_axis',(0.707106781186548,0.,0.707106781186548));
#35309=DIRECTION('',(0.577350269189629,0.577350269189619,0.577350269189629));
#35310=DIRECTION('',(-0.577350269189629,-0.577350269189619,-0.577350269189629));
#35311=DIRECTION('',(0.,-1.,0.));
#35312=DIRECTION('',(0.577350269189629,-0.577350269189619,0.577350269189629));
#35313=DIRECTION('center_axis',(0.,-0.707106781186554,0.707106781186541));
#35314=DIRECTION('ref_axis',(1.,0.,0.));
#35315=DIRECTION('',(-0.577350269189629,0.577350269189619,0.577350269189629));
#35316=DIRECTION('',(1.,0.,0.));
#35317=DIRECTION('center_axis',(-0.707106781186541,-0.707106781186554,0.));
#35318=DIRECTION('ref_axis',(0.,0.,1.));
#35319=DIRECTION('',(0.,0.,-1.));
#35320=DIRECTION('',(-0.707106781186554,0.707106781186541,0.));
#35321=DIRECTION('',(0.,0.,1.));
#35322=DIRECTION('center_axis',(0.707106781186551,0.5337451437584,0.463806124921093));
#35323=DIRECTION('ref_axis',(0.548464086412375,0.,-0.836174112201423));
#35324=DIRECTION('',(0.383127220471068,-0.840492156934371,0.383127220471115));
#35325=DIRECTION('',(-0.548464086412375,0.,0.836174112201423));
#35326=DIRECTION('',(0.,0.655920912175122,-0.75482962115391));
#35327=DIRECTION('',(-0.602464182205077,0.798145919716418,0.));
#35328=DIRECTION('',(0.,-0.655920912175122,0.75482962115391));
#35329=DIRECTION('center_axis',(0.,0.414776498746564,0.909923324290317));
#35330=DIRECTION('ref_axis',(1.,0.,0.));
#35331=DIRECTION('',(1.,0.,0.));
#35332=DIRECTION('',(-1.,0.,0.));
#35333=DIRECTION('',(0.383127220471068,0.840492156934371,-0.383127220471115));
#35334=DIRECTION('',(1.,0.,0.));
#35335=DIRECTION('',(0.,-0.909923324290317,0.414776498746564));
#35336=DIRECTION('',(1.,0.,0.));
#35337=DIRECTION('',(0.,0.909923324290317,-0.414776498746564));
#35338=DIRECTION('center_axis',(0.,0.75482962115391,0.655920912175122));
#35339=DIRECTION('ref_axis',(0.,-0.655920912175122,0.75482962115391));
#35340=DIRECTION('',(-1.,0.,0.));
#35341=DIRECTION('',(0.,0.655920912175122,-0.75482962115391));
#35342=DIRECTION('center_axis',(1.,0.,0.));
#35343=DIRECTION('ref_axis',(0.,0.,-1.));
#35344=DIRECTION('',(0.,-1.,0.));
#35345=DIRECTION('',(0.,0.923879532511279,-0.382683432365109));
#35346=DIRECTION('',(0.,-0.707106781186546,0.707106781186549));
#35347=DIRECTION('',(0.,1.,0.));
#35348=DIRECTION('',(0.,0.,1.));
#35349=DIRECTION('center_axis',(0.,0.,-1.));
#35350=DIRECTION('ref_axis',(0.,1.,0.));
#35351=DIRECTION('',(1.,0.,0.));
#35352=DIRECTION('',(0.,-1.,0.));
#35353=DIRECTION('',(-0.602464182205077,-0.798145919716418,0.));
#35354=DIRECTION('center_axis',(-0.707106781186551,0.5337451437584,0.463806124921093));
#35355=DIRECTION('ref_axis',(0.548464086412375,0.,0.836174112201423));
#35356=DIRECTION('',(0.,-0.655920912175122,0.75482962115391));
#35357=DIRECTION('',(-0.548464086412375,0.,-0.836174112201423));
#35358=DIRECTION('center_axis',(-1.,0.,0.));
#35359=DIRECTION('ref_axis',(0.,0.,1.));
#35360=DIRECTION('',(0.,0.,-1.));
#35361=DIRECTION('',(0.,0.707106781186546,-0.707106781186549));
#35362=DIRECTION('',(0.,-0.923879532511279,0.382683432365109));
#35363=DIRECTION('',(0.,1.,0.));
#35364=DIRECTION('center_axis',(-1.,0.,0.));
#35365=DIRECTION('ref_axis',(0.,0.,1.));
#35366=DIRECTION('',(0.,0.,1.));
#35367=DIRECTION('',(0.,-0.707106781186541,0.707106781186554));
#35368=DIRECTION('center_axis',(1.,0.,0.));
#35369=DIRECTION('ref_axis',(0.,0.,-1.));
#35370=DIRECTION('',(0.,0.,-1.));
#35371=DIRECTION('',(0.,0.707106781186541,-0.707106781186554));
#35372=DIRECTION('center_axis',(0.,0.,1.));
#35373=DIRECTION('ref_axis',(1.,0.,0.));
#35374=DIRECTION('',(1.,0.,0.));
#35375=DIRECTION('',(0.,1.,0.));
#35376=DIRECTION('',(-1.,0.,0.));
#35377=DIRECTION('',(0.,-1.,0.));
#35378=DIRECTION('',(1.,0.,0.));
#35379=DIRECTION('center_axis',(0.707106781186548,0.,0.707106781186548));
#35380=DIRECTION('ref_axis',(0.707106781186548,0.,-0.707106781186548));
#35381=DIRECTION('',(-0.577350269189629,-0.577350269189619,0.577350269189629));
#35382=DIRECTION('',(0.577350269189629,-0.577350269189619,-0.577350269189629));
#35383=DIRECTION('',(0.577350269189629,0.577350269189619,-0.577350269189629));
#35384=DIRECTION('',(0.,1.,0.));
#35385=DIRECTION('',(-0.577350269189616,0.577350269189646,0.577350269189616));
#35386=DIRECTION('center_axis',(0.707106781186541,-0.707106781186554,0.));
#35387=DIRECTION('ref_axis',(0.,0.,-1.));
#35388=DIRECTION('',(-0.577350269189629,-0.577350269189619,-0.577350269189629));
#35389=DIRECTION('',(0.,0.,-1.));
#35390=DIRECTION('',(-0.707106781186554,-0.707106781186541,0.));
#35391=DIRECTION('',(0.,0.,1.));
#35392=DIRECTION('center_axis',(0.,-0.707106781186554,0.707106781186541));
#35393=DIRECTION('ref_axis',(1.,0.,0.));
#35394=DIRECTION('',(0.577350269189629,0.577350269189619,0.577350269189629));
#35395=DIRECTION('',(-0.577350269189629,0.577350269189619,0.577350269189629));
#35396=DIRECTION('',(1.,0.,0.));
#35397=DIRECTION('center_axis',(-0.707106781186548,0.,0.707106781186548));
#35398=DIRECTION('ref_axis',(0.707106781186548,0.,0.707106781186548));
#35399=DIRECTION('',(-0.577350269189629,0.577350269189619,-0.577350269189629));
#35400=DIRECTION('',(-0.577350269189629,-0.577350269189619,-0.577350269189629));
#35401=DIRECTION('',(0.,-1.,0.));
#35402=DIRECTION('',(0.577350269189629,-0.577350269189619,0.577350269189629));
#35403=DIRECTION('center_axis',(-0.707106781186541,-0.707106781186554,0.));
#35404=DIRECTION('ref_axis',(0.,0.,1.));
#35405=DIRECTION('',(0.,0.,-1.));
#35406=DIRECTION('',(-0.707106781186554,0.707106781186541,0.));
#35407=DIRECTION('',(0.,0.,1.));
#35408=DIRECTION('center_axis',(0.,0.,1.));
#35409=DIRECTION('ref_axis',(-0.707106781186548,-0.707106781186548,0.));
#35410=DIRECTION('',(0.,-0.707106781186553,0.707106781186543));
#35411=DIRECTION('center_axis',(0.,0.,-1.));
#35412=DIRECTION('ref_axis',(-0.707106781186547,-0.707106781186547,0.));
#35413=DIRECTION('',(0.707106781186553,0.,-0.707106781186543));
#35414=DIRECTION('center_axis',(0.,0.,1.));
#35415=DIRECTION('ref_axis',(-0.707106781186548,-0.707106781186548,0.));
#35416=DIRECTION('center_axis',(0.,-0.707106781186543,-0.707106781186553));
#35417=DIRECTION('ref_axis',(-1.,0.,0.));
#35418=DIRECTION('',(0.,-0.707106781186553,0.707106781186543));
#35419=DIRECTION('',(-1.,0.,0.));
#35420=DIRECTION('',(1.,0.,0.));
#35421=DIRECTION('center_axis',(0.,0.,1.));
#35422=DIRECTION('ref_axis',(0.707106781186547,-0.707106781186547,0.));
#35423=DIRECTION('',(0.707106781186578,0.,0.707106781186517));
#35424=DIRECTION('center_axis',(0.,0.,-1.));
#35425=DIRECTION('ref_axis',(0.707106781186547,-0.707106781186547,0.));
#35426=DIRECTION('center_axis',(0.,0.,1.));
#35427=DIRECTION('ref_axis',(0.707106781186547,-0.707106781186547,0.));
#35428=DIRECTION('center_axis',(0.707106781186568,0.,-0.707106781186527));
#35429=DIRECTION('ref_axis',(-0.707106781186527,0.,-0.707106781186568));
#35430=DIRECTION('',(0.707106781186527,0.,0.707106781186568));
#35431=DIRECTION('',(0.,-1.,0.));
#35432=DIRECTION('',(0.,1.,0.));
#35433=DIRECTION('center_axis',(0.,0.,1.));
#35434=DIRECTION('ref_axis',(0.707106781186547,0.707106781186547,0.));
#35435=DIRECTION('',(0.,0.707106781186553,0.707106781186543));
#35436=DIRECTION('center_axis',(0.,0.,-1.));
#35437=DIRECTION('ref_axis',(0.707106781186547,0.707106781186547,0.));
#35438=DIRECTION('center_axis',(0.,0.,1.));
#35439=DIRECTION('ref_axis',(0.707106781186547,0.707106781186547,0.));
#35440=DIRECTION('center_axis',(0.,0.707106781186543,-0.707106781186553));
#35441=DIRECTION('ref_axis',(-1.,0.,0.));
#35442=DIRECTION('',(0.,0.707106781186553,0.707106781186543));
#35443=DIRECTION('',(1.,0.,0.));
#35444=DIRECTION('',(-1.,0.,0.));
#35445=DIRECTION('center_axis',(0.,0.,1.));
#35446=DIRECTION('ref_axis',(-0.707106781186548,0.707106781186548,0.));
#35447=DIRECTION('',(-0.707106781186553,0.,0.707106781186543));
#35448=DIRECTION('center_axis',(0.,0.,-1.));
#35449=DIRECTION('ref_axis',(-0.707106781186547,0.707106781186547,0.));
#35450=DIRECTION('center_axis',(0.,0.,1.));
#35451=DIRECTION('ref_axis',(-0.707106781186548,0.707106781186548,0.));
#35452=DIRECTION('center_axis',(-0.707106781186543,0.,-0.707106781186553));
#35453=DIRECTION('ref_axis',(-0.707106781186553,0.,0.707106781186543));
#35454=DIRECTION('',(0.,1.,0.));
#35455=DIRECTION('',(0.,-1.,0.));
#35456=DIRECTION('center_axis',(0.,1.,0.));
#35457=DIRECTION('ref_axis',(-1.,0.,0.));
#35458=DIRECTION('',(0.,0.,-1.));
#35459=DIRECTION('',(-1.,0.,0.));
#35460=DIRECTION('',(0.,0.,1.));
#35461=DIRECTION('center_axis',(0.,0.,1.));
#35462=DIRECTION('ref_axis',(-0.707106781186547,0.707106781186547,0.));
#35463=DIRECTION('',(0.,0.,1.));
#35464=DIRECTION('center_axis',(0.,0.,1.));
#35465=DIRECTION('ref_axis',(-0.707106781186547,0.707106781186547,0.));
#35466=DIRECTION('center_axis',(-1.,0.,0.));
#35467=DIRECTION('ref_axis',(0.,-1.,0.));
#35468=DIRECTION('',(0.,0.,-1.));
#35469=DIRECTION('',(0.,-1.,0.));
#35470=DIRECTION('center_axis',(0.,0.,1.));
#35471=DIRECTION('ref_axis',(-0.707106781186547,-0.707106781186547,0.));
#35472=DIRECTION('',(0.,0.,1.));
#35473=DIRECTION('center_axis',(0.,0.,1.));
#35474=DIRECTION('ref_axis',(-0.707106781186547,-0.707106781186547,0.));
#35475=DIRECTION('center_axis',(0.,0.,1.));
#35476=DIRECTION('ref_axis',(1.,0.,0.));
#35477=DIRECTION('center_axis',(0.,0.,-1.));
#35478=DIRECTION('ref_axis',(1.,0.,0.));
#35479=DIRECTION('center_axis',(0.,0.,-1.));
#35480=DIRECTION('ref_axis',(1.,0.,0.));
#35481=DIRECTION('center_axis',(-1.,0.,0.));
#35482=DIRECTION('ref_axis',(0.,-1.,0.));
#35483=DIRECTION('',(0.,0.,1.));
#35484=DIRECTION('',(0.,1.,0.));
#35485=DIRECTION('center_axis',(1.,0.,0.));
#35486=DIRECTION('ref_axis',(0.,1.,0.));
#35487=DIRECTION('',(0.,-1.,0.));
#35488=DIRECTION('',(0.,0.,-1.));
#35489=DIRECTION('center_axis',(-0.707106781186541,0.707106781186554,0.));
#35490=DIRECTION('ref_axis',(0.,0.,1.));
#35491=DIRECTION('',(0.577350269189629,0.577350269189619,-0.577350269189629));
#35492=DIRECTION('',(0.,0.,-1.));
#35493=DIRECTION('',(0.707106781186554,0.707106781186541,0.));
#35494=DIRECTION('center_axis',(0.,0.707106781186554,0.707106781186541));
#35495=DIRECTION('ref_axis',(1.,0.,0.));
#35496=DIRECTION('',(-1.,0.,0.));
#35497=DIRECTION('center_axis',(0.,1.,0.));
#35498=DIRECTION('ref_axis',(-1.,0.,0.));
#35499=DIRECTION('',(-1.,0.,0.));
#35500=DIRECTION('',(0.,0.,1.));
#35501=DIRECTION('',(1.,0.,0.));
#35502=DIRECTION('center_axis',(0.,1.,0.));
#35503=DIRECTION('ref_axis',(1.,0.,0.));
#35504=DIRECTION('center_axis',(0.,1.,0.));
#35505=DIRECTION('ref_axis',(1.,0.,0.));
#35506=DIRECTION('center_axis',(0.707106781186566,0.707106781186529,0.));
#35507=DIRECTION('ref_axis',(0.,0.,-1.));
#35508=DIRECTION('',(0.707106781186529,-0.707106781186566,0.));
#35509=DIRECTION('',(0.577350269189602,-0.577350269189633,0.577350269189643));
#35510=DIRECTION('center_axis',(0.,0.707106781186554,0.707106781186541));
#35511=DIRECTION('ref_axis',(1.,0.,0.));
#35512=DIRECTION('center_axis',(0.707106781186541,-0.707106781186554,0.));
#35513=DIRECTION('ref_axis',(0.,0.,-1.));
#35514=DIRECTION('',(-0.577350269189629,-0.577350269189619,-0.577350269189629));
#35515=DIRECTION('',(0.,0.,-1.));
#35516=DIRECTION('',(-0.707106781186554,-0.707106781186541,0.));
#35517=DIRECTION('',(0.,0.,1.));
#35518=DIRECTION('center_axis',(0.,-0.707106781186554,0.707106781186541));
#35519=DIRECTION('ref_axis',(1.,0.,0.));
#35520=DIRECTION('',(1.,0.,0.));
#35521=DIRECTION('center_axis',(0.,-1.,0.));
#35522=DIRECTION('ref_axis',(1.,0.,0.));
#35523=DIRECTION('',(0.,0.,-1.));
#35524=DIRECTION('',(-1.,0.,0.));
#35525=DIRECTION('center_axis',(0.,-1.,0.));
#35526=DIRECTION('ref_axis',(1.,0.,0.));
#35527=DIRECTION('center_axis',(0.,-1.,0.));
#35528=DIRECTION('ref_axis',(1.,0.,0.));
#35529=DIRECTION('center_axis',(-1.,0.,0.));
#35530=DIRECTION('ref_axis',(0.,-1.,0.));
#35531=DIRECTION('',(0.,0.,1.));
#35532=DIRECTION('',(0.,1.,0.));
#35533=DIRECTION('center_axis',(-0.707106781186541,0.707106781186554,0.));
#35534=DIRECTION('ref_axis',(0.,0.,1.));
#35535=DIRECTION('',(0.,0.,-1.));
#35536=DIRECTION('',(0.707106781186554,0.707106781186541,0.));
#35537=DIRECTION('center_axis',(1.,0.,0.));
#35538=DIRECTION('ref_axis',(0.,1.,0.));
#35539=DIRECTION('',(0.,-1.,0.));
#35540=DIRECTION('center_axis',(0.,1.,0.));
#35541=DIRECTION('ref_axis',(1.,0.,0.));
#35542=DIRECTION('center_axis',(0.,1.,0.));
#35543=DIRECTION('ref_axis',(1.,0.,0.));
#35544=DIRECTION('',(0.707106781186554,-0.707106781186541,-8.65956056235501E-17));
#35545=DIRECTION('center_axis',(0.,-1.,0.));
#35546=DIRECTION('ref_axis',(1.,0.,0.));
#35547=DIRECTION('center_axis',(0.,1.,0.));
#35548=DIRECTION('ref_axis',(1.,0.,0.));
#35549=DIRECTION('center_axis',(0.,1.,0.));
#35550=DIRECTION('ref_axis',(1.,0.,0.));
#35551=DIRECTION('',(0.,1.,0.));
#35552=DIRECTION('center_axis',(0.,1.,0.));
#35553=DIRECTION('ref_axis',(-1.,0.,0.));
#35554=DIRECTION('',(1.,0.,0.));
#35555=DIRECTION('center_axis',(0.,1.,0.));
#35556=DIRECTION('ref_axis',(1.,0.,0.));
#35557=DIRECTION('center_axis',(0.,-1.,0.));
#35558=DIRECTION('ref_axis',(1.,0.,0.));
#35559=DIRECTION('',(0.707106781186554,0.707106781186541,8.65956056235501E-17));
#35560=DIRECTION('center_axis',(0.,1.,0.));
#35561=DIRECTION('ref_axis',(1.,0.,0.));
#35562=DIRECTION('',(0.707106781186554,-0.707106781186541,-8.65956056235501E-17));
#35563=DIRECTION('center_axis',(0.,-1.,0.));
#35564=DIRECTION('ref_axis',(1.,0.,0.));
#35565=DIRECTION('center_axis',(0.,1.,0.));
#35566=DIRECTION('ref_axis',(1.,0.,0.));
#35567=DIRECTION('center_axis',(0.,1.,0.));
#35568=DIRECTION('ref_axis',(1.,0.,0.));
#35569=DIRECTION('',(0.,1.,0.));
#35570=DIRECTION('center_axis',(0.,-1.,0.));
#35571=DIRECTION('ref_axis',(1.,0.,0.));
#35572=DIRECTION('center_axis',(0.,-1.,0.));
#35573=DIRECTION('ref_axis',(1.,0.,0.));
#35574=DIRECTION('',(0.707106781186554,0.707106781186541,8.65956056235501E-17));
#35575=DIRECTION('center_axis',(0.,-1.,0.));
#35576=DIRECTION('ref_axis',(1.,0.,0.));
#35577=DIRECTION('',(-1.,0.,0.));
#35578=DIRECTION('center_axis',(0.,-1.,0.));
#35579=DIRECTION('ref_axis',(1.,0.,0.));
#35580=DIRECTION('center_axis',(0.,1.,0.));
#35581=DIRECTION('ref_axis',(1.,0.,0.));
#35582=DIRECTION('',(0.707106781186554,-0.707106781186541,-8.65956056235501E-17));
#35583=DIRECTION('center_axis',(0.,-1.,0.));
#35584=DIRECTION('ref_axis',(1.,0.,0.));
#35585=DIRECTION('center_axis',(0.,1.,0.));
#35586=DIRECTION('ref_axis',(1.,0.,0.));
#35587=DIRECTION('center_axis',(0.,1.,0.));
#35588=DIRECTION('ref_axis',(1.,0.,0.));
#35589=DIRECTION('',(0.,1.,0.));
#35590=DIRECTION('center_axis',(0.,-1.,0.));
#35591=DIRECTION('ref_axis',(1.,0.,0.));
#35592=DIRECTION('',(0.707106781186554,0.707106781186541,8.65956056235501E-17));
#35593=DIRECTION('center_axis',(0.,1.,0.));
#35594=DIRECTION('ref_axis',(1.,0.,0.));
#35595=DIRECTION('',(0.707106781186554,-0.707106781186541,-8.65956056235501E-17));
#35596=DIRECTION('center_axis',(0.,-1.,0.));
#35597=DIRECTION('ref_axis',(1.,0.,0.));
#35598=DIRECTION('center_axis',(0.,1.,0.));
#35599=DIRECTION('ref_axis',(1.,0.,0.));
#35600=DIRECTION('center_axis',(0.,1.,0.));
#35601=DIRECTION('ref_axis',(1.,0.,0.));
#35602=DIRECTION('',(0.,1.,0.));
#35603=DIRECTION('center_axis',(0.,-1.,0.));
#35604=DIRECTION('ref_axis',(1.,0.,0.));
#35605=DIRECTION('',(0.707106781186554,0.707106781186541,8.65956056235501E-17));
#35606=DIRECTION('center_axis',(0.,0.,-1.));
#35607=DIRECTION('ref_axis',(1.,0.,0.));
#35608=DIRECTION('',(0.707106781186553,-8.65956056235499E-17,0.707106781186543));
#35609=DIRECTION('center_axis',(0.,0.,1.));
#35610=DIRECTION('ref_axis',(1.,0.,0.));
#35611=DIRECTION('center_axis',(0.,0.,1.));
#35612=DIRECTION('ref_axis',(1.,0.,0.));
#35613=DIRECTION('',(0.,0.,1.));
#35614=DIRECTION('center_axis',(0.,0.,-1.));
#35615=DIRECTION('ref_axis',(1.,0.,0.));
#35616=DIRECTION('center_axis',(0.,0.,-1.));
#35617=DIRECTION('ref_axis',(1.,0.,0.));
#35618=DIRECTION('',(0.707106781186553,-8.65956056235499E-17,0.707106781186543));
#35619=DIRECTION('center_axis',(0.,0.,1.));
#35620=DIRECTION('ref_axis',(1.,0.,0.));
#35621=DIRECTION('center_axis',(0.,0.,1.));
#35622=DIRECTION('ref_axis',(1.,0.,0.));
#35623=DIRECTION('',(0.,0.,1.));
#35624=DIRECTION('center_axis',(0.,0.,-1.));
#35625=DIRECTION('ref_axis',(1.,0.,0.));
#35626=DIRECTION('center_axis',(0.,-0.382683432365109,0.923879532511279));
#35627=DIRECTION('ref_axis',(1.,0.,0.));
#35628=DIRECTION('',(-1.,0.,0.));
#35629=DIRECTION('',(0.,-0.92387953251128,-0.382683432365107));
#35630=DIRECTION('',(1.,0.,0.));
#35631=DIRECTION('center_axis',(0.,0.,-1.));
#35632=DIRECTION('ref_axis',(-0.707106781186547,-0.707106781186547,0.));
#35633=DIRECTION('',(-0.923879532511284,0.,-0.382683432365098));
#35634=DIRECTION('center_axis',(0.,0.,1.));
#35635=DIRECTION('ref_axis',(-0.707106781186548,-0.707106781186548,0.));
#35636=DIRECTION('center_axis',(0.,0.,-1.));
#35637=DIRECTION('ref_axis',(-0.707106781186547,-0.707106781186547,0.));
#35638=DIRECTION('center_axis',(-0.382683432365094,0.,0.923879532511285));
#35639=DIRECTION('ref_axis',(0.923879532511285,0.,0.382683432365094));
#35640=DIRECTION('',(-0.923879532511286,0.,-0.382683432365091));
#35641=DIRECTION('',(0.,-1.,0.));
#35642=DIRECTION('',(0.,1.,0.));
#35643=DIRECTION('center_axis',(0.,0.,-1.));
#35644=DIRECTION('ref_axis',(-0.707106781186547,0.707106781186547,0.));
#35645=DIRECTION('',(0.,0.923879532511284,-0.382683432365098));
#35646=DIRECTION('center_axis',(0.,0.,1.));
#35647=DIRECTION('ref_axis',(-0.707106781186548,0.707106781186548,0.));
#35648=DIRECTION('center_axis',(0.,0.,-1.));
#35649=DIRECTION('ref_axis',(-0.707106781186547,0.707106781186547,0.));
#35650=DIRECTION('center_axis',(0.,0.382683432365109,0.923879532511279));
#35651=DIRECTION('ref_axis',(1.,0.,0.));
#35652=DIRECTION('',(-1.,0.,0.));
#35653=DIRECTION('',(1.,0.,0.));
#35654=DIRECTION('center_axis',(0.,0.,1.));
#35655=DIRECTION('ref_axis',(1.,0.,0.));
#35656=DIRECTION('',(0.,-1.,0.));
#35657=DIRECTION('',(-1.,0.,0.));
#35658=DIRECTION('center_axis',(0.,0.,-1.));
#35659=DIRECTION('ref_axis',(0.707106781186548,-0.707106781186548,0.));
#35660=DIRECTION('',(0.,-1.,0.));
#35661=DIRECTION('center_axis',(0.,0.,-1.));
#35662=DIRECTION('ref_axis',(0.707106781186548,0.707106781186548,0.));
#35663=DIRECTION('',(1.,0.,0.));
#35664=DIRECTION('center_axis',(0.,0.,1.));
#35665=DIRECTION('ref_axis',(1.,0.,0.));
#35666=DIRECTION('center_axis',(0.,0.,1.));
#35667=DIRECTION('ref_axis',(1.,0.,0.));
#35668=DIRECTION('center_axis',(0.,0.382683432365109,0.923879532511279));
#35669=DIRECTION('ref_axis',(1.,0.,0.));
#35670=DIRECTION('',(0.,0.923879532511282,-0.382683432365102));
#35671=DIRECTION('',(-1.,0.,0.));
#35672=DIRECTION('center_axis',(0.,0.,-1.));
#35673=DIRECTION('ref_axis',(0.707106781186547,0.707106781186548,0.));
#35674=DIRECTION('',(0.923879532511287,1.92271478790291E-14,-0.38268343236509));
#35675=DIRECTION('center_axis',(0.,0.,1.));
#35676=DIRECTION('ref_axis',(0.707106781186546,0.707106781186549,0.));
#35677=DIRECTION('center_axis',(0.382683432365089,0.,0.923879532511287));
#35678=DIRECTION('ref_axis',(0.923879532511287,0.,-0.382683432365089));
#35679=DIRECTION('',(0.923879532511287,0.,-0.38268343236509));
#35680=DIRECTION('',(0.,1.,0.));
#35681=DIRECTION('center_axis',(0.,0.,-1.));
#35682=DIRECTION('ref_axis',(0.707106781186547,-0.707106781186548,0.));
#35683=DIRECTION('',(0.,-0.923879532511287,-0.38268343236509));
#35684=DIRECTION('center_axis',(0.,0.,1.));
#35685=DIRECTION('ref_axis',(0.707106781186546,-0.707106781186549,0.));
#35686=DIRECTION('center_axis',(0.,-0.382683432365109,0.923879532511279));
#35687=DIRECTION('ref_axis',(1.,0.,0.));
#35688=DIRECTION('',(0.,0.923879532511279,0.382683432365109));
#35689=DIRECTION('',(1.,0.,0.));
#35690=DIRECTION('center_axis',(0.,0.,1.));
#35691=DIRECTION('ref_axis',(1.,0.,0.));
#35692=DIRECTION('',(0.707106781186553,8.65956056235499E-17,-0.707106781186542));
#35693=DIRECTION('center_axis',(0.,0.,1.));
#35694=DIRECTION('ref_axis',(1.,0.,0.));
#35695=DIRECTION('',(0.707106781186553,8.65956056235499E-17,-0.707106781186542));
#35696=DIRECTION('center_axis',(0.,-0.75482962115391,0.655920912175122));
#35697=DIRECTION('ref_axis',(0.,-0.655920912175122,-0.75482962115391));
#35698=DIRECTION('',(-1.,0.,0.));
#35699=DIRECTION('center_axis',(0.,0.,-1.));
#35700=DIRECTION('ref_axis',(0.,1.,0.));
#35701=DIRECTION('',(-1.,0.,0.));
#35702=DIRECTION('',(0.,1.,0.));
#35703=DIRECTION('center_axis',(1.,0.,0.));
#35704=DIRECTION('ref_axis',(0.,0.,-1.));
#35705=DIRECTION('',(0.,-0.707106781186546,-0.707106781186549));
#35706=DIRECTION('center_axis',(0.,0.,-1.));
#35707=DIRECTION('ref_axis',(-0.707106781186548,-0.707106781186548,0.));
#35708=DIRECTION('',(-0.707106781186553,0.,-0.707106781186542));
#35709=DIRECTION('',(0.,0.707106781186553,0.707106781186542));
#35710=DIRECTION('center_axis',(-0.707106781186549,0.,0.707106781186546));
#35711=DIRECTION('ref_axis',(0.707106781186546,0.,0.707106781186549));
#35712=DIRECTION('',(-0.707106781186546,0.,-0.707106781186549));
#35713=DIRECTION('center_axis',(0.,0.,-1.));
#35714=DIRECTION('ref_axis',(-0.707106781186548,0.707106781186548,0.));
#35715=DIRECTION('',(0.,0.707106781186553,-0.707106781186542));
#35716=DIRECTION('center_axis',(0.,0.707106781186549,0.707106781186546));
#35717=DIRECTION('ref_axis',(1.,0.,0.));
#35718=DIRECTION('',(0.,0.707106781186546,-0.707106781186549));
#35719=DIRECTION('center_axis',(0.,0.,-1.));
#35720=DIRECTION('ref_axis',(0.707106781186548,0.707106781186548,0.));
#35721=DIRECTION('',(0.707106781186553,0.,-0.707106781186542));
#35722=DIRECTION('center_axis',(0.,0.,1.));
#35723=DIRECTION('ref_axis',(0.707106781186547,0.707106781186547,0.));
#35724=DIRECTION('center_axis',(0.707106781186542,0.,0.707106781186553));
#35725=DIRECTION('ref_axis',(0.707106781186553,0.,-0.707106781186542));
#35726=DIRECTION('',(0.707106781186553,0.,-0.707106781186542));
#35727=DIRECTION('',(0.,1.,0.));
#35728=DIRECTION('center_axis',(0.,0.,-1.));
#35729=DIRECTION('ref_axis',(0.707106781186548,-0.707106781186548,0.));
#35730=DIRECTION('',(0.,-0.707106781186553,-0.707106781186542));
#35731=DIRECTION('center_axis',(0.,0.,1.));
#35732=DIRECTION('ref_axis',(0.707106781186547,-0.707106781186547,0.));
#35733=DIRECTION('center_axis',(0.,-0.707106781186549,0.707106781186546));
#35734=DIRECTION('ref_axis',(1.,0.,0.));
#35735=DIRECTION('',(1.,0.,0.));
#35736=DIRECTION('center_axis',(1.,0.,0.));
#35737=DIRECTION('ref_axis',(0.,1.,0.));
#35738=DIRECTION('',(0.,0.,-1.));
#35739=DIRECTION('',(0.,0.,1.));
#35740=DIRECTION('center_axis',(0.,0.,1.));
#35741=DIRECTION('ref_axis',(0.707106781186547,-0.707106781186547,0.));
#35742=DIRECTION('',(0.,0.,-1.));
#35743=DIRECTION('center_axis',(0.,-1.,0.));
#35744=DIRECTION('ref_axis',(1.,0.,0.));
#35745=DIRECTION('center_axis',(0.,0.,1.));
#35746=DIRECTION('ref_axis',(0.707106781186547,0.707106781186547,0.));
#35747=DIRECTION('axis',(0.,0.,1.));
#35748=DIRECTION('refdir',(1.,0.,0.));
#35749=DIRECTION('center_axis',(-1.,0.,0.));
#35750=DIRECTION('ref_axis',(0.,0.,1.));
#35751=DIRECTION('center_axis',(0.,-1.,1.22464679914735E-16));
#35752=DIRECTION('ref_axis',(0.,-1.22464679914735E-16,-1.));
#35753=DIRECTION('center_axis',(1.,0.,0.));
#35754=DIRECTION('ref_axis',(0.,0.,1.));
#35755=DIRECTION('center_axis',(0.,0.,1.));
#35756=DIRECTION('ref_axis',(1.,0.,0.));
#35757=DIRECTION('center_axis',(0.,0.,1.));
#35758=DIRECTION('ref_axis',(1.,0.,0.));
#35759=DIRECTION('center_axis',(0.,0.,1.));
#35760=DIRECTION('ref_axis',(6.9217303377289E-15,1.,0.));
#35761=DIRECTION('center_axis',(0.,0.,1.));
#35762=DIRECTION('ref_axis',(1.,0.,0.));
#35763=DIRECTION('center_axis',(0.,0.,1.));
#35764=DIRECTION('ref_axis',(1.,0.,0.));
#35765=DIRECTION('center_axis',(-0.998217224866142,-0.00840157766811335,
0.0590913316250743));
#35766=DIRECTION('ref_axis',(0.059089238754932,0.000497329455335615,0.998252580525979));
#35767=DIRECTION('center_axis',(-0.998217224866142,-0.00840157766811335,
0.0590913316250743));
#35768=DIRECTION('ref_axis',(0.059089238754932,0.000497329455335615,0.998252580525979));
#35769=DIRECTION('center_axis',(-1.,0.,0.));
#35770=DIRECTION('ref_axis',(0.,0.,1.));
#35771=DIRECTION('center_axis',(0.,-1.,1.22464679914735E-16));
#35772=DIRECTION('ref_axis',(0.,-1.22464679914735E-16,-1.));
#35773=DIRECTION('center_axis',(1.,0.,0.));
#35774=DIRECTION('ref_axis',(0.,0.,1.));
#35775=DIRECTION('center_axis',(0.,0.,1.));
#35776=DIRECTION('ref_axis',(1.,0.,0.));
#35777=DIRECTION('center_axis',(-0.998217224843264,0.00840157766999991,
0.059091332011291));
#35778=DIRECTION('ref_axis',(0.0434273377103988,0.781407112236281,0.622508627479124));
#35779=DIRECTION('',(0.00841628444953835,0.999964582450831,0.));
#35780=DIRECTION('center_axis',(-0.998217224843264,0.00840157766999991,
0.059091332011291));
#35781=DIRECTION('ref_axis',(0.0434273377103987,0.781407112236281,0.622508627479124));
#35782=DIRECTION('center_axis',(0.,0.,1.));
#35783=DIRECTION('ref_axis',(1.,0.,0.));
#35784=DIRECTION('center_axis',(0.,0.,1.));
#35785=DIRECTION('ref_axis',(1.,0.,0.));
#35786=DIRECTION('center_axis',(0.,0.,1.));
#35787=DIRECTION('ref_axis',(-0.116141449894828,0.993232683522007,0.));
#35788=DIRECTION('axis',(0.,0.,1.));
#35789=DIRECTION('refdir',(1.,0.,0.));
#35790=DIRECTION('center_axis',(0.,0.,1.));
#35791=DIRECTION('ref_axis',(1.,0.,0.));
#35792=DIRECTION('',(0.,0.,-1.));
#35793=DIRECTION('center_axis',(0.,0.,1.));
#35794=DIRECTION('ref_axis',(1.,0.,0.));
#35795=DIRECTION('center_axis',(0.,0.,1.));
#35796=DIRECTION('ref_axis',(1.,0.,0.));
#35797=DIRECTION('',(0.,0.,-1.));
#35798=DIRECTION('center_axis',(0.,0.,1.));
#35799=DIRECTION('ref_axis',(1.,0.,0.));
#35800=DIRECTION('',(0.,0.,-1.));
#35801=DIRECTION('center_axis',(0.,0.,1.));
#35802=DIRECTION('ref_axis',(1.,0.,0.));
#35803=DIRECTION('',(0.,0.,-1.));
#35804=DIRECTION('center_axis',(0.,0.,1.));
#35805=DIRECTION('ref_axis',(1.,0.,0.));
#35806=DIRECTION('',(0.,0.,-1.));
#35807=DIRECTION('center_axis',(0.,0.,1.));
#35808=DIRECTION('ref_axis',(1.,0.,0.));
#35809=DIRECTION('',(0.,0.,-1.));
#35810=DIRECTION('center_axis',(0.,0.,1.));
#35811=DIRECTION('ref_axis',(1.,0.,0.));
#35812=DIRECTION('',(0.,0.,-1.));
#35813=DIRECTION('center_axis',(0.,0.,1.));
#35814=DIRECTION('ref_axis',(1.,0.,0.));
#35815=DIRECTION('',(0.,0.,-1.));
#35816=DIRECTION('center_axis',(0.,0.,1.));
#35817=DIRECTION('ref_axis',(1.,0.,0.));
#35818=DIRECTION('',(0.,0.,-1.));
#35819=DIRECTION('center_axis',(0.,0.,1.));
#35820=DIRECTION('ref_axis',(1.,0.,0.));
#35821=DIRECTION('',(0.,0.,-1.));
#35822=DIRECTION('center_axis',(0.,0.,1.));
#35823=DIRECTION('ref_axis',(1.,0.,0.));
#35824=DIRECTION('',(0.,0.,-1.));
#35825=DIRECTION('center_axis',(0.,0.,1.));
#35826=DIRECTION('ref_axis',(1.,5.61770717067589E-14,0.));
#35827=DIRECTION('',(0.,0.,1.));
#35828=DIRECTION('center_axis',(0.,0.,-1.));
#35829=DIRECTION('ref_axis',(1.,5.61770717067589E-14,0.));
#35830=DIRECTION('center_axis',(0.,0.,1.));
#35831=DIRECTION('ref_axis',(1.,5.61770717067589E-14,0.));
#35832=DIRECTION('',(0.,0.,1.));
#35833=DIRECTION('center_axis',(0.,0.,1.));
#35834=DIRECTION('ref_axis',(1.,5.61770717067589E-14,0.));
#35835=DIRECTION('',(0.,0.,1.));
#35836=DIRECTION('center_axis',(0.,0.,1.));
#35837=DIRECTION('ref_axis',(1.,5.61770717067589E-14,0.));
#35838=DIRECTION('',(0.,0.,1.));
#35839=DIRECTION('center_axis',(0.,0.,1.));
#35840=DIRECTION('ref_axis',(1.,5.61770717067589E-14,0.));
#35841=DIRECTION('',(0.,0.,1.));
#35842=DIRECTION('center_axis',(0.,0.,1.));
#35843=DIRECTION('ref_axis',(1.,5.61770717067589E-14,0.));
#35844=DIRECTION('',(0.,0.,1.));
#35845=DIRECTION('center_axis',(0.,0.,1.));
#35846=DIRECTION('ref_axis',(1.,5.61770717067589E-14,0.));
#35847=DIRECTION('',(0.,0.,1.));
#35848=DIRECTION('center_axis',(0.,0.,1.));
#35849=DIRECTION('ref_axis',(1.,5.61770717067589E-14,0.));
#35850=DIRECTION('',(0.,0.,1.));
#35851=DIRECTION('center_axis',(0.,0.,1.));
#35852=DIRECTION('ref_axis',(1.,5.61770717067589E-14,0.));
#35853=DIRECTION('',(0.,0.,1.));
#35854=DIRECTION('center_axis',(0.,0.,1.));
#35855=DIRECTION('ref_axis',(1.,5.61770717067589E-14,0.));
#35856=DIRECTION('',(0.,0.,1.));
#35857=DIRECTION('center_axis',(0.,0.,1.));
#35858=DIRECTION('ref_axis',(1.,5.61770717067589E-14,0.));
#35859=DIRECTION('',(0.,0.,1.));
#35860=DIRECTION('center_axis',(0.,1.,0.));
#35861=DIRECTION('ref_axis',(0.,0.,1.));
#35862=DIRECTION('center_axis',(-1.,0.,1.22464679914735E-16));
#35863=DIRECTION('ref_axis',(-1.22464679914735E-16,0.,-1.));
#35864=DIRECTION('center_axis',(-1.,0.,1.22464679914735E-16));
#35865=DIRECTION('ref_axis',(-1.22464679914735E-16,0.,-1.));
#35866=DIRECTION('center_axis',(0.,-1.,0.));
#35867=DIRECTION('ref_axis',(0.,0.,1.));
#35868=DIRECTION('center_axis',(0.,0.,1.));
#35869=DIRECTION('ref_axis',(1.,0.,0.));
#35870=DIRECTION('center_axis',(0.,0.,1.));
#35871=DIRECTION('ref_axis',(1.,0.,0.));
#35872=DIRECTION('center_axis',(0.,0.,-1.));
#35873=DIRECTION('ref_axis',(1.,0.,0.));
#35874=DIRECTION('center_axis',(0.,0.,-1.));
#35875=DIRECTION('ref_axis',(1.,0.,0.));
#35876=DIRECTION('center_axis',(0.,0.,1.));
#35877=DIRECTION('ref_axis',(1.,0.,0.));
#35878=DIRECTION('center_axis',(0.,0.,1.));
#35879=DIRECTION('ref_axis',(1.,0.,0.));
#35880=DIRECTION('center_axis',(0.,0.,-1.));
#35881=DIRECTION('ref_axis',(1.,0.,0.));
#35882=DIRECTION('center_axis',(0.,0.,-1.));
#35883=DIRECTION('ref_axis',(1.,0.,0.));
#35884=DIRECTION('center_axis',(0.,0.,1.));
#35885=DIRECTION('ref_axis',(1.,0.,0.));
#35886=DIRECTION('center_axis',(0.,0.,1.));
#35887=DIRECTION('ref_axis',(1.,0.,0.));
#35888=DIRECTION('center_axis',(0.,0.,-1.));
#35889=DIRECTION('ref_axis',(-1.,0.,0.));
#35890=DIRECTION('center_axis',(0.,0.,1.));
#35891=DIRECTION('ref_axis',(1.,0.,0.));
#35892=DIRECTION('center_axis',(0.,0.,-1.));
#35893=DIRECTION('ref_axis',(1.,0.,0.));
#35894=DIRECTION('center_axis',(0.,0.,1.));
#35895=DIRECTION('ref_axis',(1.,0.,0.));
#35896=DIRECTION('center_axis',(0.,0.,1.));
#35897=DIRECTION('ref_axis',(1.,0.,0.));
#35898=DIRECTION('',(0.,0.,-1.));
#35899=DIRECTION('center_axis',(0.,0.,-1.));
#35900=DIRECTION('ref_axis',(1.,0.,0.));
#35901=DIRECTION('',(-0.707106781186547,-8.65956056235493E-17,-0.707106781186548));
#35902=DIRECTION('center_axis',(0.,0.,1.));
#35903=DIRECTION('ref_axis',(1.,5.61770717067589E-14,0.));
#35904=DIRECTION('center_axis',(0.,0.,-1.));
#35905=DIRECTION('ref_axis',(1.,5.61770717067589E-14,0.));
#35906=DIRECTION('center_axis',(0.,0.,1.));
#35907=DIRECTION('ref_axis',(1.,0.,0.));
#35908=DIRECTION('center_axis',(0.,0.,1.));
#35909=DIRECTION('ref_axis',(1.,0.,0.));
#35910=DIRECTION('center_axis',(0.,0.,1.));
#35911=DIRECTION('ref_axis',(1.,0.,0.));
#35912=DIRECTION('center_axis',(0.,0.,-1.));
#35913=DIRECTION('ref_axis',(-1.,0.,0.));
#35914=DIRECTION('center_axis',(0.,0.,1.));
#35915=DIRECTION('ref_axis',(1.,0.,0.));
#35916=DIRECTION('center_axis',(0.,0.,1.));
#35917=DIRECTION('ref_axis',(1.,0.,0.));
#35918=DIRECTION('',(0.707106781186547,8.65956056235493E-17,-0.707106781186548));
#35919=DIRECTION('center_axis',(0.,0.,1.));
#35920=DIRECTION('ref_axis',(1.,0.,0.));
#35921=DIRECTION('axis',(0.,0.,1.));
#35922=DIRECTION('refdir',(1.,0.,0.));
#35923=DIRECTION('center_axis',(0.,0.707106781186522,-0.707106781186573));
#35924=DIRECTION('ref_axis',(-1.,0.,0.));
#35925=DIRECTION('',(0.577350269189634,0.577350269189642,0.577350269189601));
#35926=DIRECTION('',(1.,0.,0.));
#35927=DIRECTION('',(0.577350269189633,-0.577350269189643,-0.577350269189602));
#35928=DIRECTION('',(-0.577350269189594,-0.577350269189662,-0.577350269189621));
#35929=DIRECTION('',(-1.,0.,0.));
#35930=DIRECTION('',(-0.577350269189598,0.57735026918966,0.577350269189619));
#35931=DIRECTION('center_axis',(0.,0.,-1.));
#35932=DIRECTION('ref_axis',(-1.,0.,0.));
#35933=DIRECTION('',(0.,1.,0.));
#35934=DIRECTION('',(1.,0.,0.));
#35935=DIRECTION('',(0.,-1.,0.));
#35936=DIRECTION('center_axis',(0.707106781186564,0.,-0.707106781186531));
#35937=DIRECTION('ref_axis',(-0.707106781186531,0.,-0.707106781186564));
#35938=DIRECTION('',(-0.577350269189613,0.577350269189624,-0.577350269189641));
#35939=DIRECTION('',(0.,-1.,0.));
#35940=DIRECTION('',(0.577350269189613,0.577350269189624,0.577350269189641));
#35941=DIRECTION('',(0.577350269189594,-0.577350269189662,0.577350269189621));
#35942=DIRECTION('center_axis',(0.707106781186554,0.707106781186541,0.));
#35943=DIRECTION('ref_axis',(0.,0.,-1.));
#35944=DIRECTION('',(0.,0.,1.));
#35945=DIRECTION('',(0.577350269189633,-0.577350269189643,0.577350269189602));
#35946=DIRECTION('',(0.577350269189615,-0.577350269189626,-0.577350269189636));
#35947=DIRECTION('',(0.,0.,-1.));
#35948=DIRECTION('center_axis',(0.,1.,0.));
#35949=DIRECTION('ref_axis',(0.,0.,1.));
#35950=DIRECTION('',(0.,0.,-1.));
#35951=DIRECTION('',(-0.70710678118655,0.,-0.707106781186545));
#35952=DIRECTION('',(0.70710678118655,0.,-0.707106781186545));
#35953=DIRECTION('',(0.,0.,-1.));
#35954=DIRECTION('',(-1.,0.,0.));
#35955=DIRECTION('',(-0.707106781186548,0.,0.707106781186548));
#35956=DIRECTION('',(-0.707106781186548,0.,-0.707106781186548));
#35957=DIRECTION('',(-1.,0.,0.));
#35958=DIRECTION('center_axis',(1.,0.,0.));
#35959=DIRECTION('ref_axis',(0.,0.,-1.));
#35960=DIRECTION('',(0.,1.,0.));
#35961=DIRECTION('',(0.,0.,1.));
#35962=DIRECTION('center_axis',(-0.499999999999988,0.707106781186564,0.499999999999988));
#35963=DIRECTION('ref_axis',(0.707106781186548,0.,0.707106781186548));
#35964=DIRECTION('',(0.281084637714915,0.678598344545852,-0.678598344545803));
#35965=DIRECTION('',(0.,0.577350269189608,-0.816496580927739));
#35966=DIRECTION('',(0.707106781186548,0.,0.707106781186548));
#35967=DIRECTION('',(0.862856209461028,0.357406744336628,0.357406744336531));
#35968=DIRECTION('center_axis',(0.,0.707106781186522,0.707106781186573));
#35969=DIRECTION('ref_axis',(1.,0.,0.));
#35970=DIRECTION('',(-0.862856209461047,0.357406744336575,-0.357406744336539));
#35971=DIRECTION('',(1.,0.,0.));
#35972=DIRECTION('',(0.577350269189598,0.57735026918966,-0.577350269189619));
#35973=DIRECTION('center_axis',(-0.382683432365029,0.,0.923879532511312));
#35974=DIRECTION('ref_axis',(0.923879532511312,0.,0.382683432365029));
#35975=DIRECTION('',(0.,-1.,0.));
#35976=DIRECTION('',(0.923879532511312,0.,0.382683432365029));
#35977=DIRECTION('',(0.,1.,0.));
#35978=DIRECTION('center_axis',(0.382683432365106,0.,0.92387953251128));
#35979=DIRECTION('ref_axis',(0.92387953251128,0.,-0.382683432365106));
#35980=DIRECTION('',(-0.862856209460998,-0.357406744336628,0.357406744336603));
#35981=DIRECTION('',(0.,-1.,0.));
#35982=DIRECTION('',(0.862856209460998,-0.357406744336628,-0.357406744336603));
#35983=DIRECTION('',(0.86285620946102,0.357406744336566,-0.357406744336612));
#35984=DIRECTION('',(0.,1.,0.));
#35985=DIRECTION('',(-0.86285620946102,0.357406744336566,0.357406744336612));
#35986=DIRECTION('center_axis',(0.,0.,1.));
#35987=DIRECTION('ref_axis',(1.,0.,0.));
#35988=DIRECTION('',(1.,0.,0.));
#35989=DIRECTION('',(0.,1.,0.));
#35990=DIRECTION('',(-1.,0.,0.));
#35991=DIRECTION('center_axis',(0.,0.707106781186522,0.707106781186573));
#35992=DIRECTION('ref_axis',(1.,0.,0.));
#35993=DIRECTION('',(0.281084637714926,-0.678598344545849,0.678598344545801));
#35994=DIRECTION('',(-0.577350269189634,-0.577350269189642,0.577350269189601));
#35995=DIRECTION('',(0.577350269189597,-0.577350269189661,0.57735026918962));
#35996=DIRECTION('center_axis',(0.499999999999988,0.707106781186564,0.499999999999988));
#35997=DIRECTION('ref_axis',(0.707106781186548,0.,-0.707106781186548));
#35998=DIRECTION('',(0.707106781186548,0.,-0.707106781186548));
#35999=DIRECTION('center_axis',(0.707106781186548,0.,0.707106781186548));
#36000=DIRECTION('ref_axis',(0.707106781186548,0.,-0.707106781186548));
#36001=DIRECTION('',(-0.707106781186548,0.,0.707106781186548));
#36002=DIRECTION('',(0.,1.,0.));
#36003=DIRECTION('center_axis',(-0.707106781186561,0.,0.707106781186534));
#36004=DIRECTION('ref_axis',(0.707106781186534,0.,0.707106781186561));
#36005=DIRECTION('',(0.577350269189616,0.577350269189624,0.577350269189638));
#36006=DIRECTION('',(0.,-1.,0.));
#36007=DIRECTION('',(-0.577350269189616,0.577350269189624,-0.577350269189638));
#36008=DIRECTION('',(-0.577350269189597,-0.577350269189661,-0.57735026918962));
#36009=DIRECTION('center_axis',(0.,-0.707106781186522,0.707106781186573));
#36010=DIRECTION('ref_axis',(1.,0.,0.));
#36011=DIRECTION('',(0.577350269189634,-0.577350269189642,-0.577350269189601));
#36012=DIRECTION('',(1.,0.,0.));
#36013=DIRECTION('',(0.281084637714926,0.678598344545849,0.678598344545801));
#36014=DIRECTION('center_axis',(0.499999999999988,-0.707106781186564,0.499999999999988));
#36015=DIRECTION('ref_axis',(0.707106781186548,0.,-0.707106781186548));
#36016=DIRECTION('',(0.707106781186548,0.,-0.707106781186548));
#36017=DIRECTION('',(-1.02558009940453E-14,0.577350269189613,0.816496580927735));
#36018=DIRECTION('center_axis',(-0.313549377219788,-0.573302186256024,0.756975158957774));
#36019=DIRECTION('ref_axis',(0.923879532511309,0.,0.382683432365036));
#36020=DIRECTION('',(-0.732537816328754,0.653281482438167,0.191341716182569));
#36021=DIRECTION('',(-0.38268343236507,-0.653281482438217,-0.653281482438171));
#36022=DIRECTION('center_axis',(-0.499999999999988,-0.707106781186564,0.499999999999988));
#36023=DIRECTION('ref_axis',(0.707106781186548,0.,0.707106781186548));
#36024=DIRECTION('',(0.707106781186548,0.,0.707106781186548));
#36025=DIRECTION('',(-0.707106781186548,0.,-0.707106781186548));
#36026=DIRECTION('center_axis',(0.,-0.707106781186522,0.707106781186573));
#36027=DIRECTION('ref_axis',(1.,0.,0.));
#36028=DIRECTION('',(-0.577350269189598,0.57735026918966,0.577350269189619));
#36029=DIRECTION('',(-1.,0.,0.));
#36030=DIRECTION('',(1.,0.,0.));
#36031=DIRECTION('',(0.577350269189633,0.577350269189643,0.577350269189602));
#36032=DIRECTION('center_axis',(-0.707106781186552,-0.707106781186543,0.));
#36033=DIRECTION('ref_axis',(0.,0.,1.));
#36034=DIRECTION('',(0.,0.,-1.));
#36035=DIRECTION('',(0.653281482438191,-0.6532814824382,-0.382683432365065));
#36036=DIRECTION('',(0.,0.,1.));
#36037=DIRECTION('center_axis',(-0.707106781186548,0.,0.707106781186548));
#36038=DIRECTION('ref_axis',(0.707106781186548,0.,0.707106781186548));
#36039=DIRECTION('center_axis',(0.707106781186554,-0.707106781186541,0.));
#36040=DIRECTION('ref_axis',(0.,0.,-1.));
#36041=DIRECTION('',(0.,0.,-1.));
#36042=DIRECTION('',(0.577350269189633,0.577350269189643,-0.577350269189602));
#36043=DIRECTION('',(-0.577350269189615,-0.577350269189626,0.577350269189636));
#36044=DIRECTION('center_axis',(0.,-0.707106781186522,-0.707106781186573));
#36045=DIRECTION('ref_axis',(-1.,0.,0.));
#36046=DIRECTION('',(-1.,0.,0.));
#36047=DIRECTION('',(-0.577350269189634,0.577350269189642,-0.577350269189601));
#36048=DIRECTION('',(0.577350269189598,0.57735026918966,-0.577350269189619));
#36049=DIRECTION('center_axis',(-0.70710678118656,0.,-0.707106781186535));
#36050=DIRECTION('ref_axis',(-0.707106781186535,0.,0.70710678118656));
#36051=DIRECTION('',(0.577350269189616,-0.577350269189624,-0.577350269189637));
#36052=DIRECTION('',(0.,1.,0.));
#36053=DIRECTION('',(-0.577350269189616,-0.577350269189624,0.577350269189637));
#36054=DIRECTION('center_axis',(-0.707106781186552,-0.707106781186543,0.));
#36055=DIRECTION('ref_axis',(0.,0.,1.));
#36056=DIRECTION('',(0.,0.,1.));
#36057=DIRECTION('',(-0.653281482438214,0.653281482438223,-0.382683432364986));
#36058=DIRECTION('',(0.,0.,-1.));
#36059=DIRECTION('center_axis',(-0.756975158957757,0.573302186256023,-0.31354937721983));
#36060=DIRECTION('ref_axis',(-0.382683432365087,0.,0.923879532511288));
#36061=DIRECTION('',(0.382683432365099,0.,-0.923879532511283));
#36062=DIRECTION('',(-0.653281482438191,-0.6532814824382,0.382683432365065));
#36063=DIRECTION('',(0.191341716182552,0.653281482438187,0.732537816328741));
#36064=DIRECTION('center_axis',(-0.707106781186552,0.707106781186543,0.));
#36065=DIRECTION('ref_axis',(0.,0.,1.));
#36066=DIRECTION('',(0.,0.,1.));
#36067=DIRECTION('center_axis',(-0.756975158957749,-0.573302186256029,-0.313549377219838));
#36068=DIRECTION('ref_axis',(-0.382683432365099,0.,0.923879532511283));
#36069=DIRECTION('',(-0.382683432365099,0.,0.923879532511283));
#36070=DIRECTION('',(-0.191341716182552,0.653281482438187,-0.732537816328741));
#36071=DIRECTION('center_axis',(-0.923879532511283,0.,-0.382683432365099));
#36072=DIRECTION('ref_axis',(-0.382683432365099,0.,0.923879532511283));
#36073=DIRECTION('',(0.,1.,0.));
#36074=DIRECTION('',(0.,-1.,0.));
#36075=DIRECTION('center_axis',(-0.756975158957738,0.573302186256039,0.313549377219846));
#36076=DIRECTION('ref_axis',(0.382683432365112,0.,0.923879532511278));
#36077=DIRECTION('',(-0.382683432365099,0.,-0.923879532511283));
#36078=DIRECTION('',(-0.191341716182505,-0.653281482438147,0.732537816328789));
#36079=DIRECTION('',(0.653281482438214,0.653281482438223,0.382683432364986));
#36080=DIRECTION('center_axis',(-0.499999999999985,0.707106781186566,0.499999999999989));
#36081=DIRECTION('ref_axis',(0.70710678118655,0.,0.707106781186545));
#36082=DIRECTION('',(0.70710678118655,0.,0.707106781186545));
#36083=DIRECTION('',(0.816496580927738,0.577350269189609,0.));
#36084=DIRECTION('center_axis',(-0.707106781186552,0.707106781186543,0.));
#36085=DIRECTION('ref_axis',(0.,0.,1.));
#36086=DIRECTION('',(0.,0.,1.));
#36087=DIRECTION('center_axis',(-0.756975158957738,-0.573302186256037,0.31354937721985));
#36088=DIRECTION('ref_axis',(0.382683432365116,0.,0.923879532511276));
#36089=DIRECTION('',(0.382683432365099,0.,0.923879532511283));
#36090=DIRECTION('',(0.1913417161825,-0.653281482438148,-0.73253781632879));
#36091=DIRECTION('center_axis',(-0.499999999999985,-0.707106781186566,0.499999999999989));
#36092=DIRECTION('ref_axis',(0.70710678118655,0.,0.707106781186545));
#36093=DIRECTION('',(-0.70710678118655,0.,-0.707106781186545));
#36094=DIRECTION('',(0.70710678118655,0.,0.707106781186545));
#36095=DIRECTION('',(-0.816496580927738,0.577350269189609,0.));
#36096=DIRECTION('center_axis',(-0.923879532511283,0.,0.382683432365099));
#36097=DIRECTION('ref_axis',(0.382683432365099,0.,0.923879532511283));
#36098=DIRECTION('',(0.,-1.,0.));
#36099=DIRECTION('',(0.,1.,0.));
#36100=DIRECTION('center_axis',(-0.499999999999991,-0.707106781186558,-0.499999999999994));
#36101=DIRECTION('ref_axis',(-0.70710678118655,0.,0.707106781186545));
#36102=DIRECTION('',(-0.70710678118655,0.,0.707106781186545));
#36103=DIRECTION('',(0.70710678118655,0.,-0.707106781186545));
#36104=DIRECTION('center_axis',(-0.499999999999991,0.707106781186558,-0.499999999999994));
#36105=DIRECTION('ref_axis',(-0.70710678118655,0.,0.707106781186545));
#36106=DIRECTION('',(-0.70710678118655,0.,0.707106781186545));
#36107=DIRECTION('center_axis',(-1.,0.,0.));
#36108=DIRECTION('ref_axis',(0.,0.,1.));
#36109=DIRECTION('center_axis',(0.,1.,0.));
#36110=DIRECTION('ref_axis',(1.,0.,0.));
#36111=DIRECTION('center_axis',(0.707106781186545,0.,-0.70710678118655));
#36112=DIRECTION('ref_axis',(-0.70710678118655,0.,-0.707106781186545));
#36113=DIRECTION('',(0.,1.,0.));
#36114=DIRECTION('center_axis',(0.707106781186545,0.,0.70710678118655));
#36115=DIRECTION('ref_axis',(0.70710678118655,0.,-0.707106781186545));
#36116=DIRECTION('center_axis',(-1.,0.,0.));
#36117=DIRECTION('ref_axis',(0.,0.,1.));
#36118=DIRECTION('center_axis',(0.70710678118656,0.,0.707106781186535));
#36119=DIRECTION('ref_axis',(0.707106781186535,0.,-0.70710678118656));
#36120=DIRECTION('',(0.,-1.,0.));
#36121=DIRECTION('center_axis',(0.,0.,1.));
#36122=DIRECTION('ref_axis',(1.,0.,0.));
#36123=DIRECTION('axis',(0.,0.,1.));
#36124=DIRECTION('refdir',(1.,0.,0.));
#36125=DIRECTION('center_axis',(0.,0.,1.));
#36126=DIRECTION('ref_axis',(1.,0.,0.));
#36127=DIRECTION('',(0.,0.,-1.));
#36128=DIRECTION('center_axis',(0.,0.,1.));
#36129=DIRECTION('ref_axis',(1.,0.,0.));
#36130=DIRECTION('center_axis',(0.,0.,1.));
#36131=DIRECTION('ref_axis',(1.,0.,0.));
#36132=DIRECTION('',(0.,0.,-1.));
#36133=DIRECTION('center_axis',(0.,0.,1.));
#36134=DIRECTION('ref_axis',(1.,0.,0.));
#36135=DIRECTION('',(0.,0.,-1.));
#36136=DIRECTION('center_axis',(0.,0.,1.));
#36137=DIRECTION('ref_axis',(1.,0.,0.));
#36138=DIRECTION('',(0.,0.,-1.));
#36139=DIRECTION('center_axis',(0.,0.,1.));
#36140=DIRECTION('ref_axis',(1.,0.,0.));
#36141=DIRECTION('',(0.,0.,-1.));
#36142=DIRECTION('center_axis',(0.,0.,1.));
#36143=DIRECTION('ref_axis',(1.,0.,0.));
#36144=DIRECTION('',(0.,0.,-1.));
#36145=DIRECTION('center_axis',(0.,0.,1.));
#36146=DIRECTION('ref_axis',(1.,0.,0.));
#36147=DIRECTION('',(0.,0.,-1.));
#36148=DIRECTION('center_axis',(0.,0.,1.));
#36149=DIRECTION('ref_axis',(1.,0.,0.));
#36150=DIRECTION('',(0.,0.,-1.));
#36151=DIRECTION('center_axis',(0.,0.,1.));
#36152=DIRECTION('ref_axis',(1.,0.,0.));
#36153=DIRECTION('',(0.,0.,-1.));
#36154=DIRECTION('center_axis',(0.,0.,1.));
#36155=DIRECTION('ref_axis',(1.,0.,0.));
#36156=DIRECTION('',(0.,0.,-1.));
#36157=DIRECTION('center_axis',(0.,0.,1.));
#36158=DIRECTION('ref_axis',(1.,0.,0.));
#36159=DIRECTION('',(0.,0.,-1.));
#36160=DIRECTION('center_axis',(0.,0.,1.));
#36161=DIRECTION('ref_axis',(1.,0.,0.));
#36162=DIRECTION('',(0.,0.,-1.));
#36163=DIRECTION('center_axis',(0.,0.,1.));
#36164=DIRECTION('ref_axis',(1.,0.,0.));
#36165=DIRECTION('',(0.,0.,-1.));
#36166=DIRECTION('center_axis',(0.,0.,1.));
#36167=DIRECTION('ref_axis',(1.,0.,0.));
#36168=DIRECTION('',(0.,0.,-1.));
#36169=DIRECTION('center_axis',(0.,0.,1.));
#36170=DIRECTION('ref_axis',(1.,0.,0.));
#36171=DIRECTION('',(0.,0.,-1.));
#36172=DIRECTION('center_axis',(0.,0.,1.));
#36173=DIRECTION('ref_axis',(1.,0.,0.));
#36174=DIRECTION('',(0.,0.,-1.));
#36175=DIRECTION('center_axis',(0.,0.,1.));
#36176=DIRECTION('ref_axis',(1.,0.,0.));
#36177=DIRECTION('',(0.,0.,-1.));
#36178=DIRECTION('center_axis',(0.,0.,1.));
#36179=DIRECTION('ref_axis',(1.,0.,0.));
#36180=DIRECTION('',(0.,0.,-1.));
#36181=DIRECTION('center_axis',(0.,0.,1.));
#36182=DIRECTION('ref_axis',(1.,0.,0.));
#36183=DIRECTION('',(0.,0.,-1.));
#36184=DIRECTION('center_axis',(0.,0.,1.));
#36185=DIRECTION('ref_axis',(1.,0.,0.));
#36186=DIRECTION('',(0.,0.,-1.));
#36187=DIRECTION('center_axis',(0.,0.,1.));
#36188=DIRECTION('ref_axis',(1.,0.,0.));
#36189=DIRECTION('',(0.,0.,-1.));
#36190=DIRECTION('center_axis',(0.,0.,1.));
#36191=DIRECTION('ref_axis',(1.,0.,0.));
#36192=DIRECTION('',(0.,0.,-1.));
#36193=DIRECTION('center_axis',(0.,0.,1.));
#36194=DIRECTION('ref_axis',(1.,0.,0.));
#36195=DIRECTION('',(0.,0.,-1.));
#36196=DIRECTION('center_axis',(0.,0.,1.));
#36197=DIRECTION('ref_axis',(1.,0.,0.));
#36198=DIRECTION('',(0.,0.,-1.));
#36199=DIRECTION('center_axis',(0.,0.,1.));
#36200=DIRECTION('ref_axis',(1.,0.,0.));
#36201=DIRECTION('',(0.,0.,-1.));
#36202=DIRECTION('center_axis',(0.,0.,1.));
#36203=DIRECTION('ref_axis',(1.,0.,0.));
#36204=DIRECTION('',(0.,0.,-1.));
#36205=DIRECTION('center_axis',(0.,0.,1.));
#36206=DIRECTION('ref_axis',(1.,0.,0.));
#36207=DIRECTION('',(0.,0.,-1.));
#36208=DIRECTION('center_axis',(0.,0.,1.));
#36209=DIRECTION('ref_axis',(1.,0.,0.));
#36210=DIRECTION('',(0.,0.,-1.));
#36211=DIRECTION('center_axis',(0.,0.,1.));
#36212=DIRECTION('ref_axis',(1.,0.,0.));
#36213=DIRECTION('',(0.,0.,-1.));
#36214=DIRECTION('center_axis',(0.,0.,1.));
#36215=DIRECTION('ref_axis',(1.,0.,0.));
#36216=DIRECTION('',(0.,0.,-1.));
#36217=DIRECTION('center_axis',(0.,0.,1.));
#36218=DIRECTION('ref_axis',(1.,0.,0.));
#36219=DIRECTION('',(0.,0.,-1.));
#36220=DIRECTION('center_axis',(0.,0.,1.));
#36221=DIRECTION('ref_axis',(1.,0.,0.));
#36222=DIRECTION('',(0.,0.,-1.));
#36223=DIRECTION('center_axis',(0.,0.,1.));
#36224=DIRECTION('ref_axis',(1.,0.,0.));
#36225=DIRECTION('',(0.,0.,-1.));
#36226=DIRECTION('center_axis',(0.,0.,1.));
#36227=DIRECTION('ref_axis',(1.,0.,0.));
#36228=DIRECTION('',(0.,0.,-1.));
#36229=DIRECTION('center_axis',(0.,0.,1.));
#36230=DIRECTION('ref_axis',(1.,0.,0.));
#36231=DIRECTION('',(0.,0.,-1.));
#36232=DIRECTION('center_axis',(0.,0.,1.));
#36233=DIRECTION('ref_axis',(1.,0.,0.));
#36234=DIRECTION('',(0.,0.,-1.));
#36235=DIRECTION('center_axis',(0.,0.,1.));
#36236=DIRECTION('ref_axis',(1.,0.,0.));
#36237=DIRECTION('',(0.,0.,-1.));
#36238=DIRECTION('center_axis',(0.,0.,1.));
#36239=DIRECTION('ref_axis',(1.,0.,0.));
#36240=DIRECTION('',(0.,0.,-1.));
#36241=DIRECTION('center_axis',(0.,0.,1.));
#36242=DIRECTION('ref_axis',(1.,0.,0.));
#36243=DIRECTION('',(0.,0.,-1.));
#36244=DIRECTION('center_axis',(0.,0.,1.));
#36245=DIRECTION('ref_axis',(1.,0.,0.));
#36246=DIRECTION('',(0.,0.,-1.));
#36247=DIRECTION('center_axis',(0.,0.,1.));
#36248=DIRECTION('ref_axis',(1.,0.,0.));
#36249=DIRECTION('',(0.,0.,-1.));
#36250=DIRECTION('center_axis',(0.,0.,1.));
#36251=DIRECTION('ref_axis',(1.,0.,0.));
#36252=DIRECTION('',(0.,0.,-1.));
#36253=DIRECTION('center_axis',(0.,0.,1.));
#36254=DIRECTION('ref_axis',(1.,0.,0.));
#36255=DIRECTION('',(0.,0.,-1.));
#36256=DIRECTION('center_axis',(0.,0.,1.));
#36257=DIRECTION('ref_axis',(1.,0.,0.));
#36258=DIRECTION('',(0.,0.,-1.));
#36259=DIRECTION('center_axis',(0.,0.,1.));
#36260=DIRECTION('ref_axis',(1.,0.,0.));
#36261=DIRECTION('',(0.,0.,-1.));
#36262=DIRECTION('center_axis',(0.,0.,1.));
#36263=DIRECTION('ref_axis',(1.,0.,0.));
#36264=DIRECTION('',(0.,0.,-1.));
#36265=DIRECTION('center_axis',(0.,0.,1.));
#36266=DIRECTION('ref_axis',(1.,0.,0.));
#36267=DIRECTION('',(0.,0.,-1.));
#36268=DIRECTION('center_axis',(0.,0.,1.));
#36269=DIRECTION('ref_axis',(1.,0.,0.));
#36270=DIRECTION('',(0.,0.,-1.));
#36271=DIRECTION('center_axis',(0.,0.,1.));
#36272=DIRECTION('ref_axis',(1.,0.,0.));
#36273=DIRECTION('',(0.,0.,-1.));
#36274=DIRECTION('center_axis',(0.,0.,1.));
#36275=DIRECTION('ref_axis',(1.,0.,0.));
#36276=DIRECTION('',(0.,0.,-1.));
#36277=DIRECTION('center_axis',(0.,0.,1.));
#36278=DIRECTION('ref_axis',(1.,0.,0.));
#36279=DIRECTION('',(0.,0.,-1.));
#36280=DIRECTION('center_axis',(0.,0.,1.));
#36281=DIRECTION('ref_axis',(1.,0.,0.));
#36282=DIRECTION('',(0.,0.,-1.));
#36283=DIRECTION('center_axis',(0.,0.,1.));
#36284=DIRECTION('ref_axis',(1.,0.,0.));
#36285=DIRECTION('',(0.,0.,-1.));
#36286=DIRECTION('center_axis',(0.,0.,1.));
#36287=DIRECTION('ref_axis',(1.,0.,0.));
#36288=DIRECTION('',(0.,0.,-1.));
#36289=DIRECTION('center_axis',(0.,0.,1.));
#36290=DIRECTION('ref_axis',(1.,0.,0.));
#36291=DIRECTION('',(0.,0.,-1.));
#36292=DIRECTION('center_axis',(0.,0.,1.));
#36293=DIRECTION('ref_axis',(1.,0.,0.));
#36294=DIRECTION('',(0.,0.,-1.));
#36295=DIRECTION('center_axis',(0.,0.,1.));
#36296=DIRECTION('ref_axis',(1.,0.,0.));
#36297=DIRECTION('',(0.,0.,-1.));
#36298=DIRECTION('center_axis',(0.,0.,1.));
#36299=DIRECTION('ref_axis',(1.,0.,0.));
#36300=DIRECTION('',(0.,0.,-1.));
#36301=DIRECTION('center_axis',(0.,0.,1.));
#36302=DIRECTION('ref_axis',(1.,0.,0.));
#36303=DIRECTION('',(0.,0.,-1.));
#36304=DIRECTION('center_axis',(0.,0.,1.));
#36305=DIRECTION('ref_axis',(1.,0.,0.));
#36306=DIRECTION('',(0.,0.,-1.));
#36307=DIRECTION('center_axis',(0.,0.,1.));
#36308=DIRECTION('ref_axis',(1.,0.,0.));
#36309=DIRECTION('center_axis',(0.,0.,1.));
#36310=DIRECTION('ref_axis',(0.288063002257283,-0.957611459168342,0.));
#36311=DIRECTION('',(0.,0.,1.));
#36312=DIRECTION('center_axis',(0.,0.,1.));
#36313=DIRECTION('ref_axis',(1.,-9.05137471385603E-13,0.));
#36314=DIRECTION('center_axis',(0.,0.,1.));
#36315=DIRECTION('ref_axis',(1.,-9.05137471385603E-13,0.));
#36316=DIRECTION('',(0.,0.,1.));
#36317=DIRECTION('center_axis',(0.,0.,1.));
#36318=DIRECTION('ref_axis',(1.,-9.05137471385603E-13,0.));
#36319=DIRECTION('',(0.,0.,1.));
#36320=DIRECTION('center_axis',(0.,0.,1.));
#36321=DIRECTION('ref_axis',(1.,-9.05137471385603E-13,0.));
#36322=DIRECTION('',(0.,0.,1.));
#36323=DIRECTION('center_axis',(0.,0.,1.));
#36324=DIRECTION('ref_axis',(1.,-9.05137471385603E-13,0.));
#36325=DIRECTION('',(0.,0.,1.));
#36326=DIRECTION('center_axis',(0.,0.,1.));
#36327=DIRECTION('ref_axis',(1.,-9.05137471385603E-13,0.));
#36328=DIRECTION('',(0.,0.,1.));
#36329=DIRECTION('center_axis',(0.,0.,1.));
#36330=DIRECTION('ref_axis',(1.,-9.05137471385603E-13,0.));
#36331=DIRECTION('',(0.,0.,1.));
#36332=DIRECTION('center_axis',(0.,0.,1.));
#36333=DIRECTION('ref_axis',(1.,-9.05137471385603E-13,0.));
#36334=DIRECTION('',(0.,0.,1.));
#36335=DIRECTION('center_axis',(0.,0.,1.));
#36336=DIRECTION('ref_axis',(1.,-9.05137471385603E-13,0.));
#36337=DIRECTION('',(0.,0.,1.));
#36338=DIRECTION('center_axis',(0.,0.,1.));
#36339=DIRECTION('ref_axis',(1.,-9.05137471385603E-13,0.));
#36340=DIRECTION('',(0.,0.,1.));
#36341=DIRECTION('center_axis',(0.,0.,1.));
#36342=DIRECTION('ref_axis',(1.,-9.05137471385603E-13,0.));
#36343=DIRECTION('',(0.,0.,1.));
#36344=DIRECTION('center_axis',(0.,0.,1.));
#36345=DIRECTION('ref_axis',(1.,-9.05137471385603E-13,0.));
#36346=DIRECTION('',(0.,0.,1.));
#36347=DIRECTION('center_axis',(0.,0.,1.));
#36348=DIRECTION('ref_axis',(1.,-9.05137471385603E-13,0.));
#36349=DIRECTION('',(0.,0.,1.));
#36350=DIRECTION('center_axis',(0.,0.,1.));
#36351=DIRECTION('ref_axis',(1.,-9.05137471385603E-13,0.));
#36352=DIRECTION('',(0.,0.,1.));
#36353=DIRECTION('center_axis',(0.,0.,1.));
#36354=DIRECTION('ref_axis',(1.,-9.05137471385603E-13,0.));
#36355=DIRECTION('',(0.,0.,1.));
#36356=DIRECTION('center_axis',(0.,0.,1.));
#36357=DIRECTION('ref_axis',(1.,-9.05137471385603E-13,0.));
#36358=DIRECTION('',(0.,0.,1.));
#36359=DIRECTION('center_axis',(0.,0.,1.));
#36360=DIRECTION('ref_axis',(1.,-9.05137471385603E-13,0.));
#36361=DIRECTION('',(0.,0.,1.));
#36362=DIRECTION('center_axis',(0.,0.,1.));
#36363=DIRECTION('ref_axis',(1.,-9.05137471385603E-13,0.));
#36364=DIRECTION('',(0.,0.,1.));
#36365=DIRECTION('center_axis',(0.,0.,1.));
#36366=DIRECTION('ref_axis',(1.,-9.05137471385603E-13,0.));
#36367=DIRECTION('',(0.,0.,1.));
#36368=DIRECTION('center_axis',(0.,0.,1.));
#36369=DIRECTION('ref_axis',(1.,-9.05137471385603E-13,0.));
#36370=DIRECTION('',(0.,0.,1.));
#36371=DIRECTION('center_axis',(0.,0.,1.));
#36372=DIRECTION('ref_axis',(1.,-9.05137471385603E-13,0.));
#36373=DIRECTION('',(0.,0.,1.));
#36374=DIRECTION('center_axis',(0.,0.,1.));
#36375=DIRECTION('ref_axis',(1.,-9.05137471385603E-13,0.));
#36376=DIRECTION('',(0.,0.,1.));
#36377=DIRECTION('center_axis',(0.,0.,1.));
#36378=DIRECTION('ref_axis',(1.,-9.05137471385603E-13,0.));
#36379=DIRECTION('',(0.,0.,1.));
#36380=DIRECTION('center_axis',(0.,0.,1.));
#36381=DIRECTION('ref_axis',(1.,-9.05137471385603E-13,0.));
#36382=DIRECTION('',(0.,0.,1.));
#36383=DIRECTION('center_axis',(0.,0.,1.));
#36384=DIRECTION('ref_axis',(1.,-9.05137471385603E-13,0.));
#36385=DIRECTION('',(0.,0.,1.));
#36386=DIRECTION('center_axis',(0.,0.,1.));
#36387=DIRECTION('ref_axis',(1.,-9.05137471385603E-13,0.));
#36388=DIRECTION('',(0.,0.,1.));
#36389=DIRECTION('center_axis',(0.,0.,1.));
#36390=DIRECTION('ref_axis',(1.,-9.05137471385603E-13,0.));
#36391=DIRECTION('',(0.,0.,1.));
#36392=DIRECTION('center_axis',(0.,0.,1.));
#36393=DIRECTION('ref_axis',(1.,-9.05137471385603E-13,0.));
#36394=DIRECTION('',(0.,0.,1.));
#36395=DIRECTION('center_axis',(0.,0.,1.));
#36396=DIRECTION('ref_axis',(1.,-9.05137471385603E-13,0.));
#36397=DIRECTION('',(0.,0.,1.));
#36398=DIRECTION('center_axis',(0.,0.,1.));
#36399=DIRECTION('ref_axis',(1.,-9.05137471385603E-13,0.));
#36400=DIRECTION('',(0.,0.,1.));
#36401=DIRECTION('center_axis',(0.,0.,1.));
#36402=DIRECTION('ref_axis',(1.,-9.05137471385603E-13,0.));
#36403=DIRECTION('',(0.,0.,1.));
#36404=DIRECTION('center_axis',(0.,0.,1.));
#36405=DIRECTION('ref_axis',(1.,-9.05137471385603E-13,0.));
#36406=DIRECTION('',(0.,0.,1.));
#36407=DIRECTION('center_axis',(0.,0.,1.));
#36408=DIRECTION('ref_axis',(1.,-9.05137471385603E-13,0.));
#36409=DIRECTION('',(0.,0.,1.));
#36410=DIRECTION('center_axis',(0.,0.,1.));
#36411=DIRECTION('ref_axis',(1.,-9.05137471385603E-13,0.));
#36412=DIRECTION('',(0.,0.,1.));
#36413=DIRECTION('center_axis',(0.,0.,1.));
#36414=DIRECTION('ref_axis',(1.,-9.05137471385603E-13,0.));
#36415=DIRECTION('',(0.,0.,1.));
#36416=DIRECTION('center_axis',(0.,0.,1.));
#36417=DIRECTION('ref_axis',(1.,-9.05137471385603E-13,0.));
#36418=DIRECTION('',(0.,0.,1.));
#36419=DIRECTION('center_axis',(0.,0.,1.));
#36420=DIRECTION('ref_axis',(1.,-9.05137471385603E-13,0.));
#36421=DIRECTION('',(0.,0.,1.));
#36422=DIRECTION('center_axis',(0.,0.,1.));
#36423=DIRECTION('ref_axis',(1.,-9.05137471385603E-13,0.));
#36424=DIRECTION('',(0.,0.,1.));
#36425=DIRECTION('center_axis',(0.,0.,1.));
#36426=DIRECTION('ref_axis',(1.,-9.05137471385603E-13,0.));
#36427=DIRECTION('',(0.,0.,1.));
#36428=DIRECTION('center_axis',(0.,0.,1.));
#36429=DIRECTION('ref_axis',(1.,-9.05137471385603E-13,0.));
#36430=DIRECTION('',(0.,0.,1.));
#36431=DIRECTION('center_axis',(0.,0.,1.));
#36432=DIRECTION('ref_axis',(1.,-9.05137471385603E-13,0.));
#36433=DIRECTION('',(0.,0.,1.));
#36434=DIRECTION('center_axis',(0.,0.,1.));
#36435=DIRECTION('ref_axis',(1.,-9.05137471385603E-13,0.));
#36436=DIRECTION('',(0.,0.,1.));
#36437=DIRECTION('center_axis',(0.,0.,1.));
#36438=DIRECTION('ref_axis',(1.,-9.05137471385603E-13,0.));
#36439=DIRECTION('',(0.,0.,1.));
#36440=DIRECTION('center_axis',(0.,0.,1.));
#36441=DIRECTION('ref_axis',(1.,-9.05137471385603E-13,0.));
#36442=DIRECTION('',(0.,0.,1.));
#36443=DIRECTION('center_axis',(0.,0.,1.));
#36444=DIRECTION('ref_axis',(1.,-9.05137471385603E-13,0.));
#36445=DIRECTION('',(0.,0.,1.));
#36446=DIRECTION('center_axis',(0.,0.,1.));
#36447=DIRECTION('ref_axis',(1.,-9.05137471385603E-13,0.));
#36448=DIRECTION('',(0.,0.,1.));
#36449=DIRECTION('center_axis',(0.,0.,1.));
#36450=DIRECTION('ref_axis',(1.,-9.05137471385603E-13,0.));
#36451=DIRECTION('',(0.,0.,1.));
#36452=DIRECTION('center_axis',(0.,0.,1.));
#36453=DIRECTION('ref_axis',(1.,-9.05137471385603E-13,0.));
#36454=DIRECTION('',(0.,0.,1.));
#36455=DIRECTION('center_axis',(0.,0.,1.));
#36456=DIRECTION('ref_axis',(1.,-9.05137471385603E-13,0.));
#36457=DIRECTION('',(0.,0.,1.));
#36458=DIRECTION('center_axis',(0.,0.,1.));
#36459=DIRECTION('ref_axis',(1.,-9.05137471385603E-13,0.));
#36460=DIRECTION('',(0.,0.,1.));
#36461=DIRECTION('center_axis',(0.,0.,1.));
#36462=DIRECTION('ref_axis',(1.,-9.05137471385603E-13,0.));
#36463=DIRECTION('',(0.,0.,1.));
#36464=DIRECTION('center_axis',(0.,0.,1.));
#36465=DIRECTION('ref_axis',(1.,-9.05137471385603E-13,0.));
#36466=DIRECTION('',(0.,0.,1.));
#36467=DIRECTION('center_axis',(0.,0.,1.));
#36468=DIRECTION('ref_axis',(1.,-9.05137471385603E-13,0.));
#36469=DIRECTION('',(0.,0.,1.));
#36470=DIRECTION('center_axis',(0.,0.,1.));
#36471=DIRECTION('ref_axis',(1.,-9.05137471385603E-13,0.));
#36472=DIRECTION('',(0.,0.,1.));
#36473=DIRECTION('center_axis',(0.,0.,1.));
#36474=DIRECTION('ref_axis',(1.,-9.05137471385603E-13,0.));
#36475=DIRECTION('',(0.,0.,1.));
#36476=DIRECTION('center_axis',(0.,0.,1.));
#36477=DIRECTION('ref_axis',(1.,-9.05137471385603E-13,0.));
#36478=DIRECTION('',(0.,0.,1.));
#36479=DIRECTION('center_axis',(0.,0.,1.));
#36480=DIRECTION('ref_axis',(1.,-9.05137471385603E-13,0.));
#36481=DIRECTION('',(0.,0.,1.));
#36482=DIRECTION('center_axis',(0.,0.,1.));
#36483=DIRECTION('ref_axis',(1.,-9.05137471385603E-13,0.));
#36484=DIRECTION('',(0.,0.,1.));
#36485=DIRECTION('center_axis',(0.,0.,1.));
#36486=DIRECTION('ref_axis',(1.,-9.05137471385603E-13,0.));
#36487=DIRECTION('',(0.,0.,1.));
#36488=DIRECTION('',(0.,0.,-1.));
#36489=DIRECTION('',(0.,0.,-1.));
#36490=DIRECTION('',(0.,0.,-1.));
#36491=DIRECTION('',(0.,0.,-1.));
#36492=DIRECTION('',(0.,0.,-1.));
#36493=DIRECTION('',(0.,0.,-1.));
#36494=DIRECTION('',(0.,0.,-1.));
#36495=DIRECTION('',(0.,0.,-1.));
#36496=DIRECTION('',(0.,0.,-1.));
#36497=DIRECTION('',(0.,0.,-1.));
#36498=DIRECTION('',(0.,0.,-1.));
#36499=DIRECTION('',(0.,0.,-1.));
#36500=DIRECTION('',(0.,0.,-1.));
#36501=DIRECTION('',(0.,0.,-1.));
#36502=DIRECTION('',(0.,0.,-1.));
#36503=DIRECTION('',(0.,0.,-1.));
#36504=DIRECTION('',(0.,0.,-1.));
#36505=DIRECTION('',(0.,0.,-1.));
#36506=DIRECTION('',(0.,0.,-1.));
#36507=DIRECTION('',(0.,0.,-1.));
#36508=DIRECTION('',(0.,0.,-1.));
#36509=DIRECTION('',(0.,0.,-1.));
#36510=DIRECTION('',(0.,0.,-1.));
#36511=DIRECTION('',(0.,0.,-1.));
#36512=DIRECTION('',(0.,0.,-1.));
#36513=DIRECTION('',(0.,0.,-1.));
#36514=DIRECTION('',(0.,0.,-1.));
#36515=DIRECTION('',(0.,0.,-1.));
#36516=DIRECTION('',(0.,0.,-1.));
#36517=DIRECTION('',(0.,0.,-1.));
#36518=DIRECTION('',(0.,0.,-1.));
#36519=DIRECTION('',(0.,0.,-1.));
#36520=DIRECTION('',(0.,0.,-1.));
#36521=DIRECTION('center_axis',(0.,0.,1.));
#36522=DIRECTION('ref_axis',(1.,0.,0.));
#36523=DIRECTION('center_axis',(0.,1.,0.));
#36524=DIRECTION('ref_axis',(1.,0.,0.));
#36525=DIRECTION('',(1.,0.,0.));
#36526=DIRECTION('',(0.,0.,-1.));
#36527=DIRECTION('',(1.,0.,0.));
#36528=DIRECTION('',(0.,0.,-1.));
#36529=DIRECTION('center_axis',(-1.,0.,0.));
#36530=DIRECTION('ref_axis',(0.,1.,0.));
#36531=DIRECTION('',(0.,1.,0.));
#36532=DIRECTION('',(0.,0.,-1.));
#36533=DIRECTION('',(0.,1.,0.));
#36534=DIRECTION('center_axis',(0.,-1.,0.));
#36535=DIRECTION('ref_axis',(-1.,0.,0.));
#36536=DIRECTION('',(-1.,0.,0.));
#36537=DIRECTION('',(0.,0.,-1.));
#36538=DIRECTION('',(-1.,0.,0.));
#36539=DIRECTION('center_axis',(1.,0.,0.));
#36540=DIRECTION('ref_axis',(0.,-1.,0.));
#36541=DIRECTION('',(0.,-1.,0.));
#36542=DIRECTION('',(0.,-1.,0.));
#36543=DIRECTION('center_axis',(0.,0.,-1.));
#36544=DIRECTION('ref_axis',(-1.,0.,0.));
#36545=DIRECTION('',(0.,0.,-1.));
#36546=DIRECTION('',(0.,0.,-1.));
#36547=DIRECTION('',(0.,0.,-1.));
#36548=DIRECTION('',(0.,0.,-1.));
#36549=DIRECTION('',(0.,0.,-1.));
#36550=DIRECTION('',(0.,0.,-1.));
#36551=DIRECTION('',(0.,0.,-1.));
#36552=DIRECTION('',(0.,0.,-1.));
#36553=DIRECTION('',(0.,0.,-1.));
#36554=DIRECTION('',(0.,0.,-1.));
#36555=DIRECTION('',(0.,0.,-1.));
#36556=DIRECTION('',(0.,0.,-1.));
#36557=DIRECTION('',(0.,0.,-1.));
#36558=DIRECTION('',(0.,0.,-1.));
#36559=DIRECTION('',(0.,0.,-1.));
#36560=DIRECTION('',(0.,0.,-1.));
#36561=DIRECTION('',(0.,0.,-1.));
#36562=DIRECTION('',(0.,0.,-1.));
#36563=DIRECTION('',(0.,0.,-1.));
#36564=DIRECTION('',(0.,0.,-1.));
#36565=DIRECTION('',(0.,0.,-1.));
#36566=DIRECTION('',(0.,0.,-1.));
#36567=DIRECTION('',(0.,0.,-1.));
#36568=DIRECTION('',(0.,0.,-1.));
#36569=DIRECTION('',(0.,0.,-1.));
#36570=DIRECTION('',(0.,0.,-1.));
#36571=DIRECTION('',(0.,0.,-1.));
#36572=DIRECTION('',(0.,0.,-1.));
#36573=DIRECTION('',(0.,0.,-1.));
#36574=DIRECTION('',(0.,0.,-1.));
#36575=DIRECTION('',(0.,0.,-1.));
#36576=DIRECTION('',(0.,0.,-1.));
#36577=DIRECTION('',(0.,0.,-1.));
#36578=DIRECTION('center_axis',(0.,0.,1.));
#36579=DIRECTION('ref_axis',(1.,0.,0.));
#36580=DIRECTION('center_axis',(0.,0.,1.));
#36581=DIRECTION('ref_axis',(1.,0.,0.));
#36582=DIRECTION('center_axis',(0.,0.,1.));
#36583=DIRECTION('ref_axis',(1.,0.,0.));
#36584=DIRECTION('center_axis',(0.,0.,1.));
#36585=DIRECTION('ref_axis',(1.,0.,0.));
#36586=DIRECTION('center_axis',(0.,0.,1.));
#36587=DIRECTION('ref_axis',(1.,0.,0.));
#36588=DIRECTION('center_axis',(0.,0.,1.));
#36589=DIRECTION('ref_axis',(1.,0.,0.));
#36590=DIRECTION('center_axis',(0.,0.,1.));
#36591=DIRECTION('ref_axis',(1.,0.,0.));
#36592=DIRECTION('center_axis',(0.,0.,1.));
#36593=DIRECTION('ref_axis',(1.,0.,0.));
#36594=DIRECTION('center_axis',(0.,0.,1.));
#36595=DIRECTION('ref_axis',(1.,0.,0.));
#36596=DIRECTION('center_axis',(0.,0.,1.));
#36597=DIRECTION('ref_axis',(1.,0.,0.));
#36598=DIRECTION('center_axis',(0.,0.,1.));
#36599=DIRECTION('ref_axis',(1.,0.,0.));
#36600=DIRECTION('center_axis',(0.,0.,-1.));
#36601=DIRECTION('ref_axis',(1.,-9.05137471385603E-13,0.));
#36602=DIRECTION('center_axis',(0.,0.,1.));
#36603=DIRECTION('ref_axis',(1.,-9.05137471385603E-13,0.));
#36604=DIRECTION('center_axis',(0.,0.,-1.));
#36605=DIRECTION('ref_axis',(-1.,0.,0.));
#36606=DIRECTION('center_axis',(0.,0.,-1.));
#36607=DIRECTION('ref_axis',(1.,0.,0.));
#36608=DIRECTION('center_axis',(-1.22464679914735E-16,-1.,0.));
#36609=DIRECTION('ref_axis',(1.,-1.22464679914735E-16,0.));
#36610=DIRECTION('center_axis',(0.,0.,1.));
#36611=DIRECTION('ref_axis',(1.,0.,0.));
#36612=DIRECTION('center_axis',(0.,0.,1.));
#36613=DIRECTION('ref_axis',(1.,0.,0.));
#36614=DIRECTION('',(3.20493781063927E-16,1.,0.));
#36615=DIRECTION('',(0.866025403784439,0.5,0.));
#36616=DIRECTION('',(0.866025403784439,-0.5,0.));
#36617=DIRECTION('',(1.60246890531964E-16,-1.,0.));
#36618=DIRECTION('',(-0.866025403784439,-0.5,0.));
#36619=DIRECTION('',(-0.866025403784439,0.5,0.));
#36620=DIRECTION('center_axis',(0.,0.,1.));
#36621=DIRECTION('ref_axis',(-0.978821812799614,-0.204714090349635,0.));
#36622=DIRECTION('center_axis',(0.,0.,-1.));
#36623=DIRECTION('ref_axis',(1.,0.,0.));
#36624=DIRECTION('',(0.866025403784438,1.06057523872491E-16,0.5));
#36625=DIRECTION('center_axis',(0.,0.,1.));
#36626=DIRECTION('ref_axis',(1.,0.,0.));
#36627=DIRECTION('center_axis',(-0.5,0.866025403784439,0.));
#36628=DIRECTION('ref_axis',(-0.866025403784439,-0.5,0.));
#36629=DIRECTION('',(0.,0.,1.));
#36630=DIRECTION('',(0.,0.,1.));
#36631=DIRECTION('center_axis',(0.5,0.866025403784439,0.));
#36632=DIRECTION('ref_axis',(-0.866025403784439,0.5,0.));
#36633=DIRECTION('',(0.,0.,1.));
#36634=DIRECTION('center_axis',(1.,-3.20493781063927E-16,0.));
#36635=DIRECTION('ref_axis',(3.20493781063927E-16,1.,0.));
#36636=DIRECTION('',(0.,0.,1.));
#36637=DIRECTION('center_axis',(0.5,-0.866025403784439,0.));
#36638=DIRECTION('ref_axis',(0.866025403784439,0.5,0.));
#36639=DIRECTION('',(0.,0.,1.));
#36640=DIRECTION('center_axis',(-0.5,-0.866025403784439,0.));
#36641=DIRECTION('ref_axis',(0.866025403784439,-0.5,0.));
#36642=DIRECTION('',(0.,0.,1.));
#36643=DIRECTION('center_axis',(-1.,-1.60246890531964E-16,0.));
#36644=DIRECTION('ref_axis',(1.60246890531964E-16,-1.,0.));
#36645=DIRECTION('center_axis',(0.,0.,1.));
#36646=DIRECTION('ref_axis',(1.,0.,0.));
#36647=DIRECTION('center_axis',(0.,0.,-1.));
#36648=DIRECTION('ref_axis',(-1.,0.,0.));
#36649=DIRECTION('center_axis',(0.,0.,1.));
#36650=DIRECTION('ref_axis',(1.,0.,0.));
#36651=DIRECTION('center_axis',(0.,0.,1.));
#36652=DIRECTION('ref_axis',(1.,0.,0.));
#36653=DIRECTION('',(0.707106781186549,8.65956056235495E-17,-0.707106781186546));
#36654=DIRECTION('axis',(0.,0.,1.));
#36655=DIRECTION('refdir',(1.,0.,0.));
#36656=DIRECTION('center_axis',(0.,0.,-1.));
#36657=DIRECTION('ref_axis',(1.,0.,0.));
#36658=DIRECTION('center_axis',(0.,0.,1.));
#36659=DIRECTION('ref_axis',(1.,0.,0.));
#36660=DIRECTION('',(-0.707106781186547,-8.65956056235493E-17,-0.707106781186548));
#36661=DIRECTION('center_axis',(0.,0.,-1.));
#36662=DIRECTION('ref_axis',(1.,0.,0.));
#36663=DIRECTION('center_axis',(0.,0.,1.));
#36664=DIRECTION('ref_axis',(1.,0.,0.));
#36665=DIRECTION('center_axis',(0.,0.,-1.));
#36666=DIRECTION('ref_axis',(1.,0.,0.));
#36667=DIRECTION('',(0.,0.,-1.));
#36668=DIRECTION('center_axis',(0.,0.,1.));
#36669=DIRECTION('ref_axis',(1.,0.,0.));
#36670=DIRECTION('center_axis',(0.,0.,-1.));
#36671=DIRECTION('ref_axis',(1.,0.,0.));
#36672=DIRECTION('center_axis',(0.,0.,1.));
#36673=DIRECTION('ref_axis',(1.,0.,0.));
#36674=DIRECTION('center_axis',(0.,0.,1.));
#36675=DIRECTION('ref_axis',(1.,0.,0.));
#36676=DIRECTION('',(0.707106781186547,8.65956056235493E-17,-0.707106781186548));
#36677=DIRECTION('center_axis',(0.,0.,1.));
#36678=DIRECTION('ref_axis',(1.,0.,0.));
#36679=DIRECTION('center_axis',(0.,0.,1.));
#36680=DIRECTION('ref_axis',(1.,0.,0.));
#36681=DIRECTION('center_axis',(0.,0.,1.));
#36682=DIRECTION('ref_axis',(1.,0.,0.));
#36683=DIRECTION('',(-0.866025403784439,-1.06057523872491E-16,0.5));
#36684=DIRECTION('center_axis',(0.5,-0.866025403784439,0.));
#36685=DIRECTION('ref_axis',(0.866025403784439,0.5,0.));
#36686=DIRECTION('',(0.,0.,1.));
#36687=DIRECTION('',(0.,0.,1.));
#36688=DIRECTION('center_axis',(1.,-3.20493781063927E-16,0.));
#36689=DIRECTION('ref_axis',(3.20493781063927E-16,1.,0.));
#36690=DIRECTION('',(0.,0.,1.));
#36691=DIRECTION('center_axis',(0.5,0.866025403784439,0.));
#36692=DIRECTION('ref_axis',(-0.866025403784439,0.5,0.));
#36693=DIRECTION('',(0.,0.,1.));
#36694=DIRECTION('center_axis',(0.,0.,-1.));
#36695=DIRECTION('ref_axis',(1.,0.,0.));
#36696=DIRECTION('',(0.866025403784439,1.06057523872491E-16,0.5));
#36697=DIRECTION('center_axis',(-0.5,0.866025403784439,0.));
#36698=DIRECTION('ref_axis',(-0.866025403784439,-0.5,0.));
#36699=DIRECTION('',(0.,0.,1.));
#36700=DIRECTION('center_axis',(-0.5,-0.866025403784439,0.));
#36701=DIRECTION('ref_axis',(0.866025403784439,-0.5,0.));
#36702=DIRECTION('',(0.,0.,1.));
#36703=DIRECTION('center_axis',(-1.,-1.60246890531964E-16,0.));
#36704=DIRECTION('ref_axis',(1.60246890531964E-16,-1.,0.));
#36705=DIRECTION('axis',(0.,0.,1.));
#36706=DIRECTION('refdir',(1.,0.,0.));
#36707=DIRECTION('center_axis',(0.,0.,1.));
#36708=DIRECTION('ref_axis',(1.,0.,0.));
#36709=DIRECTION('center_axis',(0.,0.,1.));
#36710=DIRECTION('ref_axis',(1.,0.,0.));
#36711=DIRECTION('',(0.,0.,-1.));
#36712=DIRECTION('center_axis',(0.,0.,1.));
#36713=DIRECTION('ref_axis',(1.,0.,0.));
#36714=DIRECTION('center_axis',(0.,0.,-1.));
#36715=DIRECTION('ref_axis',(-1.,0.,0.));
#36716=DIRECTION('center_axis',(0.,0.,1.));
#36717=DIRECTION('ref_axis',(1.,0.,0.));
#36718=DIRECTION('center_axis',(0.,0.,1.));
#36719=DIRECTION('ref_axis',(1.,0.,0.));
#36720=DIRECTION('center_axis',(0.,0.,1.));
#36721=DIRECTION('ref_axis',(1.,0.,0.));
#36722=DIRECTION('',(0.,0.,-1.));
#36723=DIRECTION('center_axis',(0.,0.,-1.));
#36724=DIRECTION('ref_axis',(1.,0.,0.));
#36725=DIRECTION('center_axis',(0.,0.,1.));
#36726=DIRECTION('ref_axis',(1.,0.,0.));
#36727=DIRECTION('',(-0.707106781186548,-8.65956056235494E-17,-0.707106781186547));
#36728=DIRECTION('center_axis',(0.,0.,1.));
#36729=DIRECTION('ref_axis',(1.,0.,0.));
#36730=DIRECTION('center_axis',(0.,0.,1.));
#36731=DIRECTION('ref_axis',(1.,0.,0.));
#36732=DIRECTION('center_axis',(0.,0.,1.));
#36733=DIRECTION('ref_axis',(1.,0.,0.));
#36734=DIRECTION('',(0.707106781186548,8.65956056235494E-17,-0.707106781186547));
#36735=DIRECTION('axis',(0.,0.,1.));
#36736=DIRECTION('refdir',(1.,0.,0.));
#36737=DIRECTION('center_axis',(0.951056516295133,0.,0.309016994375011));
#36738=DIRECTION('ref_axis',(0.309016994374947,0.,-0.951056516295154));
#36739=DIRECTION('center_axis',(0.951056516295154,0.,0.309016994374948));
#36740=DIRECTION('ref_axis',(0.309016994374948,0.,-0.951056516295153));
#36741=DIRECTION('',(0.0784590957277245,1.13142611228773E-16,0.996917333733138));
#36742=DIRECTION('center_axis',(-0.951056516295154,-2.65900928743012E-15,
-0.309016994374947));
#36743=DIRECTION('ref_axis',(0.309016994374947,0.,-0.951056516295154));
#36744=DIRECTION('center_axis',(-0.951056516295154,-2.65900928743012E-15,
-0.309016994374947));
#36745=DIRECTION('ref_axis',(0.309016994374947,0.,-0.951056516295154));
#36746=DIRECTION('center_axis',(0.951056516295154,0.,0.309016994374948));
#36747=DIRECTION('ref_axis',(-0.309016994374944,0.,0.951056516295155));
#36748=DIRECTION('',(0.891006524188362,-8.65956056235505E-17,-0.453990499739558));
#36749=DIRECTION('center_axis',(0.951056516295154,0.,0.309016994374946));
#36750=DIRECTION('ref_axis',(0.309016994374946,0.,-0.951056516295154));
#36751=DIRECTION('center_axis',(0.951056516295154,0.,0.309016994374946));
#36752=DIRECTION('ref_axis',(0.309016994374946,0.,-0.951056516295154));
#36753=DIRECTION('center_axis',(-0.951056516295154,0.,-0.309016994374948));
#36754=DIRECTION('ref_axis',(-0.309016994374948,0.,0.951056516295154));
#36755=DIRECTION('center_axis',(0.951056516295153,0.,0.309016994374949));
#36756=DIRECTION('ref_axis',(0.309016994374945,0.,-0.951056516295154));
#36757=DIRECTION('',(0.760405965600097,4.68652040532512E-17,0.649448048330106));
#36758=DIRECTION('center_axis',(-0.951056516295154,0.,-0.309016994374948));
#36759=DIRECTION('ref_axis',(0.309016994374944,0.,-0.951056516295155));
#36760=DIRECTION('center_axis',(-0.951056516295154,0.,-0.309016994374948));
#36761=DIRECTION('ref_axis',(0.309016994374944,0.,-0.951056516295155));
#36762=DIRECTION('center_axis',(-0.951056516295154,0.,-0.309016994374948));
#36763=DIRECTION('ref_axis',(-0.309016994374944,0.,0.951056516295155));
#36764=DIRECTION('',(0.951056516295154,0.,0.309016994374948));
#36765=DIRECTION('center_axis',(-0.951056516295154,0.,-0.309016994374948));
#36766=DIRECTION('ref_axis',(-0.309016994374944,0.,0.951056516295155));
#36767=DIRECTION('center_axis',(0.,1.,0.));
#36768=DIRECTION('ref_axis',(1.,0.,0.));
#36769=DIRECTION('center_axis',(0.,1.,0.));
#36770=DIRECTION('ref_axis',(1.,0.,0.));
#36771=DIRECTION('',(0.707106781186547,-0.707106781186547,-8.65956056235493E-17));
#36772=DIRECTION('center_axis',(0.,-1.,0.));
#36773=DIRECTION('ref_axis',(1.,0.,0.));
#36774=DIRECTION('center_axis',(0.,1.,0.));
#36775=DIRECTION('ref_axis',(1.,0.,0.));
#36776=DIRECTION('center_axis',(0.,1.,0.));
#36777=DIRECTION('ref_axis',(1.,0.,0.));
#36778=DIRECTION('',(0.,1.,0.));
#36779=DIRECTION('center_axis',(0.,1.,0.));
#36780=DIRECTION('ref_axis',(1.,0.,0.));
#36781=DIRECTION('',(-0.309016994374948,0.,0.951056516295154));
#36782=DIRECTION('',(-0.951056516295154,0.,-0.309016994374947));
#36783=DIRECTION('center_axis',(0.,-1.,0.));
#36784=DIRECTION('ref_axis',(-0.309016994374959,0.,0.95105651629515));
#36785=DIRECTION('',(0.951056516295154,0.,0.309016994374947));
#36786=DIRECTION('center_axis',(0.,-1.,0.));
#36787=DIRECTION('ref_axis',(1.,0.,0.));
#36788=DIRECTION('center_axis',(0.,-1.,0.));
#36789=DIRECTION('ref_axis',(1.,0.,0.));
#36790=DIRECTION('',(0.707106781186547,0.707106781186547,8.65956056235493E-17));
#36791=DIRECTION('center_axis',(0.,1.,0.));
#36792=DIRECTION('ref_axis',(1.,0.,0.));
#36793=DIRECTION('',(0.309016994374948,0.,-0.951056516295154));
#36794=DIRECTION('',(-0.951056516295154,0.,-0.309016994374947));
#36795=DIRECTION('center_axis',(0.,1.,0.));
#36796=DIRECTION('ref_axis',(-0.309016994374959,0.,0.95105651629515));
#36797=DIRECTION('',(0.951056516295154,0.,0.309016994374947));
#36798=DIRECTION('center_axis',(-0.95105651629516,0.,-0.309016994374926));
#36799=DIRECTION('ref_axis',(0.309016994374946,0.,-0.951056516295154));
#36800=DIRECTION('center_axis',(0.951056516295154,0.,0.309016994374948));
#36801=DIRECTION('ref_axis',(0.309016994374944,0.,-0.951056516295155));
#36802=DIRECTION('center_axis',(0.951056516295154,0.,0.309016994374948));
#36803=DIRECTION('ref_axis',(0.309016994374944,0.,-0.951056516295155));
#36804=DIRECTION('',(0.891006524188383,-8.65956056235445E-17,-0.453990499739517));
#36805=DIRECTION('center_axis',(-0.951056516295154,0.,-0.309016994374948));
#36806=DIRECTION('ref_axis',(0.309016994374948,0.,-0.951056516295153));
#36807=DIRECTION('center_axis',(-0.951056516295154,0.,-0.309016994374948));
#36808=DIRECTION('ref_axis',(-0.309016994374944,0.,0.951056516295155));
#36809=DIRECTION('center_axis',(0.951056516295154,0.,0.309016994374948));
#36810=DIRECTION('ref_axis',(-0.309016994374944,0.,0.951056516295155));
#36811=DIRECTION('',(0.951056516295154,0.,0.309016994374948));
#36812=DIRECTION('center_axis',(0.951056516295154,0.,0.309016994374948));
#36813=DIRECTION('ref_axis',(0.309016994374948,0.,-0.951056516295154));
#36814=DIRECTION('center_axis',(-0.951056516295154,0.,-0.309016994374948));
#36815=DIRECTION('ref_axis',(0.309016994374948,0.,-0.951056516295154));
#36816=DIRECTION('center_axis',(-0.951056516295154,0.,-0.309016994374948));
#36817=DIRECTION('ref_axis',(-0.309016994374948,0.,0.951056516295154));
#36818=DIRECTION('center_axis',(-0.951056516295154,0.,-0.309016994374948));
#36819=DIRECTION('ref_axis',(0.309016994374948,0.,-0.951056516295154));
#36820=DIRECTION('center_axis',(-0.951056516295154,0.,-0.309016994374948));
#36821=DIRECTION('ref_axis',(-0.309016994374948,0.,0.951056516295153));
#36822=DIRECTION('center_axis',(-0.951056516295154,0.,-0.309016994374948));
#36823=DIRECTION('ref_axis',(0.309016994374948,0.,-0.951056516295154));
#36824=DIRECTION('',(-0.951056516295153,0.,-0.309016994374948));
#36825=DIRECTION('center_axis',(0.951056516295154,0.,0.309016994374948));
#36826=DIRECTION('ref_axis',(0.309016994374948,0.,-0.951056516295154));
#36827=DIRECTION('center_axis',(0.951056516295154,0.,0.309016994374948));
#36828=DIRECTION('ref_axis',(-0.309016994374944,0.,0.951056516295155));
#36829=DIRECTION('center_axis',(-0.951056516295154,0.,-0.309016994374948));
#36830=DIRECTION('ref_axis',(-0.309016994374944,0.,0.951056516295155));
#36831=DIRECTION('',(0.951056516295154,0.,0.309016994374948));
#36832=DIRECTION('center_axis',(-0.951056516295154,0.,-0.309016994374948));
#36833=DIRECTION('ref_axis',(-0.309016994374944,0.,0.951056516295155));
#36834=DIRECTION('center_axis',(-0.951056516295154,0.,-0.309016994374948));
#36835=DIRECTION('ref_axis',(-0.309016994374948,0.,0.951056516295154));
#36836=DIRECTION('center_axis',(-0.951056516295154,0.,-0.309016994374948));
#36837=DIRECTION('ref_axis',(0.309016994374948,0.,-0.951056516295153));
#36838=DIRECTION('center_axis',(-0.951056516295154,0.,-0.309016994374948));
#36839=DIRECTION('ref_axis',(-0.309016994374948,0.,0.951056516295154));
#36840=DIRECTION('center_axis',(-0.951056516295154,0.,-0.309016994374948));
#36841=DIRECTION('ref_axis',(0.309016994374948,0.,-0.951056516295153));
#36842=DIRECTION('',(-0.951056516295154,0.,-0.309016994374948));
#36843=DIRECTION('center_axis',(0.951056516295154,0.,0.309016994374948));
#36844=DIRECTION('ref_axis',(0.309016994374948,0.,-0.951056516295154));
#36845=DIRECTION('center_axis',(0.951056516295154,0.,0.309016994374948));
#36846=DIRECTION('ref_axis',(-0.309016994374944,0.,0.951056516295155));
#36847=DIRECTION('center_axis',(-0.951056516295154,0.,-0.309016994374948));
#36848=DIRECTION('ref_axis',(-0.309016994374944,0.,0.951056516295155));
#36849=DIRECTION('',(0.951056516295154,0.,0.309016994374948));
#36850=DIRECTION('center_axis',(-0.951056516295154,0.,-0.309016994374948));
#36851=DIRECTION('ref_axis',(-0.309016994374944,0.,0.951056516295155));
#36852=DIRECTION('center_axis',(-0.951056516295154,0.,-0.309016994374948));
#36853=DIRECTION('ref_axis',(-0.309016994374948,0.,0.951056516295154));
#36854=DIRECTION('center_axis',(-0.951056516295154,0.,-0.309016994374948));
#36855=DIRECTION('ref_axis',(0.309016994374948,0.,-0.951056516295154));
#36856=DIRECTION('center_axis',(-0.951056516295154,0.,-0.309016994374948));
#36857=DIRECTION('ref_axis',(-0.309016994374948,0.,0.951056516295153));
#36858=DIRECTION('center_axis',(-0.951056516295154,0.,-0.309016994374948));
#36859=DIRECTION('ref_axis',(0.309016994374948,0.,-0.951056516295154));
#36860=DIRECTION('',(-0.951056516295153,0.,-0.309016994374948));
#36861=DIRECTION('center_axis',(0.951056516295154,0.,0.309016994374948));
#36862=DIRECTION('ref_axis',(0.309016994374948,0.,-0.951056516295154));
#36863=DIRECTION('center_axis',(0.951056516295154,0.,0.309016994374948));
#36864=DIRECTION('ref_axis',(0.309016994374948,0.,-0.951056516295154));
#36865=DIRECTION('center_axis',(-0.951056516295154,0.,-0.309016994374948));
#36866=DIRECTION('ref_axis',(0.309016994374948,0.,-0.951056516295153));
#36867=DIRECTION('',(0.218508012224404,0.707106781186568,-0.672498511963937));
#36868=DIRECTION('',(0.218508012224404,-0.707106781186569,-0.672498511963937));
#36869=DIRECTION('',(0.,-1.,0.));
#36870=DIRECTION('',(-0.218508012224404,-0.707106781186569,0.672498511963937));
#36871=DIRECTION('',(-0.218508012224404,0.707106781186568,0.672498511963937));
#36872=DIRECTION('',(0.,1.,0.));
#36873=DIRECTION('center_axis',(-0.951056516295154,0.,-0.309016994374948));
#36874=DIRECTION('ref_axis',(-0.309016994374944,0.,0.951056516295155));
#36875=DIRECTION('center_axis',(-0.951056516295154,0.,-0.309016994374948));
#36876=DIRECTION('ref_axis',(0.309016994374948,0.,-0.951056516295153));
#36877=DIRECTION('',(0.453990499739571,8.6595605623547E-17,0.891006524188356));
#36878=DIRECTION('center_axis',(-0.951056516295154,0.,-0.309016994374948));
#36879=DIRECTION('ref_axis',(-0.309016994374944,0.,0.951056516295155));
#36880=DIRECTION('center_axis',(-0.951056516295154,0.,-0.309016994374948));
#36881=DIRECTION('ref_axis',(0.309016994374948,0.,-0.951056516295153));
#36882=DIRECTION('',(0.951056516295153,0.,0.309016994374948));
#36883=DIRECTION('center_axis',(0.951056516295154,0.,0.309016994374948));
#36884=DIRECTION('ref_axis',(-0.309016994374944,0.,0.951056516295155));
#36885=DIRECTION('center_axis',(-0.951056516295154,0.,-0.309016994374948));
#36886=DIRECTION('ref_axis',(0.309016994374948,0.,-0.951056516295154));
#36887=DIRECTION('',(0.891006524188336,-8.65956056235554E-17,-0.453990499739609));
#36888=DIRECTION('center_axis',(-0.951056516295154,0.,-0.309016994374948));
#36889=DIRECTION('ref_axis',(-0.309016994374948,0.,0.951056516295154));
#36890=DIRECTION('center_axis',(-0.951056516295154,0.,-0.309016994374948));
#36891=DIRECTION('ref_axis',(0.309016994374948,0.,-0.951056516295153));
#36892=DIRECTION('center_axis',(-0.951056516295154,0.,-0.309016994374948));
#36893=DIRECTION('ref_axis',(-0.309016994374944,0.,0.951056516295155));
#36894=DIRECTION('',(0.951056516295154,0.,0.309016994374948));
#36895=DIRECTION('center_axis',(-0.218508012224417,0.707106781186526,0.672498511963978));
#36896=DIRECTION('ref_axis',(0.951056516295154,0.,0.309016994374947));
#36897=DIRECTION('',(0.951056516295154,0.,0.309016994374947));
#36898=DIRECTION('',(0.218508012224407,0.707106781186617,-0.672498511963885));
#36899=DIRECTION('center_axis',(-0.309016994374947,0.,0.951056516295154));
#36900=DIRECTION('ref_axis',(0.951056516295154,0.,0.309016994374947));
#36901=DIRECTION('',(-0.951056516295154,0.,-0.309016994374947));
#36902=DIRECTION('',(0.,1.,0.));
#36903=DIRECTION('center_axis',(-0.218508012224417,-0.707106781186526,0.672498511963978));
#36904=DIRECTION('ref_axis',(0.951056516295154,0.,0.309016994374947));
#36905=DIRECTION('',(0.218508012224413,-0.707106781186516,-0.67249851196399));
#36906=DIRECTION('center_axis',(0.,-1.,0.));
#36907=DIRECTION('ref_axis',(-0.309016994374959,0.,0.95105651629515));
#36908=DIRECTION('',(-0.218508012224428,0.707106781186564,0.672498511963935));
#36909=DIRECTION('center_axis',(0.,1.,0.));
#36910=DIRECTION('ref_axis',(-0.309016994374959,0.,0.95105651629515));
#36911=DIRECTION('center_axis',(0.218508012224416,0.707106781186527,-0.672498511963977));
#36912=DIRECTION('ref_axis',(-0.951056516295154,0.,-0.309016994374947));
#36913=DIRECTION('',(-0.951056516295154,0.,-0.309016994374947));
#36914=DIRECTION('center_axis',(0.,1.,0.));
#36915=DIRECTION('ref_axis',(-0.309016994374959,0.,0.95105651629515));
#36916=DIRECTION('center_axis',(0.,-1.,0.));
#36917=DIRECTION('ref_axis',(-0.309016994374959,0.,0.95105651629515));
#36918=DIRECTION('',(0.,1.,0.));
#36919=DIRECTION('center_axis',(0.218508012224416,-0.707106781186527,-0.672498511963977));
#36920=DIRECTION('ref_axis',(-0.951056516295154,0.,-0.309016994374947));
#36921=DIRECTION('',(0.951056516295154,0.,0.309016994374947));
#36922=DIRECTION('',(-0.21850801222441,-0.707106781186566,0.672498511963938));
#36923=DIRECTION('center_axis',(0.,1.,0.));
#36924=DIRECTION('ref_axis',(-0.309016994374959,0.,0.95105651629515));
#36925=DIRECTION('center_axis',(0.309016994374947,0.,-0.951056516295154));
#36926=DIRECTION('ref_axis',(-0.951056516295154,0.,-0.309016994374947));
#36927=DIRECTION('axis',(0.,0.,1.));
#36928=DIRECTION('refdir',(1.,0.,0.));
#36929=DIRECTION('center_axis',(0.,-1.,0.));
#36930=DIRECTION('ref_axis',(1.,0.,0.));
#36931=DIRECTION('center_axis',(0.,-1.,0.));
#36932=DIRECTION('ref_axis',(1.,0.,0.));
#36933=DIRECTION('',(0.707106781186552,0.707106781186543,8.65956056235499E-17));
#36934=DIRECTION('center_axis',(0.,1.,0.));
#36935=DIRECTION('ref_axis',(1.,0.,0.));
#36936=DIRECTION('center_axis',(0.,-1.,0.));
#36937=DIRECTION('ref_axis',(1.,0.,0.));
#36938=DIRECTION('',(-1.,0.,0.));
#36939=DIRECTION('',(0.,0.,-1.));
#36940=DIRECTION('',(1.,0.,0.));
#36941=DIRECTION('',(0.,0.,1.));
#36942=DIRECTION('center_axis',(0.,-1.,0.));
#36943=DIRECTION('ref_axis',(1.,0.,0.));
#36944=DIRECTION('center_axis',(0.,-1.,0.));
#36945=DIRECTION('ref_axis',(1.,0.,0.));
#36946=DIRECTION('center_axis',(0.,-1.,0.));
#36947=DIRECTION('ref_axis',(1.,0.,0.));
#36948=DIRECTION('center_axis',(0.,-1.,0.));
#36949=DIRECTION('ref_axis',(1.,0.,0.));
#36950=DIRECTION('center_axis',(0.,-1.,0.));
#36951=DIRECTION('ref_axis',(1.,0.,0.));
#36952=DIRECTION('center_axis',(0.,-1.,0.));
#36953=DIRECTION('ref_axis',(1.,0.,0.));
#36954=DIRECTION('center_axis',(0.,-1.,0.));
#36955=DIRECTION('ref_axis',(1.,0.,0.));
#36956=DIRECTION('center_axis',(0.,-1.,0.));
#36957=DIRECTION('ref_axis',(1.,0.,0.));
#36958=DIRECTION('center_axis',(0.,-1.,0.));
#36959=DIRECTION('ref_axis',(1.,0.,0.));
#36960=DIRECTION('center_axis',(0.,-1.,0.));
#36961=DIRECTION('ref_axis',(1.,0.,0.));
#36962=DIRECTION('center_axis',(0.,1.,0.));
#36963=DIRECTION('ref_axis',(1.,0.,0.));
#36964=DIRECTION('',(0.,1.,0.));
#36965=DIRECTION('center_axis',(0.,-1.,0.));
#36966=DIRECTION('ref_axis',(1.,0.,0.));
#36967=DIRECTION('center_axis',(0.,-1.,0.));
#36968=DIRECTION('ref_axis',(1.,0.,0.));
#36969=DIRECTION('',(0.707106781186552,0.707106781186543,8.65956056235499E-17));
#36970=DIRECTION('center_axis',(0.,1.,0.));
#36971=DIRECTION('ref_axis',(1.,0.,0.));
#36972=DIRECTION('center_axis',(0.,1.,0.));
#36973=DIRECTION('ref_axis',(1.,0.,0.));
#36974=DIRECTION('',(0.,1.,0.));
#36975=DIRECTION('center_axis',(0.,-1.,0.));
#36976=DIRECTION('ref_axis',(1.,0.,0.));
#36977=DIRECTION('center_axis',(0.,-1.,0.));
#36978=DIRECTION('ref_axis',(1.,0.,0.));
#36979=DIRECTION('',(0.707106781186552,0.707106781186543,8.65956056235499E-17));
#36980=DIRECTION('center_axis',(0.,1.,0.));
#36981=DIRECTION('ref_axis',(1.,0.,0.));
#36982=DIRECTION('center_axis',(0.,1.,0.));
#36983=DIRECTION('ref_axis',(1.,0.,0.));
#36984=DIRECTION('',(0.,1.,0.));
#36985=DIRECTION('center_axis',(0.,-1.,0.));
#36986=DIRECTION('ref_axis',(1.,0.,0.));
#36987=DIRECTION('center_axis',(0.,-1.,0.));
#36988=DIRECTION('ref_axis',(1.,0.,0.));
#36989=DIRECTION('',(0.707106781186552,0.707106781186543,8.65956056235499E-17));
#36990=DIRECTION('center_axis',(0.,1.,0.));
#36991=DIRECTION('ref_axis',(1.,0.,0.));
#36992=DIRECTION('center_axis',(0.,1.,0.));
#36993=DIRECTION('ref_axis',(1.,0.,0.));
#36994=DIRECTION('',(0.,1.,0.));
#36995=DIRECTION('center_axis',(0.,-1.,0.));
#36996=DIRECTION('ref_axis',(1.,0.,0.));
#36997=DIRECTION('center_axis',(0.,-1.,0.));
#36998=DIRECTION('ref_axis',(1.,0.,0.));
#36999=DIRECTION('',(0.707106781186552,0.707106781186543,8.65956056235499E-17));
#37000=DIRECTION('center_axis',(0.,1.,0.));
#37001=DIRECTION('ref_axis',(1.,0.,0.));
#37002=DIRECTION('center_axis',(0.,1.,0.));
#37003=DIRECTION('ref_axis',(1.,0.,0.));
#37004=DIRECTION('',(0.,1.,0.));
#37005=DIRECTION('center_axis',(0.,-1.,0.));
#37006=DIRECTION('ref_axis',(1.,0.,0.));
#37007=DIRECTION('center_axis',(0.,-1.,0.));
#37008=DIRECTION('ref_axis',(1.,0.,0.));
#37009=DIRECTION('',(0.707106781186552,0.707106781186543,8.65956056235499E-17));
#37010=DIRECTION('center_axis',(0.,1.,0.));
#37011=DIRECTION('ref_axis',(1.,0.,0.));
#37012=DIRECTION('center_axis',(0.,1.,0.));
#37013=DIRECTION('ref_axis',(1.,0.,0.));
#37014=DIRECTION('',(0.,1.,0.));
#37015=DIRECTION('center_axis',(0.,-1.,0.));
#37016=DIRECTION('ref_axis',(1.,0.,0.));
#37017=DIRECTION('center_axis',(0.,-1.,0.));
#37018=DIRECTION('ref_axis',(1.,0.,0.));
#37019=DIRECTION('',(0.707106781186552,0.707106781186543,8.65956056235499E-17));
#37020=DIRECTION('center_axis',(0.,1.,0.));
#37021=DIRECTION('ref_axis',(1.,0.,0.));
#37022=DIRECTION('center_axis',(0.,1.,0.));
#37023=DIRECTION('ref_axis',(1.,0.,0.));
#37024=DIRECTION('',(0.,1.,0.));
#37025=DIRECTION('center_axis',(0.,-1.,0.));
#37026=DIRECTION('ref_axis',(1.,0.,0.));
#37027=DIRECTION('center_axis',(0.,1.,0.));
#37028=DIRECTION('ref_axis',(1.,0.,0.));
#37029=DIRECTION('center_axis',(0.,1.,0.));
#37030=DIRECTION('ref_axis',(1.,0.,0.));
#37031=DIRECTION('',(0.707106781186552,-0.707106781186543,-8.65956056235499E-17));
#37032=DIRECTION('center_axis',(0.,-1.,0.));
#37033=DIRECTION('ref_axis',(1.,0.,0.));
#37034=DIRECTION('center_axis',(0.,1.,0.));
#37035=DIRECTION('ref_axis',(-1.,0.,0.));
#37036=DIRECTION('',(1.,0.,0.));
#37037=DIRECTION('',(0.,0.,-1.));
#37038=DIRECTION('',(-1.,0.,0.));
#37039=DIRECTION('',(0.,0.,1.));
#37040=DIRECTION('center_axis',(0.,1.,0.));
#37041=DIRECTION('ref_axis',(1.,0.,0.));
#37042=DIRECTION('center_axis',(0.,1.,0.));
#37043=DIRECTION('ref_axis',(1.,0.,0.));
#37044=DIRECTION('center_axis',(0.,1.,0.));
#37045=DIRECTION('ref_axis',(1.,0.,0.));
#37046=DIRECTION('center_axis',(0.,1.,0.));
#37047=DIRECTION('ref_axis',(1.,0.,0.));
#37048=DIRECTION('center_axis',(0.,1.,0.));
#37049=DIRECTION('ref_axis',(1.,0.,0.));
#37050=DIRECTION('center_axis',(0.,1.,0.));
#37051=DIRECTION('ref_axis',(1.,0.,0.));
#37052=DIRECTION('center_axis',(0.,1.,0.));
#37053=DIRECTION('ref_axis',(1.,0.,0.));
#37054=DIRECTION('center_axis',(0.,1.,0.));
#37055=DIRECTION('ref_axis',(1.,0.,0.));
#37056=DIRECTION('center_axis',(0.,1.,0.));
#37057=DIRECTION('ref_axis',(1.,0.,0.));
#37058=DIRECTION('center_axis',(0.,1.,0.));
#37059=DIRECTION('ref_axis',(1.,0.,0.));
#37060=DIRECTION('center_axis',(0.,1.,0.));
#37061=DIRECTION('ref_axis',(1.,0.,0.));
#37062=DIRECTION('center_axis',(0.,1.,0.));
#37063=DIRECTION('ref_axis',(1.,0.,0.));
#37064=DIRECTION('',(0.,1.,0.));
#37065=DIRECTION('center_axis',(0.,1.,0.));
#37066=DIRECTION('ref_axis',(1.,0.,0.));
#37067=DIRECTION('',(0.707106781186552,-0.707106781186543,-8.65956056235499E-17));
#37068=DIRECTION('center_axis',(0.,-1.,0.));
#37069=DIRECTION('ref_axis',(1.,0.,0.));
#37070=DIRECTION('center_axis',(0.,1.,0.));
#37071=DIRECTION('ref_axis',(1.,0.,0.));
#37072=DIRECTION('center_axis',(0.,1.,0.));
#37073=DIRECTION('ref_axis',(1.,0.,0.));
#37074=DIRECTION('',(0.,1.,0.));
#37075=DIRECTION('center_axis',(0.,1.,0.));
#37076=DIRECTION('ref_axis',(1.,0.,0.));
#37077=DIRECTION('',(0.707106781186552,-0.707106781186543,-8.65956056235499E-17));
#37078=DIRECTION('center_axis',(0.,-1.,0.));
#37079=DIRECTION('ref_axis',(1.,0.,0.));
#37080=DIRECTION('center_axis',(0.,1.,0.));
#37081=DIRECTION('ref_axis',(1.,0.,0.));
#37082=DIRECTION('center_axis',(0.,1.,0.));
#37083=DIRECTION('ref_axis',(1.,0.,0.));
#37084=DIRECTION('',(0.,1.,0.));
#37085=DIRECTION('center_axis',(0.,1.,0.));
#37086=DIRECTION('ref_axis',(1.,0.,0.));
#37087=DIRECTION('',(0.707106781186552,-0.707106781186543,-8.65956056235499E-17));
#37088=DIRECTION('center_axis',(0.,-1.,0.));
#37089=DIRECTION('ref_axis',(1.,0.,0.));
#37090=DIRECTION('center_axis',(0.,1.,0.));
#37091=DIRECTION('ref_axis',(1.,0.,0.));
#37092=DIRECTION('center_axis',(0.,1.,0.));
#37093=DIRECTION('ref_axis',(1.,0.,0.));
#37094=DIRECTION('',(0.,1.,0.));
#37095=DIRECTION('center_axis',(0.,1.,0.));
#37096=DIRECTION('ref_axis',(1.,0.,0.));
#37097=DIRECTION('',(0.707106781186552,-0.707106781186543,-8.65956056235499E-17));
#37098=DIRECTION('center_axis',(0.,-1.,0.));
#37099=DIRECTION('ref_axis',(1.,0.,0.));
#37100=DIRECTION('center_axis',(0.,1.,0.));
#37101=DIRECTION('ref_axis',(1.,0.,0.));
#37102=DIRECTION('center_axis',(0.,1.,0.));
#37103=DIRECTION('ref_axis',(1.,0.,0.));
#37104=DIRECTION('',(0.,1.,0.));
#37105=DIRECTION('center_axis',(0.,0.707106781186548,-0.707106781186548));
#37106=DIRECTION('ref_axis',(-1.,0.,0.));
#37107=DIRECTION('',(0.,0.707106781186548,0.707106781186548));
#37108=DIRECTION('',(0.,-0.707106781186548,-0.707106781186548));
#37109=DIRECTION('',(-1.,0.,0.));
#37110=DIRECTION('center_axis',(0.,0.,-1.));
#37111=DIRECTION('ref_axis',(-0.707106781186553,-0.707106781186542,0.));
#37112=DIRECTION('',(0.707106781186565,0.,0.70710678118653));
#37113=DIRECTION('center_axis',(0.,0.,1.));
#37114=DIRECTION('ref_axis',(-0.707106781186553,-0.707106781186542,0.));
#37115=DIRECTION('center_axis',(0.,0.,-1.));
#37116=DIRECTION('ref_axis',(-0.707106781186553,-0.707106781186542,0.));
#37117=DIRECTION('center_axis',(0.707106781186543,0.,-0.707106781186552));
#37118=DIRECTION('ref_axis',(-0.707106781186552,0.,-0.707106781186543));
#37119=DIRECTION('',(0.707106781186552,0.,0.707106781186543));
#37120=DIRECTION('',(0.,-1.,0.));
#37121=DIRECTION('',(0.,1.,0.));
#37122=DIRECTION('center_axis',(0.,0.,-1.));
#37123=DIRECTION('ref_axis',(-0.707106781186544,0.707106781186551,0.));
#37124=DIRECTION('',(0.,-0.707106781186546,0.707106781186549));
#37125=DIRECTION('center_axis',(0.,0.,1.));
#37126=DIRECTION('ref_axis',(-0.707106781186544,0.707106781186551,0.));
#37127=DIRECTION('center_axis',(0.,0.,-1.));
#37128=DIRECTION('ref_axis',(-0.707106781186544,0.707106781186551,0.));
#37129=DIRECTION('center_axis',(0.,-0.707106781186548,-0.707106781186548));
#37130=DIRECTION('ref_axis',(-1.,0.,0.));
#37131=DIRECTION('',(0.,-0.707106781186548,0.707106781186548));
#37132=DIRECTION('',(1.,0.,0.));
#37133=DIRECTION('center_axis',(0.,0.,-1.));
#37134=DIRECTION('ref_axis',(0.707106781186544,0.707106781186551,0.));
#37135=DIRECTION('',(-0.707106781186577,0.,0.707106781186518));
#37136=DIRECTION('center_axis',(0.,0.,1.));
#37137=DIRECTION('ref_axis',(0.707106781186544,0.707106781186551,0.));
#37138=DIRECTION('center_axis',(0.,0.,-1.));
#37139=DIRECTION('ref_axis',(0.707106781186544,0.707106781186551,0.));
#37140=DIRECTION('center_axis',(-0.707106781186543,0.,-0.707106781186552));
#37141=DIRECTION('ref_axis',(-0.707106781186552,0.,0.707106781186543));
#37142=DIRECTION('',(-0.707106781186552,0.,0.707106781186543));
#37143=DIRECTION('',(0.,1.,0.));
#37144=DIRECTION('',(0.,-1.,0.));
#37145=DIRECTION('center_axis',(0.,0.,-1.));
#37146=DIRECTION('ref_axis',(0.707106781186544,-0.707106781186551,0.));
#37147=DIRECTION('center_axis',(0.,0.,1.));
#37148=DIRECTION('ref_axis',(0.707106781186544,-0.707106781186551,0.));
#37149=DIRECTION('center_axis',(0.,0.,-1.));
#37150=DIRECTION('ref_axis',(0.707106781186544,-0.707106781186551,0.));
#37151=DIRECTION('center_axis',(0.,0.,1.));
#37152=DIRECTION('ref_axis',(0.707106781186544,0.707106781186551,0.));
#37153=DIRECTION('',(0.,0.,1.));
#37154=DIRECTION('center_axis',(0.,0.,-1.));
#37155=DIRECTION('ref_axis',(0.707106781186544,0.707106781186551,0.));
#37156=DIRECTION('center_axis',(-1.,0.,0.));
#37157=DIRECTION('ref_axis',(0.,-1.,0.));
#37158=DIRECTION('',(0.,0.,-1.));
#37159=DIRECTION('',(0.,-1.,0.));
#37160=DIRECTION('center_axis',(0.,0.,1.));
#37161=DIRECTION('ref_axis',(0.707106781186544,-0.707106781186551,0.));
#37162=DIRECTION('center_axis',(0.,0.,-1.));
#37163=DIRECTION('ref_axis',(0.707106781186544,-0.707106781186551,0.));
#37164=DIRECTION('center_axis',(0.,0.,1.));
#37165=DIRECTION('ref_axis',(1.,0.,0.));
#37166=DIRECTION('',(-1.,0.,0.));
#37167=DIRECTION('center_axis',(0.,0.,1.));
#37168=DIRECTION('ref_axis',(0.707106781186546,0.707106781186549,0.));
#37169=DIRECTION('',(0.,1.,0.));
#37170=DIRECTION('center_axis',(0.,0.,1.));
#37171=DIRECTION('ref_axis',(0.707106781186546,-0.707106781186549,0.));
#37172=DIRECTION('',(1.,0.,0.));
#37173=DIRECTION('center_axis',(0.,0.,1.));
#37174=DIRECTION('ref_axis',(-0.707106781186546,-0.707106781186549,0.));
#37175=DIRECTION('',(0.,-1.,0.));
#37176=DIRECTION('center_axis',(0.,0.,1.));
#37177=DIRECTION('ref_axis',(-0.707106781186549,0.707106781186546,0.));
#37178=DIRECTION('center_axis',(0.,1.,0.));
#37179=DIRECTION('ref_axis',(1.,0.,0.));
#37180=DIRECTION('',(0.707106781186552,-0.707106781186543,-8.65956056235499E-17));
#37181=DIRECTION('center_axis',(0.,-1.,0.));
#37182=DIRECTION('ref_axis',(1.,0.,0.));
#37183=DIRECTION('center_axis',(0.,1.,0.));
#37184=DIRECTION('ref_axis',(1.,0.,0.));
#37185=DIRECTION('center_axis',(0.,1.,0.));
#37186=DIRECTION('ref_axis',(1.,0.,0.));
#37187=DIRECTION('',(0.,1.,0.));
#37188=DIRECTION('center_axis',(0.,1.,0.));
#37189=DIRECTION('ref_axis',(1.,0.,0.));
#37190=DIRECTION('',(0.707106781186552,-0.707106781186543,-8.65956056235499E-17));
#37191=DIRECTION('center_axis',(0.,-1.,0.));
#37192=DIRECTION('ref_axis',(1.,0.,0.));
#37193=DIRECTION('center_axis',(0.,1.,0.));
#37194=DIRECTION('ref_axis',(1.,0.,0.));
#37195=DIRECTION('center_axis',(0.,1.,0.));
#37196=DIRECTION('ref_axis',(1.,0.,0.));
#37197=DIRECTION('',(0.,1.,0.));
#37198=DIRECTION('center_axis',(0.,1.,0.));
#37199=DIRECTION('ref_axis',(1.,0.,0.));
#37200=DIRECTION('',(0.707106781186552,-0.707106781186543,-8.65956056235499E-17));
#37201=DIRECTION('center_axis',(0.,-1.,0.));
#37202=DIRECTION('ref_axis',(1.,0.,0.));
#37203=DIRECTION('center_axis',(0.,1.,0.));
#37204=DIRECTION('ref_axis',(1.,0.,0.));
#37205=DIRECTION('center_axis',(0.,1.,0.));
#37206=DIRECTION('ref_axis',(1.,0.,0.));
#37207=DIRECTION('',(0.,1.,0.));
#37208=DIRECTION('center_axis',(0.,-1.,0.));
#37209=DIRECTION('ref_axis',(1.,0.,0.));
#37210=DIRECTION('',(0.707106781186552,0.707106781186543,8.65956056235499E-17));
#37211=DIRECTION('center_axis',(0.,1.,0.));
#37212=DIRECTION('ref_axis',(1.,0.,0.));
#37213=DIRECTION('center_axis',(0.,1.,0.));
#37214=DIRECTION('ref_axis',(1.,0.,0.));
#37215=DIRECTION('',(0.,1.,0.));
#37216=DIRECTION('center_axis',(0.,-1.,0.));
#37217=DIRECTION('ref_axis',(1.,0.,0.));
#37218=DIRECTION('center_axis',(0.,1.,0.));
#37219=DIRECTION('ref_axis',(1.,0.,0.));
#37220=DIRECTION('',(0.707106781186552,-0.707106781186543,-8.65956056235499E-17));
#37221=DIRECTION('center_axis',(0.,-1.,0.));
#37222=DIRECTION('ref_axis',(1.,0.,0.));
#37223=DIRECTION('center_axis',(0.,1.,0.));
#37224=DIRECTION('ref_axis',(1.,0.,0.));
#37225=DIRECTION('center_axis',(0.,1.,0.));
#37226=DIRECTION('ref_axis',(1.,0.,0.));
#37227=DIRECTION('',(0.,1.,0.));
#37228=DIRECTION('center_axis',(0.,-1.,0.));
#37229=DIRECTION('ref_axis',(1.,0.,0.));
#37230=DIRECTION('',(0.707106781186552,0.707106781186543,8.65956056235499E-17));
#37231=DIRECTION('center_axis',(0.,1.,0.));
#37232=DIRECTION('ref_axis',(1.,0.,0.));
#37233=DIRECTION('center_axis',(0.,1.,0.));
#37234=DIRECTION('ref_axis',(1.,0.,0.));
#37235=DIRECTION('',(0.,1.,0.));
#37236=DIRECTION('center_axis',(0.,-1.,0.));
#37237=DIRECTION('ref_axis',(1.,0.,0.));
#37238=DIRECTION('center_axis',(0.,1.,0.));
#37239=DIRECTION('ref_axis',(1.,0.,0.));
#37240=DIRECTION('',(0.707106781186552,-0.707106781186543,-8.65956056235499E-17));
#37241=DIRECTION('center_axis',(0.,-1.,0.));
#37242=DIRECTION('ref_axis',(1.,0.,0.));
#37243=DIRECTION('center_axis',(0.,1.,0.));
#37244=DIRECTION('ref_axis',(1.,0.,0.));
#37245=DIRECTION('center_axis',(0.,1.,0.));
#37246=DIRECTION('ref_axis',(1.,0.,0.));
#37247=DIRECTION('',(0.,1.,0.));
#37248=DIRECTION('center_axis',(0.,-1.,0.));
#37249=DIRECTION('ref_axis',(1.,0.,0.));
#37250=DIRECTION('',(0.707106781186552,0.707106781186543,8.65956056235499E-17));
#37251=DIRECTION('center_axis',(0.,1.,0.));
#37252=DIRECTION('ref_axis',(1.,0.,0.));
#37253=DIRECTION('center_axis',(0.,1.,0.));
#37254=DIRECTION('ref_axis',(1.,0.,0.));
#37255=DIRECTION('',(0.,1.,0.));
#37256=DIRECTION('center_axis',(0.,-1.,0.));
#37257=DIRECTION('ref_axis',(1.,0.,0.));
#37258=DIRECTION('center_axis',(0.,1.,0.));
#37259=DIRECTION('ref_axis',(1.,0.,0.));
#37260=DIRECTION('',(0.707106781186552,-0.707106781186543,-8.65956056235499E-17));
#37261=DIRECTION('center_axis',(0.,-1.,0.));
#37262=DIRECTION('ref_axis',(1.,0.,0.));
#37263=DIRECTION('center_axis',(0.,1.,0.));
#37264=DIRECTION('ref_axis',(1.,0.,0.));
#37265=DIRECTION('center_axis',(0.,1.,0.));
#37266=DIRECTION('ref_axis',(1.,0.,0.));
#37267=DIRECTION('',(0.,1.,0.));
#37268=DIRECTION('center_axis',(0.,-1.,0.));
#37269=DIRECTION('ref_axis',(1.,0.,0.));
#37270=DIRECTION('center_axis',(0.,-1.,0.));
#37271=DIRECTION('ref_axis',(1.,0.,0.));
#37272=DIRECTION('',(0.707106781186552,0.707106781186543,8.65956056235499E-17));
#37273=DIRECTION('center_axis',(0.,-1.,0.));
#37274=DIRECTION('ref_axis',(1.,0.,0.));
#37275=DIRECTION('',(-1.,0.,0.));
#37276=DIRECTION('',(0.,0.,-1.));
#37277=DIRECTION('',(1.,0.,0.));
#37278=DIRECTION('',(0.,0.,1.));
#37279=DIRECTION('center_axis',(0.,-1.,0.));
#37280=DIRECTION('ref_axis',(1.,0.,0.));
#37281=DIRECTION('center_axis',(0.,-1.,0.));
#37282=DIRECTION('ref_axis',(1.,0.,0.));
#37283=DIRECTION('center_axis',(0.,-1.,0.));
#37284=DIRECTION('ref_axis',(1.,0.,0.));
#37285=DIRECTION('center_axis',(0.,-1.,0.));
#37286=DIRECTION('ref_axis',(1.,0.,0.));
#37287=DIRECTION('center_axis',(0.,-1.,0.));
#37288=DIRECTION('ref_axis',(1.,0.,0.));
#37289=DIRECTION('center_axis',(0.,-1.,0.));
#37290=DIRECTION('ref_axis',(1.,0.,0.));
#37291=DIRECTION('center_axis',(0.,-1.,0.));
#37292=DIRECTION('ref_axis',(1.,0.,0.));
#37293=DIRECTION('center_axis',(0.,-1.,0.));
#37294=DIRECTION('ref_axis',(1.,0.,0.));
#37295=DIRECTION('center_axis',(0.,-1.,0.));
#37296=DIRECTION('ref_axis',(1.,0.,0.));
#37297=DIRECTION('center_axis',(0.,-1.,0.));
#37298=DIRECTION('ref_axis',(1.,0.,0.));
#37299=DIRECTION('center_axis',(0.,-1.,0.));
#37300=DIRECTION('ref_axis',(1.,0.,0.));
#37301=DIRECTION('',(0.707106781186552,0.707106781186543,8.65956056235499E-17));
#37302=DIRECTION('center_axis',(0.,-1.,0.));
#37303=DIRECTION('ref_axis',(1.,0.,0.));
#37304=DIRECTION('',(0.707106781186552,0.707106781186543,8.65956056235499E-17));
#37305=DIRECTION('center_axis',(0.,-1.,0.));
#37306=DIRECTION('ref_axis',(1.,0.,0.));
#37307=DIRECTION('',(0.707106781186552,0.707106781186543,8.65956056235499E-17));
#37308=DIRECTION('center_axis',(0.,-1.,0.));
#37309=DIRECTION('ref_axis',(1.,0.,0.));
#37310=DIRECTION('',(0.707106781186552,0.707106781186543,8.65956056235499E-17));
#37311=DIRECTION('center_axis',(0.,-1.,0.));
#37312=DIRECTION('ref_axis',(1.,0.,0.));
#37313=DIRECTION('',(0.707106781186552,0.707106781186543,8.65956056235499E-17));
#37314=DIRECTION('center_axis',(0.,1.,0.));
#37315=DIRECTION('ref_axis',(1.,0.,0.));
#37316=DIRECTION('center_axis',(0.,1.,0.));
#37317=DIRECTION('ref_axis',(1.,0.,0.));
#37318=DIRECTION('',(0.,1.,0.));
#37319=DIRECTION('center_axis',(0.,-1.,0.));
#37320=DIRECTION('ref_axis',(1.,0.,0.));
#37321=DIRECTION('center_axis',(0.,1.,0.));
#37322=DIRECTION('ref_axis',(1.,0.,0.));
#37323=DIRECTION('center_axis',(0.,1.,0.));
#37324=DIRECTION('ref_axis',(1.,0.,0.));
#37325=DIRECTION('',(0.707106781186552,-0.707106781186543,-8.65956056235499E-17));
#37326=DIRECTION('center_axis',(0.,1.,0.));
#37327=DIRECTION('ref_axis',(-1.,0.,0.));
#37328=DIRECTION('',(1.,0.,0.));
#37329=DIRECTION('',(0.,0.,-1.));
#37330=DIRECTION('',(-1.,0.,0.));
#37331=DIRECTION('',(0.,0.,1.));
#37332=DIRECTION('center_axis',(0.,1.,0.));
#37333=DIRECTION('ref_axis',(1.,0.,0.));
#37334=DIRECTION('center_axis',(0.,1.,0.));
#37335=DIRECTION('ref_axis',(1.,0.,0.));
#37336=DIRECTION('center_axis',(0.,1.,0.));
#37337=DIRECTION('ref_axis',(1.,0.,0.));
#37338=DIRECTION('center_axis',(0.,1.,0.));
#37339=DIRECTION('ref_axis',(1.,0.,0.));
#37340=DIRECTION('center_axis',(0.,1.,0.));
#37341=DIRECTION('ref_axis',(1.,0.,0.));
#37342=DIRECTION('center_axis',(0.,1.,0.));
#37343=DIRECTION('ref_axis',(1.,0.,0.));
#37344=DIRECTION('center_axis',(0.,1.,0.));
#37345=DIRECTION('ref_axis',(1.,0.,0.));
#37346=DIRECTION('center_axis',(0.,1.,0.));
#37347=DIRECTION('ref_axis',(1.,0.,0.));
#37348=DIRECTION('center_axis',(0.,1.,0.));
#37349=DIRECTION('ref_axis',(1.,0.,0.));
#37350=DIRECTION('center_axis',(0.,1.,0.));
#37351=DIRECTION('ref_axis',(1.,0.,0.));
#37352=DIRECTION('center_axis',(0.,1.,0.));
#37353=DIRECTION('ref_axis',(1.,0.,0.));
#37354=DIRECTION('',(0.707106781186552,-0.707106781186543,-8.65956056235499E-17));
#37355=DIRECTION('center_axis',(0.,1.,0.));
#37356=DIRECTION('ref_axis',(1.,0.,0.));
#37357=DIRECTION('',(0.707106781186552,-0.707106781186543,-8.65956056235499E-17));
#37358=DIRECTION('center_axis',(0.,1.,0.));
#37359=DIRECTION('ref_axis',(1.,0.,0.));
#37360=DIRECTION('',(0.707106781186552,-0.707106781186543,-8.65956056235499E-17));
#37361=DIRECTION('center_axis',(0.,1.,0.));
#37362=DIRECTION('ref_axis',(1.,0.,0.));
#37363=DIRECTION('',(0.707106781186552,-0.707106781186543,-8.65956056235499E-17));
#37364=DIRECTION('center_axis',(0.,0.707106781186548,-0.707106781186548));
#37365=DIRECTION('ref_axis',(-1.,0.,0.));
#37366=DIRECTION('',(0.,0.707106781186548,0.707106781186548));
#37367=DIRECTION('',(0.,-0.707106781186548,-0.707106781186548));
#37368=DIRECTION('center_axis',(0.,0.,1.));
#37369=DIRECTION('ref_axis',(-0.707106781186549,0.707106781186546,0.));
#37370=DIRECTION('',(-0.707106781186552,0.,0.707106781186543));
#37371=DIRECTION('center_axis',(0.,0.,-1.));
#37372=DIRECTION('ref_axis',(-0.70710678118655,0.707106781186546,0.));
#37373=DIRECTION('center_axis',(-0.707106781186543,0.,-0.707106781186552));
#37374=DIRECTION('ref_axis',(-0.707106781186552,0.,0.707106781186543));
#37375=DIRECTION('',(-0.707106781186552,0.,0.707106781186543));
#37376=DIRECTION('',(0.,1.,0.));
#37377=DIRECTION('center_axis',(0.,0.,1.));
#37378=DIRECTION('ref_axis',(-0.707106781186546,-0.707106781186549,0.));
#37379=DIRECTION('',(0.,-0.707106781186544,0.707106781186551));
#37380=DIRECTION('center_axis',(0.,0.,-1.));
#37381=DIRECTION('ref_axis',(-0.707106781186546,-0.707106781186549,0.));
#37382=DIRECTION('center_axis',(0.,-0.707106781186548,-0.707106781186548));
#37383=DIRECTION('ref_axis',(-1.,0.,0.));
#37384=DIRECTION('',(0.,-0.707106781186548,0.707106781186548));
#37385=DIRECTION('center_axis',(0.,0.,1.));
#37386=DIRECTION('ref_axis',(0.707106781186546,-0.707106781186549,0.));
#37387=DIRECTION('',(0.707106781186552,0.,0.707106781186543));
#37388=DIRECTION('center_axis',(0.,0.,-1.));
#37389=DIRECTION('ref_axis',(0.707106781186546,-0.707106781186549,0.));
#37390=DIRECTION('center_axis',(0.707106781186543,0.,-0.707106781186552));
#37391=DIRECTION('ref_axis',(-0.707106781186552,0.,-0.707106781186543));
#37392=DIRECTION('',(0.707106781186552,0.,0.707106781186543));
#37393=DIRECTION('',(0.,-1.,0.));
#37394=DIRECTION('center_axis',(0.,0.,1.));
#37395=DIRECTION('ref_axis',(0.707106781186546,0.707106781186549,0.));
#37396=DIRECTION('center_axis',(0.,0.,-1.));
#37397=DIRECTION('ref_axis',(0.707106781186546,0.707106781186549,0.));
#37398=DIRECTION('center_axis',(0.,0.,1.));
#37399=DIRECTION('ref_axis',(0.707106781186546,-0.707106781186549,0.));
#37400=DIRECTION('',(0.,0.,1.));
#37401=DIRECTION('center_axis',(0.,0.,1.));
#37402=DIRECTION('ref_axis',(0.707106781186546,-0.707106781186549,0.));
#37403=DIRECTION('center_axis',(1.,0.,0.));
#37404=DIRECTION('ref_axis',(0.,1.,0.));
#37405=DIRECTION('',(0.,0.,-1.));
#37406=DIRECTION('',(0.,1.,0.));
#37407=DIRECTION('center_axis',(0.,0.,1.));
#37408=DIRECTION('ref_axis',(0.707106781186546,0.707106781186549,0.));
#37409=DIRECTION('center_axis',(0.,0.,1.));
#37410=DIRECTION('ref_axis',(0.707106781186546,0.707106781186549,0.));
#37411=DIRECTION('center_axis',(0.,1.,0.));
#37412=DIRECTION('ref_axis',(1.,0.,0.));
#37413=DIRECTION('',(0.707106781186552,-0.707106781186543,-8.65956056235499E-17));
#37414=DIRECTION('center_axis',(0.,-1.,0.));
#37415=DIRECTION('ref_axis',(1.,0.,0.));
#37416=DIRECTION('',(0.707106781186552,0.707106781186543,8.65956056235499E-17));
#37417=DIRECTION('center_axis',(0.,1.,0.));
#37418=DIRECTION('ref_axis',(1.,0.,0.));
#37419=DIRECTION('',(0.707106781186552,-0.707106781186543,-8.65956056235499E-17));
#37420=DIRECTION('center_axis',(0.,-1.,0.));
#37421=DIRECTION('ref_axis',(1.,0.,0.));
#37422=DIRECTION('',(0.707106781186552,0.707106781186543,8.65956056235499E-17));
#37423=DIRECTION('center_axis',(0.,1.,0.));
#37424=DIRECTION('ref_axis',(1.,0.,0.));
#37425=DIRECTION('',(0.707106781186552,-0.707106781186543,-8.65956056235499E-17));
#37426=DIRECTION('center_axis',(0.,-1.,0.));
#37427=DIRECTION('ref_axis',(1.,0.,0.));
#37428=DIRECTION('',(0.707106781186552,0.707106781186543,8.65956056235499E-17));
#37429=DIRECTION('center_axis',(0.,1.,0.));
#37430=DIRECTION('ref_axis',(1.,0.,0.));
#37431=DIRECTION('',(0.707106781186552,-0.707106781186543,-8.65956056235499E-17));
#37432=DIRECTION('center_axis',(0.,-1.,0.));
#37433=DIRECTION('ref_axis',(1.,0.,0.));
#37434=DIRECTION('',(0.707106781186552,0.707106781186543,8.65956056235499E-17));
#37435=DIRECTION('center_axis',(0.,1.,0.));
#37436=DIRECTION('ref_axis',(1.,0.,0.));
#37437=DIRECTION('',(0.707106781186552,-0.707106781186543,-8.65956056235499E-17));
#37438=DIRECTION('center_axis',(0.,-1.,0.));
#37439=DIRECTION('ref_axis',(1.,0.,0.));
#37440=DIRECTION('',(0.707106781186552,0.707106781186543,8.65956056235499E-17));
#37441=DIRECTION('center_axis',(0.,1.,0.));
#37442=DIRECTION('ref_axis',(1.,0.,0.));
#37443=DIRECTION('',(0.707106781186552,-0.707106781186543,-8.65956056235499E-17));
#37444=DIRECTION('center_axis',(0.,-1.,0.));
#37445=DIRECTION('ref_axis',(1.,0.,0.));
#37446=DIRECTION('',(0.707106781186552,0.707106781186543,8.65956056235499E-17));
#37447=DIRECTION('center_axis',(0.,0.,-1.));
#37448=DIRECTION('ref_axis',(-0.707106781186546,-0.707106781186549,0.));
#37449=DIRECTION('',(-0.70710678118656,0.,-0.707106781186535));
#37450=DIRECTION('center_axis',(0.,0.,1.));
#37451=DIRECTION('ref_axis',(-0.707106781186546,-0.707106781186549,0.));
#37452=DIRECTION('',(0.,0.707106781186565,0.70710678118653));
#37453=DIRECTION('center_axis',(0.,0.,-1.));
#37454=DIRECTION('ref_axis',(-0.707106781186546,-0.707106781186549,0.));
#37455=DIRECTION('center_axis',(-0.707106781186522,0.,0.707106781186573));
#37456=DIRECTION('ref_axis',(0.707106781186573,0.,0.707106781186522));
#37457=DIRECTION('',(0.,1.,0.));
#37458=DIRECTION('',(-0.707106781186573,0.,-0.707106781186522));
#37459=DIRECTION('',(0.,-1.,0.));
#37460=DIRECTION('center_axis',(0.,0.,-1.));
#37461=DIRECTION('ref_axis',(-0.707106781186549,0.707106781186546,0.));
#37462=DIRECTION('',(0.,0.707106781186565,-0.70710678118653));
#37463=DIRECTION('center_axis',(0.,0.,1.));
#37464=DIRECTION('ref_axis',(-0.70710678118655,0.707106781186546,0.));
#37465=DIRECTION('center_axis',(0.,0.,-1.));
#37466=DIRECTION('ref_axis',(-0.707106781186549,0.707106781186546,0.));
#37467=DIRECTION('center_axis',(0.,0.707106781186527,0.707106781186568));
#37468=DIRECTION('ref_axis',(1.,0.,0.));
#37469=DIRECTION('',(1.,0.,0.));
#37470=DIRECTION('',(0.,0.707106781186568,-0.707106781186527));
#37471=DIRECTION('center_axis',(0.,0.,-1.));
#37472=DIRECTION('ref_axis',(0.707106781186546,0.707106781186549,0.));
#37473=DIRECTION('',(0.707106781186573,0.,-0.707106781186522));
#37474=DIRECTION('center_axis',(0.,0.,-1.));
#37475=DIRECTION('ref_axis',(0.707106781186546,0.707106781186549,0.));
#37476=DIRECTION('center_axis',(0.707106781186522,0.,0.707106781186573));
#37477=DIRECTION('ref_axis',(0.707106781186573,0.,-0.707106781186522));
#37478=DIRECTION('',(0.,-1.,0.));
#37479=DIRECTION('',(0.707106781186573,0.,-0.707106781186522));
#37480=DIRECTION('center_axis',(0.,0.,-1.));
#37481=DIRECTION('ref_axis',(0.707106781186546,-0.707106781186549,0.));
#37482=DIRECTION('',(0.,-0.707106781186579,-0.707106781186516));
#37483=DIRECTION('center_axis',(0.,0.,-1.));
#37484=DIRECTION('ref_axis',(0.707106781186546,-0.707106781186549,0.));
#37485=DIRECTION('center_axis',(0.,-0.707106781186527,0.707106781186568));
#37486=DIRECTION('ref_axis',(1.,0.,0.));
#37487=DIRECTION('',(-1.,0.,0.));
#37488=DIRECTION('center_axis',(0.,0.,1.));
#37489=DIRECTION('ref_axis',(-0.707106781186546,-0.707106781186549,0.));
#37490=DIRECTION('',(0.,0.,-1.));
#37491=DIRECTION('center_axis',(0.,0.,1.));
#37492=DIRECTION('ref_axis',(1.,0.,0.));
#37493=DIRECTION('center_axis',(0.,0.,1.));
#37494=DIRECTION('ref_axis',(-0.707106781186544,0.707106781186551,0.));
#37495=DIRECTION('',(-1.,0.,0.));
#37496=DIRECTION('center_axis',(0.,0.,1.));
#37497=DIRECTION('ref_axis',(0.707106781186544,0.707106781186551,0.));
#37498=DIRECTION('',(0.,1.,0.));
#37499=DIRECTION('center_axis',(0.,0.,1.));
#37500=DIRECTION('ref_axis',(0.707106781186544,-0.707106781186551,0.));
#37501=DIRECTION('',(1.,0.,0.));
#37502=DIRECTION('center_axis',(0.,0.,1.));
#37503=DIRECTION('ref_axis',(-0.707106781186553,-0.707106781186542,0.));
#37504=DIRECTION('',(0.,-1.,0.));
#37505=DIRECTION('center_axis',(0.,0.,1.));
#37506=DIRECTION('ref_axis',(-0.707106781186544,0.707106781186551,0.));
#37507=DIRECTION('',(0.707106781186585,0.,-0.70710678118651));
#37508=DIRECTION('center_axis',(0.,0.,-1.));
#37509=DIRECTION('ref_axis',(-0.707106781186544,0.707106781186551,0.));
#37510=DIRECTION('',(0.,0.707106781186566,0.707106781186529));
#37511=DIRECTION('center_axis',(0.707106781186522,0.,0.707106781186573));
#37512=DIRECTION('ref_axis',(0.707106781186573,0.,-0.707106781186522));
#37513=DIRECTION('',(0.707106781186573,0.,-0.707106781186522));
#37514=DIRECTION('',(0.,1.,0.));
#37515=DIRECTION('center_axis',(0.,0.,1.));
#37516=DIRECTION('ref_axis',(-0.707106781186553,-0.707106781186542,0.));
#37517=DIRECTION('',(0.,0.707106781186584,-0.707106781186511));
#37518=DIRECTION('center_axis',(0.,0.,-1.));
#37519=DIRECTION('ref_axis',(-0.707106781186553,-0.707106781186542,0.));
#37520=DIRECTION('center_axis',(0.,0.707106781186527,0.707106781186568));
#37521=DIRECTION('ref_axis',(1.,0.,0.));
#37522=DIRECTION('',(0.,0.707106781186568,-0.707106781186527));
#37523=DIRECTION('center_axis',(0.,0.,1.));
#37524=DIRECTION('ref_axis',(0.707106781186544,-0.707106781186551,0.));
#37525=DIRECTION('',(-0.707106781186598,0.,-0.707106781186497));
#37526=DIRECTION('center_axis',(-0.707106781186522,0.,0.707106781186573));
#37527=DIRECTION('ref_axis',(0.707106781186573,0.,0.707106781186522));
#37528=DIRECTION('',(-0.707106781186573,0.,-0.707106781186522));
#37529=DIRECTION('center_axis',(0.,0.,1.));
#37530=DIRECTION('ref_axis',(0.707106781186544,0.707106781186551,0.));
#37531=DIRECTION('',(0.,-0.707106781186579,-0.707106781186516));
#37532=DIRECTION('center_axis',(0.,-0.707106781186527,0.707106781186568));
#37533=DIRECTION('ref_axis',(1.,0.,0.));
#37534=DIRECTION('center_axis',(0.,0.,1.));
#37535=DIRECTION('ref_axis',(-0.707106781186544,0.707106781186551,0.));
#37536=DIRECTION('',(0.,0.,-1.));
#37537=DIRECTION('center_axis',(0.,0.,1.));
#37538=DIRECTION('ref_axis',(-0.707106781186553,-0.707106781186542,0.));
#37539=DIRECTION('',(0.,0.,1.));
#37540=DIRECTION('center_axis',(1.,0.,0.));
#37541=DIRECTION('ref_axis',(0.,1.,0.));
#37542=DIRECTION('center_axis',(-1.,0.,0.));
#37543=DIRECTION('ref_axis',(0.,-1.,0.));
#37544=DIRECTION('',(0.,0.,1.));
#37545=DIRECTION('center_axis',(0.,0.,1.));
#37546=DIRECTION('ref_axis',(-0.70710678118655,0.707106781186546,0.));
#37547=DIRECTION('',(0.,0.,1.));
#37548=DIRECTION('',(1.,0.,0.));
#37549=DIRECTION('',(0.,0.,1.));
#37550=DIRECTION('',(1.,0.,0.));
#37551=DIRECTION('',(0.,0.,1.));
#37552=DIRECTION('',(1.,0.,0.));
#37553=DIRECTION('',(0.,0.,1.));
#37554=DIRECTION('',(1.,0.,0.));
#37555=DIRECTION('',(0.,0.,1.));
#37556=DIRECTION('',(1.,0.,0.));
#37557=DIRECTION('',(0.,0.,1.));
#37558=DIRECTION('',(1.,0.,0.));
#37559=DIRECTION('',(0.,0.,1.));
#37560=DIRECTION('',(1.,0.,0.));
#37561=DIRECTION('',(0.,0.,1.));
#37562=DIRECTION('',(1.,0.,0.));
#37563=DIRECTION('',(0.,0.,1.));
#37564=DIRECTION('',(1.,0.,0.));
#37565=DIRECTION('',(0.,0.,1.));
#37566=DIRECTION('',(1.,0.,0.));
#37567=DIRECTION('',(0.,0.,1.));
#37568=DIRECTION('',(1.,0.,0.));
#37569=DIRECTION('',(0.,0.,1.));
#37570=DIRECTION('',(1.,0.,0.));
#37571=DIRECTION('',(0.,0.,1.));
#37572=DIRECTION('',(1.,0.,0.));
#37573=DIRECTION('',(0.,-1.22464679914735E-16,-1.));
#37574=DIRECTION('',(1.,0.,0.));
#37575=DIRECTION('',(0.,0.,1.));
#37576=DIRECTION('',(1.,0.,0.));
#37577=DIRECTION('',(0.,-1.,-2.22044604925031E-16));
#37578=DIRECTION('',(1.,0.,0.));
#37579=DIRECTION('',(0.,1.,-2.22044604925031E-16));
#37580=DIRECTION('',(1.,0.,0.));
#37581=DIRECTION('',(0.,-1.,-2.22044604925031E-16));
#37582=DIRECTION('',(1.,0.,0.));
#37583=DIRECTION('',(0.,0.,1.));
#37584=DIRECTION('',(1.,0.,0.));
#37585=DIRECTION('',(0.,0.,1.));
#37586=DIRECTION('',(1.,0.,0.));
#37587=DIRECTION('',(0.,0.,1.));
#37588=DIRECTION('',(-1.,1.22464679914735E-16,0.));
#37589=DIRECTION('',(0.,0.,1.));
#37590=DIRECTION('',(1.,0.,0.));
#37591=DIRECTION('',(0.,-1.22464679914735E-16,-1.));
#37592=DIRECTION('',(1.,0.,0.));
#37593=DIRECTION('',(0.,0.,1.));
#37594=DIRECTION('',(1.,0.,0.));
#37595=DIRECTION('',(0.,0.,1.));
#37596=DIRECTION('',(1.,0.,0.));
#37597=DIRECTION('',(0.,0.,1.));
#37598=DIRECTION('',(-1.,1.22464679914735E-16,0.));
#37599=DIRECTION('',(0.,-1.,-2.22044604925031E-16));
#37600=DIRECTION('',(1.,0.,0.));
#37601=DIRECTION('',(0.,-1.,-2.22044604925031E-16));
#37602=DIRECTION('',(1.,0.,0.));
#37603=DIRECTION('',(0.,-1.,-2.22044604925031E-16));
#37604=DIRECTION('',(1.,0.,0.));
#37605=DIRECTION('',(0.,-1.,-2.22044604925031E-16));
#37606=DIRECTION('',(1.,0.,0.));
#37607=DIRECTION('',(0.,-1.,-2.22044604925031E-16));
#37608=DIRECTION('',(1.,0.,0.));
#37609=DIRECTION('',(0.,-1.,-2.22044604925031E-16));
#37610=DIRECTION('',(1.,0.,0.));
#37611=DIRECTION('',(0.,-1.,-2.22044604925031E-16));
#37612=DIRECTION('',(1.,0.,0.));
#37613=DIRECTION('',(0.,-1.,-2.22044604925031E-16));
#37614=DIRECTION('',(1.,0.,0.));
#37615=DIRECTION('',(0.,-1.,-2.22044604925031E-16));
#37616=DIRECTION('',(1.,0.,0.));
#37617=DIRECTION('',(0.,1.,-2.22044604925031E-16));
#37618=DIRECTION('',(1.,0.,0.));
#37619=DIRECTION('',(0.,1.,-2.22044604925031E-16));
#37620=DIRECTION('',(1.,0.,0.));
#37621=DIRECTION('',(0.,1.,-2.22044604925031E-16));
#37622=DIRECTION('',(1.,0.,0.));
#37623=DIRECTION('',(0.,1.,-2.22044604925031E-16));
#37624=DIRECTION('',(1.,0.,0.));
#37625=DIRECTION('',(0.,1.,-2.22044604925031E-16));
#37626=DIRECTION('',(1.,0.,0.));
#37627=DIRECTION('',(0.,1.,-2.22044604925031E-16));
#37628=DIRECTION('',(1.,0.,0.));
#37629=DIRECTION('',(0.,1.,-2.22044604925031E-16));
#37630=DIRECTION('',(1.,0.,0.));
#37631=DIRECTION('',(0.,1.,-2.22044604925031E-16));
#37632=DIRECTION('',(1.,0.,0.));
#37633=DIRECTION('',(0.,1.,-2.22044604925031E-16));
#37634=DIRECTION('',(1.,0.,0.));
#37635=DIRECTION('',(0.,-1.,-2.22044604925031E-16));
#37636=DIRECTION('',(1.,0.,0.));
#37637=DIRECTION('',(0.,-1.,-2.22044604925031E-16));
#37638=DIRECTION('',(1.,0.,0.));
#37639=DIRECTION('',(0.,-1.,-2.22044604925031E-16));
#37640=DIRECTION('',(1.,0.,0.));
#37641=DIRECTION('',(0.,-1.,-2.22044604925031E-16));
#37642=DIRECTION('',(1.,0.,0.));
#37643=DIRECTION('',(0.,-1.,-2.22044604925031E-16));
#37644=DIRECTION('',(1.,0.,0.));
#37645=DIRECTION('',(0.,-1.,-2.22044604925031E-16));
#37646=DIRECTION('',(1.,0.,0.));
#37647=DIRECTION('',(0.,-1.,-2.22044604925031E-16));
#37648=DIRECTION('',(1.,0.,0.));
#37649=DIRECTION('',(0.,-1.,-2.22044604925031E-16));
#37650=DIRECTION('',(1.,0.,0.));
#37651=DIRECTION('',(0.,-1.,-2.22044604925031E-16));
#37652=DIRECTION('',(1.,0.,0.));
#37653=DIRECTION('',(0.,1.,-2.22044604925031E-16));
#37654=DIRECTION('',(1.,0.,0.));
#37655=DIRECTION('',(0.,1.,-2.22044604925031E-16));
#37656=DIRECTION('',(1.,0.,0.));
#37657=DIRECTION('',(0.,1.,-2.22044604925031E-16));
#37658=DIRECTION('',(1.,0.,0.));
#37659=DIRECTION('',(0.,1.,-2.22044604925031E-16));
#37660=DIRECTION('',(1.,0.,0.));
#37661=DIRECTION('',(0.,1.,-2.22044604925031E-16));
#37662=DIRECTION('',(1.,0.,0.));
#37663=DIRECTION('',(0.,1.,-2.22044604925031E-16));
#37664=DIRECTION('',(1.,0.,0.));
#37665=DIRECTION('',(0.,1.,-2.22044604925031E-16));
#37666=DIRECTION('',(1.,0.,0.));
#37667=DIRECTION('',(0.,1.,-2.22044604925031E-16));
#37668=DIRECTION('',(1.,0.,0.));
#37669=DIRECTION('',(0.,1.,-2.22044604925031E-16));
#37670=DIRECTION('',(1.,0.,0.));
#37671=DIRECTION('',(0.,1.,-2.22044604925031E-16));
#37672=DIRECTION('',(1.,0.,0.));
#37673=DIRECTION('',(0.,0.,1.));
#37674=DIRECTION('',(1.,0.,0.));
#37675=DIRECTION('',(0.,0.,1.));
#37676=DIRECTION('',(1.,0.,0.));
#37677=CARTESIAN_POINT('',(0.,0.,0.));
#37678=CARTESIAN_POINT('',(0.,0.,0.));
#37679=CARTESIAN_POINT('Origin',(-25.75,8.95,134.));
#37680=CARTESIAN_POINT('',(-25.8,8.9,135.));
#37681=CARTESIAN_POINT('',(-25.7,9.,134.9));
#37682=CARTESIAN_POINT('',(-19.150000000001,15.549999999999,128.349999999999));
#37683=CARTESIAN_POINT('',(-25.7,9.,134.15));
#37684=CARTESIAN_POINT('',(-25.7,9.,134.));
#37685=CARTESIAN_POINT('',(-25.75,8.95,134.1));
#37686=CARTESIAN_POINT('',(-19.3333333333335,15.3666666666665,140.516666666667));
#37687=CARTESIAN_POINT('',(-25.8,8.9,134.15));
#37688=CARTESIAN_POINT('',(-26.4666666666666,8.23333333333335,134.816666666667));
#37689=CARTESIAN_POINT('',(-25.8,8.9,134.));
#37690=CARTESIAN_POINT('Origin',(12.9,8.925,134.075));
#37691=CARTESIAN_POINT('',(25.7,9.,134.15));
#37692=CARTESIAN_POINT('',(12.9,9.,134.15));
#37693=CARTESIAN_POINT('',(25.75,8.95,134.1));
#37694=CARTESIAN_POINT('',(23.6333333333334,11.0666666666666,136.216666666667));
#37695=CARTESIAN_POINT('',(25.65,8.85,134.));
#37696=CARTESIAN_POINT('',(25.65,8.85,134.));
#37697=CARTESIAN_POINT('',(-25.65,8.85,134.));
#37698=CARTESIAN_POINT('',(12.9,8.85,134.));
#37699=CARTESIAN_POINT('',(-25.8,9.,134.15));
#37700=CARTESIAN_POINT('Origin',(25.8,9.,134.));
#37701=CARTESIAN_POINT('',(25.7,9.,134.9));
#37702=CARTESIAN_POINT('',(12.9,9.,134.9));
#37703=CARTESIAN_POINT('',(25.7,9.,134.));
#37704=CARTESIAN_POINT('Origin',(12.9,8.95,134.95));
#37705=CARTESIAN_POINT('',(25.8,8.9,135.));
#37706=CARTESIAN_POINT('',(12.9,8.9,135.));
#37707=CARTESIAN_POINT('',(23.4500000000003,11.2499999999997,132.65));
#37708=CARTESIAN_POINT('Origin',(25.75,8.95,134.));
#37709=CARTESIAN_POINT('',(25.8,8.9,134.15));
#37710=CARTESIAN_POINT('',(25.8,8.9,134.));
#37711=CARTESIAN_POINT('',(27.9666666666666,6.7333333333334,136.316666666667));
#37712=CARTESIAN_POINT('Origin',(25.725,-4.5,134.075));
#37713=CARTESIAN_POINT('',(25.8,-8.9,134.15));
#37714=CARTESIAN_POINT('',(25.8,-4.5,134.15));
#37715=CARTESIAN_POINT('',(25.75,-8.95,134.1));
#37716=CARTESIAN_POINT('',(26.4666666666666,-8.23333333333335,134.816666666667));
#37717=CARTESIAN_POINT('',(25.65,-8.85,134.));
#37718=CARTESIAN_POINT('',(25.65,-8.85,134.));
#37719=CARTESIAN_POINT('',(25.65,-4.5,134.));
#37720=CARTESIAN_POINT('Origin',(25.8,-9.,134.));
#37721=CARTESIAN_POINT('',(25.8,8.2,135.));
#37722=CARTESIAN_POINT('',(25.8,-9.,135.));
#37723=CARTESIAN_POINT('',(25.8,4.8,135.));
#37724=CARTESIAN_POINT('',(25.8,-2.5,135.));
#37725=CARTESIAN_POINT('',(25.8,-4.8,135.));
#37726=CARTESIAN_POINT('',(25.8,-9.,135.));
#37727=CARTESIAN_POINT('',(25.8,-8.2,135.));
#37728=CARTESIAN_POINT('',(25.8,-9.,135.));
#37729=CARTESIAN_POINT('',(25.8,-8.9,135.));
#37730=CARTESIAN_POINT('',(25.8,-9.,135.));
#37731=CARTESIAN_POINT('',(25.8,-8.9,134.));
#37732=CARTESIAN_POINT('Origin',(-25.75,-8.95,134.));
#37733=CARTESIAN_POINT('',(-25.7,-9.,134.9));
#37734=CARTESIAN_POINT('',(-25.8,-8.9,135.));
#37735=CARTESIAN_POINT('',(-23.4500000000003,-11.2499999999997,132.65));
#37736=CARTESIAN_POINT('',(-25.8,-8.9,134.15));
#37737=CARTESIAN_POINT('',(-25.8,-8.9,134.));
#37738=CARTESIAN_POINT('',(-25.75,-8.95,134.1));
#37739=CARTESIAN_POINT('',(-27.9666666666666,-6.7333333333334,136.316666666667));
#37740=CARTESIAN_POINT('',(-25.7,-9.,134.15));
#37741=CARTESIAN_POINT('',(-23.6333333333334,-11.0666666666666,136.216666666667));
#37742=CARTESIAN_POINT('',(-25.7,-9.,134.));
#37743=CARTESIAN_POINT('Origin',(-25.8,-9.,134.));
#37744=CARTESIAN_POINT('',(25.7,-9.,134.15));
#37745=CARTESIAN_POINT('',(-12.9,-9.,134.15));
#37746=CARTESIAN_POINT('',(25.7,-9.,134.9));
#37747=CARTESIAN_POINT('',(25.7,-9.,134.));
#37748=CARTESIAN_POINT('',(-12.9,-9.,134.9));
#37749=CARTESIAN_POINT('Origin',(-12.9,-8.925,134.075));
#37750=CARTESIAN_POINT('',(-25.65,-8.85,134.));
#37751=CARTESIAN_POINT('',(-25.65,-8.85,134.));
#37752=CARTESIAN_POINT('',(-12.9,-8.85,134.));
#37753=CARTESIAN_POINT('',(19.3333333333335,-15.3666666666665,140.516666666667));
#37754=CARTESIAN_POINT('Origin',(-25.725,4.5,134.075));
#37755=CARTESIAN_POINT('',(-25.65,4.5,134.));
#37756=CARTESIAN_POINT('',(-25.8,4.5,134.15));
#37757=CARTESIAN_POINT('Origin',(-12.9,-8.95,134.95));
#37758=CARTESIAN_POINT('',(19.150000000001,-15.549999999999,128.349999999999));
#37759=CARTESIAN_POINT('',(-12.9,-8.9,135.));
#37760=CARTESIAN_POINT('Origin',(0.,0.,135.));
#37761=CARTESIAN_POINT('',(-25.8,-8.2,135.));
#37762=CARTESIAN_POINT('',(-38.,-8.2,135.));
#37763=CARTESIAN_POINT('',(-25.8,9.,135.));
#37764=CARTESIAN_POINT('Origin',(25.75,-8.95,134.));
#37765=CARTESIAN_POINT('Origin',(30.,-4.55,142.5));
#37766=CARTESIAN_POINT('',(29.025,-4.6,142.5));
#37767=CARTESIAN_POINT('Origin',(30.,-4.6,142.5));
#37768=CARTESIAN_POINT('',(29.125,-4.5,142.5));
#37769=CARTESIAN_POINT('',(29.075,-4.55,142.5));
#37770=CARTESIAN_POINT('Origin',(30.,-4.5,142.5));
#37771=CARTESIAN_POINT('Origin',(-38.,-4.6,144.4));
#37772=CARTESIAN_POINT('',(-37.9,-4.6,136.));
#37773=CARTESIAN_POINT('',(-37.9,-4.6,144.));
#37774=CARTESIAN_POINT('',(-37.9,-4.6,142.2));
#37775=CARTESIAN_POINT('',(37.9,-4.6,136.));
#37776=CARTESIAN_POINT('',(-38.,-4.6,136.));
#37777=CARTESIAN_POINT('',(37.9,-4.6,144.));
#37778=CARTESIAN_POINT('',(37.9,-4.6,142.2));
#37779=CARTESIAN_POINT('',(-38.,-4.6,144.));
#37780=CARTESIAN_POINT('',(-30.975,-4.6,137.5));
#37781=CARTESIAN_POINT('Origin',(-30.,-4.6,137.5));
#37782=CARTESIAN_POINT('',(29.025,-4.6,137.5));
#37783=CARTESIAN_POINT('Origin',(30.,-4.6,137.5));
#37784=CARTESIAN_POINT('',(-30.975,-4.6,142.5));
#37785=CARTESIAN_POINT('Origin',(-30.,-4.6,142.5));
#37786=CARTESIAN_POINT('Origin',(30.,0.,142.5));
#37787=CARTESIAN_POINT('',(29.125,-4.1,142.5));
#37788=CARTESIAN_POINT('',(29.125,0.,142.5));
#37789=CARTESIAN_POINT('Origin',(30.,-4.1,142.5));
#37790=CARTESIAN_POINT('Origin',(-30.,-4.55,137.5));
#37791=CARTESIAN_POINT('',(-30.875,-4.5,137.5));
#37792=CARTESIAN_POINT('',(-30.925,-4.55,137.5));
#37793=CARTESIAN_POINT('Origin',(-30.,-4.5,137.5));
#37794=CARTESIAN_POINT('Origin',(-30.,0.,137.5));
#37795=CARTESIAN_POINT('',(-30.875,-4.1,137.5));
#37796=CARTESIAN_POINT('',(-30.875,0.,137.5));
#37797=CARTESIAN_POINT('Origin',(-30.,-4.1,137.5));
#37798=CARTESIAN_POINT('Origin',(-30.,-4.55,142.5));
#37799=CARTESIAN_POINT('',(-30.875,-4.5,142.5));
#37800=CARTESIAN_POINT('',(-30.925,-4.55,142.5));
#37801=CARTESIAN_POINT('Origin',(-30.,-4.5,142.5));
#37802=CARTESIAN_POINT('Origin',(-30.,0.,142.5));
#37803=CARTESIAN_POINT('',(-30.875,-4.1,142.5));
#37804=CARTESIAN_POINT('',(-30.875,0.,142.5));
#37805=CARTESIAN_POINT('Origin',(-30.,-4.1,142.5));
#37806=CARTESIAN_POINT('Origin',(30.,-4.55,137.5));
#37807=CARTESIAN_POINT('',(29.125,-4.5,137.5));
#37808=CARTESIAN_POINT('',(29.075,-4.55,137.5));
#37809=CARTESIAN_POINT('Origin',(30.,-4.5,137.5));
#37810=CARTESIAN_POINT('Origin',(30.,0.,137.5));
#37811=CARTESIAN_POINT('',(29.125,-4.1,137.5));
#37812=CARTESIAN_POINT('',(29.125,0.,137.5));
#37813=CARTESIAN_POINT('Origin',(30.,-4.1,137.5));
#37814=CARTESIAN_POINT('Origin',(30.,-4.05,137.5));
#37815=CARTESIAN_POINT('',(29.025,-4.,137.5));
#37816=CARTESIAN_POINT('Origin',(30.,-4.,137.5));
#37817=CARTESIAN_POINT('',(29.075,-4.05,137.5));
#37818=CARTESIAN_POINT('Origin',(-38.,-4.,135.));
#37819=CARTESIAN_POINT('',(37.9,-4.,135.8));
#37820=CARTESIAN_POINT('',(37.9,-4.,144.2));
#37821=CARTESIAN_POINT('',(37.9,-4.,137.5));
#37822=CARTESIAN_POINT('',(-37.9,-4.,135.8));
#37823=CARTESIAN_POINT('',(-38.,-4.,135.8));
#37824=CARTESIAN_POINT('',(-37.9,-4.,144.2));
#37825=CARTESIAN_POINT('',(-37.9,-4.,137.5));
#37826=CARTESIAN_POINT('',(-38.,-4.,144.2));
#37827=CARTESIAN_POINT('',(-30.975,-4.,142.5));
#37828=CARTESIAN_POINT('Origin',(-30.,-4.,142.5));
#37829=CARTESIAN_POINT('',(29.025,-4.,142.5));
#37830=CARTESIAN_POINT('Origin',(30.,-4.,142.5));
#37831=CARTESIAN_POINT('',(-30.975,-4.,137.5));
#37832=CARTESIAN_POINT('Origin',(-30.,-4.,137.5));
#37833=CARTESIAN_POINT('Origin',(-30.,-4.05,142.5));
#37834=CARTESIAN_POINT('',(-30.925,-4.05,142.5));
#37835=CARTESIAN_POINT('Origin',(-30.,-4.05,137.5));
#37836=CARTESIAN_POINT('',(-30.925,-4.05,137.5));
#37837=CARTESIAN_POINT('Origin',(30.,-4.05,142.5));
#37838=CARTESIAN_POINT('',(29.075,-4.05,142.5));
#37839=CARTESIAN_POINT('Origin',(30.,4.55,142.5));
#37840=CARTESIAN_POINT('',(29.025,4.6,142.5));
#37841=CARTESIAN_POINT('Origin',(30.,4.6,142.5));
#37842=CARTESIAN_POINT('',(29.125,4.5,142.5));
#37843=CARTESIAN_POINT('',(29.075,4.55,142.5));
#37844=CARTESIAN_POINT('Origin',(30.,4.5,142.5));
#37845=CARTESIAN_POINT('Origin',(-38.,4.6,135.6));
#37846=CARTESIAN_POINT('',(37.9,4.6,136.));
#37847=CARTESIAN_POINT('',(37.9,4.6,144.));
#37848=CARTESIAN_POINT('',(37.9,4.6,137.8));
#37849=CARTESIAN_POINT('',(-37.9,4.6,136.));
#37850=CARTESIAN_POINT('',(-38.,4.6,136.));
#37851=CARTESIAN_POINT('',(-37.9,4.6,144.));
#37852=CARTESIAN_POINT('',(-37.9,4.6,137.8));
#37853=CARTESIAN_POINT('',(-38.,4.6,144.));
#37854=CARTESIAN_POINT('',(-30.975,4.6,137.5));
#37855=CARTESIAN_POINT('Origin',(-30.,4.6,137.5));
#37856=CARTESIAN_POINT('',(29.025,4.6,137.5));
#37857=CARTESIAN_POINT('Origin',(30.,4.6,137.5));
#37858=CARTESIAN_POINT('',(-30.975,4.6,142.5));
#37859=CARTESIAN_POINT('Origin',(-30.,4.6,142.5));
#37860=CARTESIAN_POINT('Origin',(30.,0.,142.5));
#37861=CARTESIAN_POINT('',(29.125,4.1,142.5));
#37862=CARTESIAN_POINT('Origin',(30.,4.1,142.5));
#37863=CARTESIAN_POINT('',(29.125,0.,142.5));
#37864=CARTESIAN_POINT('Origin',(-30.,4.55,137.5));
#37865=CARTESIAN_POINT('',(-30.875,4.5,137.5));
#37866=CARTESIAN_POINT('',(-30.925,4.55,137.5));
#37867=CARTESIAN_POINT('Origin',(-30.,4.5,137.5));
#37868=CARTESIAN_POINT('Origin',(-30.,0.,137.5));
#37869=CARTESIAN_POINT('',(-30.875,4.1,137.5));
#37870=CARTESIAN_POINT('Origin',(-30.,4.1,137.5));
#37871=CARTESIAN_POINT('',(-30.875,0.,137.5));
#37872=CARTESIAN_POINT('Origin',(-30.,4.55,142.5));
#37873=CARTESIAN_POINT('',(-30.875,4.5,142.5));
#37874=CARTESIAN_POINT('',(-30.925,4.55,142.5));
#37875=CARTESIAN_POINT('Origin',(-30.,4.5,142.5));
#37876=CARTESIAN_POINT('Origin',(-30.,0.,142.5));
#37877=CARTESIAN_POINT('',(-30.875,4.1,142.5));
#37878=CARTESIAN_POINT('Origin',(-30.,4.1,142.5));
#37879=CARTESIAN_POINT('',(-30.875,0.,142.5));
#37880=CARTESIAN_POINT('Origin',(30.,4.55,137.5));
#37881=CARTESIAN_POINT('',(29.125,4.5,137.5));
#37882=CARTESIAN_POINT('',(29.075,4.55,137.5));
#37883=CARTESIAN_POINT('Origin',(30.,4.5,137.5));
#37884=CARTESIAN_POINT('Origin',(30.,0.,137.5));
#37885=CARTESIAN_POINT('',(29.125,4.1,137.5));
#37886=CARTESIAN_POINT('Origin',(30.,4.1,137.5));
#37887=CARTESIAN_POINT('',(29.125,0.,137.5));
#37888=CARTESIAN_POINT('Origin',(30.,-8.95,142.5));
#37889=CARTESIAN_POINT('',(30.8485281374239,-9.,144.2));
#37890=CARTESIAN_POINT('',(30.80386876177,-8.9,144.110526315789));
#37891=CARTESIAN_POINT('',(30.8485281374239,-9.,144.2));
#37892=CARTESIAN_POINT('',(28.2,-8.9,142.5));
#37893=CARTESIAN_POINT('Origin',(30.,-8.9,142.5));
#37894=CARTESIAN_POINT('',(29.19613123823,-8.9,144.110526315789));
#37895=CARTESIAN_POINT('Origin',(30.,-8.9,142.5));
#37896=CARTESIAN_POINT('',(29.1514718625761,-9.,144.2));
#37897=CARTESIAN_POINT('',(29.19613123823,-8.9,144.110526315789));
#37898=CARTESIAN_POINT('Origin',(30.,-9.,142.5));
#37899=CARTESIAN_POINT('Ctrl Pts',(29.37557606376,-8.99442305443429,144.29429745799));
#37900=CARTESIAN_POINT('Ctrl Pts',(29.4528789423666,-8.99125209441901,144.321011685441));
#37901=CARTESIAN_POINT('Ctrl Pts',(29.6108779014912,-8.98340236313526,144.364462672992));
#37902=CARTESIAN_POINT('Ctrl Pts',(29.8538300241761,-8.97543935789693,144.397225194892));
#37903=CARTESIAN_POINT('Ctrl Pts',(30.1578937093748,-8.97381382255402,144.402534138038));
#37904=CARTESIAN_POINT('Ctrl Pts',(30.4034174830284,-8.98452879794544,144.36323637123));
#37905=CARTESIAN_POINT('Ctrl Pts',(30.5816912715748,-8.99263170993257,144.308616992978));
#37906=CARTESIAN_POINT('Ctrl Pts',(30.6031336007836,-8.99354972599348,144.301654944207));
#37907=CARTESIAN_POINT('Ctrl Pts',(30.62442393624,-8.99442305443429,144.29429745799));
#37908=CARTESIAN_POINT('Ctrl Pts',(29.3865147164033,-8.96294870295619,144.262864971993));
#37909=CARTESIAN_POINT('Ctrl Pts',(29.4621247530599,-8.96082929478778,144.289053145881));
#37910=CARTESIAN_POINT('Ctrl Pts',(29.6170733795065,-8.95481417908684,144.331935721362));
#37911=CARTESIAN_POINT('Ctrl Pts',(29.8560577408031,-8.94828380943131,144.364473342857));
#37912=CARTESIAN_POINT('Ctrl Pts',(30.1554889558999,-8.9469018651377,144.369780678576));
#37913=CARTESIAN_POINT('Ctrl Pts',(30.3970550842887,-8.95587368877562,144.3306496463));
#37914=CARTESIAN_POINT('Ctrl Pts',(30.5716687838969,-8.96172308279366,144.276909344891));
#37915=CARTESIAN_POINT('Ctrl Pts',(30.5926595579726,-8.9623708163431,144.270081805573));
#37916=CARTESIAN_POINT('Ctrl Pts',(30.6134852835967,-8.96294870295619,144.262864971993));
#37917=CARTESIAN_POINT('Ctrl Pts',(29.3974533690466,-8.9314743514781,144.231432485996));
#37918=CARTESIAN_POINT('Ctrl Pts',(29.4713946846489,-8.93042279963123,144.257101347462));
#37919=CARTESIAN_POINT('Ctrl Pts',(29.6232594585157,-8.92620755420488,144.299394395606));
#37920=CARTESIAN_POINT('Ctrl Pts',(29.8582882281875,-8.92111994873181,144.331713130336));
#37921=CARTESIAN_POINT('Ctrl Pts',(30.1530997401632,-8.91998748202325,144.337018634271));
#37922=CARTESIAN_POINT('Ctrl Pts',(30.3906863776209,-8.92714570081842,144.297997431227));
#37923=CARTESIAN_POINT('Ctrl Pts',(30.5616480648658,-8.93082793618361,144.245213046289));
#37924=CARTESIAN_POINT('Ctrl Pts',(30.5821837421954,-8.93117890965038,144.238497833085));
#37925=CARTESIAN_POINT('Ctrl Pts',(30.6025466309533,-8.9314743514781,144.231432485997));
#37926=CARTESIAN_POINT('Ctrl Pts',(29.40839202169,-8.9,144.2));
#37927=CARTESIAN_POINT('Ctrl Pts',(29.4806404953422,-8.9,144.225142807902));
#37928=CARTESIAN_POINT('Ctrl Pts',(29.6294549365309,-8.89761937015647,144.266867443976));
#37929=CARTESIAN_POINT('Ctrl Pts',(29.8605159448146,-8.89396440026619,144.298961278301));
#37930=CARTESIAN_POINT('Ctrl Pts',(30.1506949866883,-8.89307552460693,144.304265174808));
#37931=CARTESIAN_POINT('Ctrl Pts',(30.3843239788812,-8.8984905916486,144.265410706296));
#37932=CARTESIAN_POINT('Ctrl Pts',(30.5516255771879,-8.8999193090447,144.213505398201));
#37933=CARTESIAN_POINT('Ctrl Pts',(30.5717096993844,-8.9,144.206924694451));
#37934=CARTESIAN_POINT('Ctrl Pts',(30.59160797831,-8.9,144.2));
#37935=CARTESIAN_POINT('',(30.59160797831,-8.9,144.2));
#37936=CARTESIAN_POINT('',(30.62442393624,-8.99442305443429,144.29429745799));
#37937=CARTESIAN_POINT('',(30.59160797831,-8.9,144.2));
#37938=CARTESIAN_POINT('',(29.37557606376,-8.99442305443429,144.29429745799));
#37939=CARTESIAN_POINT('Ctrl Pts',(30.62442393624,-8.99442305443429,144.29429745799));
#37940=CARTESIAN_POINT('Ctrl Pts',(30.6031336007836,-8.99354972599348,144.301654944207));
#37941=CARTESIAN_POINT('Ctrl Pts',(30.5816912715748,-8.99263170993257,144.308616992978));
#37942=CARTESIAN_POINT('Ctrl Pts',(30.4034174830284,-8.98452879794544,144.36323637123));
#37943=CARTESIAN_POINT('Ctrl Pts',(30.1578937093748,-8.97381382255402,144.402534138038));
#37944=CARTESIAN_POINT('Ctrl Pts',(29.8538300241761,-8.97543935789693,144.397225194892));
#37945=CARTESIAN_POINT('Ctrl Pts',(29.6108779014912,-8.98340236313526,144.364462672992));
#37946=CARTESIAN_POINT('Ctrl Pts',(29.4528789423666,-8.99125209441901,144.321011685441));
#37947=CARTESIAN_POINT('Ctrl Pts',(29.37557606376,-8.99442305443429,144.29429745799));
#37948=CARTESIAN_POINT('',(29.40839202169,-8.9,144.2));
#37949=CARTESIAN_POINT('',(29.37557606376,-8.99442305443429,144.29429745799));
#37950=CARTESIAN_POINT('Ctrl Pts',(29.40839202169,-8.9,144.2));
#37951=CARTESIAN_POINT('Ctrl Pts',(29.4806404953422,-8.9,144.225142807902));
#37952=CARTESIAN_POINT('Ctrl Pts',(29.6294549365309,-8.89761937015647,144.266867443976));
#37953=CARTESIAN_POINT('Ctrl Pts',(29.8605159448146,-8.89396440026619,144.298961278301));
#37954=CARTESIAN_POINT('Ctrl Pts',(30.1506949866883,-8.89307552460693,144.304265174808));
#37955=CARTESIAN_POINT('Ctrl Pts',(30.3843239788812,-8.8984905916486,144.265410706296));
#37956=CARTESIAN_POINT('Ctrl Pts',(30.5516255771879,-8.8999193090447,144.213505398201));
#37957=CARTESIAN_POINT('Ctrl Pts',(30.5717096993844,-8.9,144.206924694451));
#37958=CARTESIAN_POINT('Ctrl Pts',(30.59160797831,-8.9,144.2));
#37959=CARTESIAN_POINT('Ctrl Pts',(29.1514718625761,-9.,144.2));
#37960=CARTESIAN_POINT('Ctrl Pts',(29.2240383852933,-9.,144.236220433153));
#37961=CARTESIAN_POINT('Ctrl Pts',(29.2989266202372,-8.99756721057679,144.267809043778));
#37962=CARTESIAN_POINT('Ctrl Pts',(29.37557606376,-8.99442305443429,144.29429745799));
#37963=CARTESIAN_POINT('Ctrl Pts',(29.1663583211274,-8.96666666666667,144.170175438596));
#37964=CARTESIAN_POINT('Ctrl Pts',(29.2376517469549,-8.96666666666667,144.205760425554));
#37965=CARTESIAN_POINT('Ctrl Pts',(29.3112262464824,-8.96504480705119,144.236788199029));
#37966=CARTESIAN_POINT('Ctrl Pts',(29.3865147164034,-8.96294870295619,144.262864971993));
#37967=CARTESIAN_POINT('Ctrl Pts',(29.1812447796787,-8.93333333333333,144.140350877193));
#37968=CARTESIAN_POINT('Ctrl Pts',(29.2512651086164,-8.93333333333333,144.175300417955));
#37969=CARTESIAN_POINT('Ctrl Pts',(29.3235258727276,-8.9325224035256,144.20576735428));
#37970=CARTESIAN_POINT('Ctrl Pts',(29.3974533690467,-8.9314743514781,144.231432485997));
#37971=CARTESIAN_POINT('Ctrl Pts',(29.19613123823,-8.9,144.110526315789));
#37972=CARTESIAN_POINT('Ctrl Pts',(29.2648784702779,-8.9,144.144840410356));
#37973=CARTESIAN_POINT('Ctrl Pts',(29.3358254989728,-8.9,144.174746509531));
#37974=CARTESIAN_POINT('Ctrl Pts',(29.40839202169,-8.9,144.2));
#37975=CARTESIAN_POINT('Ctrl Pts',(29.37557606376,-8.99442305443429,144.29429745799));
#37976=CARTESIAN_POINT('Ctrl Pts',(29.2989266202372,-8.99756721057679,144.267809043778));
#37977=CARTESIAN_POINT('Ctrl Pts',(29.2240383852933,-9.,144.236220433153));
#37978=CARTESIAN_POINT('Ctrl Pts',(29.1514718625761,-9.,144.2));
#37979=CARTESIAN_POINT('Ctrl Pts',(29.19613123823,-8.9,144.110526315789));
#37980=CARTESIAN_POINT('Ctrl Pts',(29.2648784702779,-8.9,144.144840410356));
#37981=CARTESIAN_POINT('Ctrl Pts',(29.3358254989728,-8.9,144.174746509531));
#37982=CARTESIAN_POINT('Ctrl Pts',(29.40839202169,-8.9,144.2));
#37983=CARTESIAN_POINT('Ctrl Pts',(30.62442393624,-8.99442305443429,144.29429745799));
#37984=CARTESIAN_POINT('Ctrl Pts',(30.7010733797633,-8.99756721057681,144.267809043778));
#37985=CARTESIAN_POINT('Ctrl Pts',(30.7759616147076,-9.00000000000003,144.236220433153));
#37986=CARTESIAN_POINT('Ctrl Pts',(30.8485281374252,-9.,144.199999999999));
#37987=CARTESIAN_POINT('Ctrl Pts',(30.6134852835966,-8.96294870295619,144.262864971993));
#37988=CARTESIAN_POINT('Ctrl Pts',(30.688773753518,-8.96504480705121,144.236788199029));
#37989=CARTESIAN_POINT('Ctrl Pts',(30.762348253046,-8.96666666666669,144.205760425554));
#37990=CARTESIAN_POINT('Ctrl Pts',(30.8336416788739,-8.96666666666667,144.170175438596));
#37991=CARTESIAN_POINT('Ctrl Pts',(30.6025466309533,-8.9314743514781,144.231432485997));
#37992=CARTESIAN_POINT('Ctrl Pts',(30.6764741272728,-8.9325224035256,144.20576735428));
#37993=CARTESIAN_POINT('Ctrl Pts',(30.7487348913845,-8.93333333333334,144.175300417955));
#37994=CARTESIAN_POINT('Ctrl Pts',(30.8187552203225,-8.93333333333333,144.140350877192));
#37995=CARTESIAN_POINT('Ctrl Pts',(30.59160797831,-8.9,144.2));
#37996=CARTESIAN_POINT('Ctrl Pts',(30.6641745010276,-8.9,144.174746509531));
#37997=CARTESIAN_POINT('Ctrl Pts',(30.7351215297229,-8.9,144.144840410355));
#37998=CARTESIAN_POINT('Ctrl Pts',(30.8038687617712,-8.9,144.110526315789));
#37999=CARTESIAN_POINT('Ctrl Pts',(30.8485281374252,-9.,144.199999999999));
#38000=CARTESIAN_POINT('Ctrl Pts',(30.7759616147076,-9.00000000000003,144.236220433153));
#38001=CARTESIAN_POINT('Ctrl Pts',(30.7010733797633,-8.99756721057681,144.267809043778));
#38002=CARTESIAN_POINT('Ctrl Pts',(30.62442393624,-8.99442305443429,144.29429745799));
#38003=CARTESIAN_POINT('Ctrl Pts',(30.59160797831,-8.9,144.2));
#38004=CARTESIAN_POINT('Ctrl Pts',(30.6641745010276,-8.9,144.174746509531));
#38005=CARTESIAN_POINT('Ctrl Pts',(30.7351215297229,-8.9,144.144840410355));
#38006=CARTESIAN_POINT('Ctrl Pts',(30.8038687617712,-8.9,144.110526315789));
#38007=CARTESIAN_POINT('Origin',(-38.,-8.2,144.2));
#38008=CARTESIAN_POINT('',(37.9,-9.,144.2));
#38009=CARTESIAN_POINT('',(-38.,-9.,144.2));
#38010=CARTESIAN_POINT('',(37.9,-8.2,145.));
#38011=CARTESIAN_POINT('Origin',(37.9,-8.2,144.2));
#38012=CARTESIAN_POINT('',(-37.9,-8.2,145.));
#38013=CARTESIAN_POINT('',(-38.,-8.2,145.));
#38014=CARTESIAN_POINT('',(-37.9,-9.,144.2));
#38015=CARTESIAN_POINT('Origin',(-37.9,-8.2,144.2));
#38016=CARTESIAN_POINT('',(-30.8485281374239,-9.,144.2));
#38017=CARTESIAN_POINT('',(-38.,-9.,144.2));
#38018=CARTESIAN_POINT('',(-30.62442393624,-8.99442305443429,144.29429745799));
#38019=CARTESIAN_POINT('Ctrl Pts',(-30.62442393624,-8.99442305443429,144.29429745799));
#38020=CARTESIAN_POINT('Ctrl Pts',(-30.7010733797628,-8.99756721057679,
144.267809043778));
#38021=CARTESIAN_POINT('Ctrl Pts',(-30.7759616147067,-9.,144.236220433153));
#38022=CARTESIAN_POINT('Ctrl Pts',(-30.8485281374239,-9.,144.2));
#38023=CARTESIAN_POINT('',(-29.37557606376,-8.99442305443429,144.29429745799));
#38024=CARTESIAN_POINT('Ctrl Pts',(-29.37557606376,-8.99442305443429,144.29429745799));
#38025=CARTESIAN_POINT('Ctrl Pts',(-29.3968663992163,-8.99354972599348,
144.301654944207));
#38026=CARTESIAN_POINT('Ctrl Pts',(-29.4183151210873,-8.99261764548661,
144.308633020031));
#38027=CARTESIAN_POINT('Ctrl Pts',(-29.5181405190621,-8.98818372075475,
144.339120021515));
#38028=CARTESIAN_POINT('Ctrl Pts',(-29.6784757526138,-8.98055560583611,
144.37677095198));
#38029=CARTESIAN_POINT('Ctrl Pts',(-29.917310908637,-8.97429943254969,144.401048817597));
#38030=CARTESIAN_POINT('Ctrl Pts',(-30.1466727558104,-8.97528496697549,
144.397455998416));
#38031=CARTESIAN_POINT('Ctrl Pts',(-30.3890975283267,-8.98340931878656,
144.364446023987));
#38032=CARTESIAN_POINT('Ctrl Pts',(-30.5471210576335,-8.99125209441902,
144.321011685441));
#38033=CARTESIAN_POINT('Ctrl Pts',(-30.62442393624,-8.99442305443429,144.29429745799));
#38034=CARTESIAN_POINT('',(-29.1514718625761,-9.,144.2));
#38035=CARTESIAN_POINT('Ctrl Pts',(-29.1514718625749,-9.,144.199999999999));
#38036=CARTESIAN_POINT('Ctrl Pts',(-29.2240383852925,-9.00000000000003,
144.236220433153));
#38037=CARTESIAN_POINT('Ctrl Pts',(-29.2989266202368,-8.99756721057681,
144.267809043778));
#38038=CARTESIAN_POINT('Ctrl Pts',(-29.37557606376,-8.99442305443429,144.29429745799));
#38039=CARTESIAN_POINT('',(-38.,-9.,144.2));
#38040=CARTESIAN_POINT('Origin',(30.,-9.1,142.5));
#38041=CARTESIAN_POINT('',(28.2,-8.5,142.5));
#38042=CARTESIAN_POINT('',(28.2,-9.1,142.5));
#38043=CARTESIAN_POINT('',(28.8951880620293,-8.5,143.921052631579));
#38044=CARTESIAN_POINT('Origin',(30.,-8.5,142.5));
#38045=CARTESIAN_POINT('',(29.0050125628934,-8.5,144.));
#38046=CARTESIAN_POINT('Ctrl Pts',(29.0050125628934,-8.5,144.));
#38047=CARTESIAN_POINT('Ctrl Pts',(28.9674326867105,-8.5,143.975072330207));
#38048=CARTESIAN_POINT('Ctrl Pts',(28.9307900499921,-8.5,143.948731762135));
#38049=CARTESIAN_POINT('Ctrl Pts',(28.8951880620293,-8.5,143.921052631579));
#38050=CARTESIAN_POINT('',(30.9949874371066,-8.5,144.));
#38051=CARTESIAN_POINT('Ctrl Pts',(30.9949874371066,-8.5,144.));
#38052=CARTESIAN_POINT('Ctrl Pts',(30.9864258065899,-8.5,144.005679143204));
#38053=CARTESIAN_POINT('Ctrl Pts',(30.9778381533882,-8.49988803935537,144.011270671384));
#38054=CARTESIAN_POINT('Ctrl Pts',(30.9692257738747,-8.49967189801602,144.016774735463));
#38055=CARTESIAN_POINT('Ctrl Pts',(30.957514713753,-8.49937799036647,144.024259127581));
#38056=CARTESIAN_POINT('Ctrl Pts',(30.9457617930679,-8.49889895697764,144.031575977005));
#38057=CARTESIAN_POINT('Ctrl Pts',(30.9339633564761,-8.49823699277985,144.038742874564));
#38058=CARTESIAN_POINT('Ctrl Pts',(30.7924312547142,-8.4902961793105,144.124715797054));
#38059=CARTESIAN_POINT('Ctrl Pts',(30.6455798173351,-8.45921759112122,144.187305181965));
#38060=CARTESIAN_POINT('Ctrl Pts',(30.4983882415935,-8.42943950721129,144.229760076013));
#38061=CARTESIAN_POINT('Ctrl Pts',(30.351196665852,-8.39966142330136,144.272214970061));
#38062=CARTESIAN_POINT('Ctrl Pts',(30.203664951748,-8.37118384367076,144.294535373247));
#38063=CARTESIAN_POINT('Ctrl Pts',(30.0579688188435,-8.36568430314537,144.299260363718));
#38064=CARTESIAN_POINT('Ctrl Pts',(30.0552225698401,-8.36558064145315,144.299349425796));
#38065=CARTESIAN_POINT('Ctrl Pts',(30.0524708101528,-8.36548152859756,144.29943128211));
#38066=CARTESIAN_POINT('Ctrl Pts',(30.0497199697297,-8.36539021135648,144.299506886864));
#38067=CARTESIAN_POINT('Ctrl Pts',(30.0414674484601,-8.36511625963326,144.299733701128));
#38068=CARTESIAN_POINT('Ctrl Pts',(30.033223200568,-8.36491246844071,144.299904251363));
#38069=CARTESIAN_POINT('Ctrl Pts',(30.0249742066664,-8.36477495772506,144.300018317497));
#38070=CARTESIAN_POINT('Ctrl Pts',(30.0019993209539,-8.36439196641558,144.300336011563));
#38071=CARTESIAN_POINT('Ctrl Pts',(29.9790119784398,-8.36454534261746,144.300212596464));
#38072=CARTESIAN_POINT('Ctrl Pts',(29.9560473210098,-8.36522412779964,144.299650865472));
#38073=CARTESIAN_POINT('Ctrl Pts',(29.9330826635799,-8.36590291298182,144.29908913448));
#38074=CARTESIAN_POINT('Ctrl Pts',(29.910140691234,-8.36710710714431,144.298089087593));
#38075=CARTESIAN_POINT('Ctrl Pts',(29.8871242708781,-8.36880464134516,144.296640642262));
#38076=CARTESIAN_POINT('Ctrl Pts',(29.8702147027416,-8.37005177577307,144.295576506978));
#38077=CARTESIAN_POINT('Ctrl Pts',(29.8533332047851,-8.37156072057906,144.294283011609));
#38078=CARTESIAN_POINT('Ctrl Pts',(29.8364165493979,-8.37330886307701,144.292734900211));
#38079=CARTESIAN_POINT('Ctrl Pts',(29.8194998940106,-8.37505700557497,144.291186788813));
#38080=CARTESIAN_POINT('Ctrl Pts',(29.8025480811926,-8.3770443457649,144.289384061385));
#38081=CARTESIAN_POINT('Ctrl Pts',(29.7856564998322,-8.37924514274765,144.287392801698));
#38082=CARTESIAN_POINT('Ctrl Pts',(29.5878470697021,-8.40501764963735,144.264074088329));
#38083=CARTESIAN_POINT('Ctrl Pts',(29.3817564945146,-8.46015770243706,144.20400082464));
#38084=CARTESIAN_POINT('Ctrl Pts',(29.1909226085664,-8.4860152481162,144.108025770902));
#38085=CARTESIAN_POINT('Ctrl Pts',(29.1273113132504,-8.49463443000924,144.076034086322));
#38086=CARTESIAN_POINT('Ctrl Pts',(29.0653952056276,-8.5,144.04005331396));
#38087=CARTESIAN_POINT('Ctrl Pts',(29.0050125628934,-8.5,144.));
#38088=CARTESIAN_POINT('',(31.1048119379707,-8.5,143.921052631579));
#38089=CARTESIAN_POINT('Ctrl Pts',(31.1048119379707,-8.5,143.921052631579));
#38090=CARTESIAN_POINT('Ctrl Pts',(31.0692099500079,-8.5,143.948731762135));
#38091=CARTESIAN_POINT('Ctrl Pts',(31.0325673132895,-8.5,143.975072330207));
#38092=CARTESIAN_POINT('Ctrl Pts',(30.9949874371066,-8.5,144.));
#38093=CARTESIAN_POINT('Origin',(30.,-8.5,142.5));
#38094=CARTESIAN_POINT('Origin',(30.,4.05,137.5));
#38095=CARTESIAN_POINT('',(29.025,4.,137.5));
#38096=CARTESIAN_POINT('Origin',(30.,4.,137.5));
#38097=CARTESIAN_POINT('',(29.075,4.05,137.5));
#38098=CARTESIAN_POINT('Origin',(-38.,4.,145.));
#38099=CARTESIAN_POINT('',(-37.9,4.,135.8));
#38100=CARTESIAN_POINT('',(-37.9,4.,144.2));
#38101=CARTESIAN_POINT('',(-37.9,4.,142.5));
#38102=CARTESIAN_POINT('',(37.9,4.,135.8));
#38103=CARTESIAN_POINT('',(-38.,4.,135.8));
#38104=CARTESIAN_POINT('',(37.9,4.,144.2));
#38105=CARTESIAN_POINT('',(37.9,4.,142.5));
#38106=CARTESIAN_POINT('',(-38.,4.,144.2));
#38107=CARTESIAN_POINT('',(-30.975,4.,142.5));
#38108=CARTESIAN_POINT('Origin',(-30.,4.,142.5));
#38109=CARTESIAN_POINT('',(29.025,4.,142.5));
#38110=CARTESIAN_POINT('Origin',(30.,4.,142.5));
#38111=CARTESIAN_POINT('',(-30.975,4.,137.5));
#38112=CARTESIAN_POINT('Origin',(-30.,4.,137.5));
#38113=CARTESIAN_POINT('Origin',(-30.,4.05,142.5));
#38114=CARTESIAN_POINT('',(-30.925,4.05,142.5));
#38115=CARTESIAN_POINT('Origin',(-30.,4.05,137.5));
#38116=CARTESIAN_POINT('',(-30.925,4.05,137.5));
#38117=CARTESIAN_POINT('Origin',(30.,4.05,142.5));
#38118=CARTESIAN_POINT('',(29.075,4.05,142.5));
#38119=CARTESIAN_POINT('Origin',(37.95,-8.2,135.8));
#38120=CARTESIAN_POINT('',(38.,-8.90000000000001,135.8));
#38121=CARTESIAN_POINT('',(37.9,-9.,135.8));
#38122=CARTESIAN_POINT('',(38.,-8.90000000000001,135.8));
#38123=CARTESIAN_POINT('',(37.9,-8.2,135.));
#38124=CARTESIAN_POINT('Origin',(37.9,-8.2,135.8));
#38125=CARTESIAN_POINT('',(38.,-8.2,135.1));
#38126=CARTESIAN_POINT('',(37.9,-8.2,135.));
#38127=CARTESIAN_POINT('Origin',(38.,-8.2,135.8));
#38128=CARTESIAN_POINT('Origin',(37.95,-8.95,142.5));
#38129=CARTESIAN_POINT('',(38.,-8.9,144.2));
#38130=CARTESIAN_POINT('',(38.,-8.9,142.5));
#38131=CARTESIAN_POINT('',(38.,-8.9,144.2));
#38132=CARTESIAN_POINT('',(37.9,-9.,142.5));
#38133=CARTESIAN_POINT('Origin',(37.95,-8.2,144.2));
#38134=CARTESIAN_POINT('',(38.,-8.2,144.9));
#38135=CARTESIAN_POINT('',(38.,-8.2,144.9));
#38136=CARTESIAN_POINT('Origin',(38.,-8.2,144.2));
#38137=CARTESIAN_POINT('Origin',(37.95,-5.25,144.95));
#38138=CARTESIAN_POINT('',(38.,-4.8,144.9));
#38139=CARTESIAN_POINT('',(38.,-5.25,144.9));
#38140=CARTESIAN_POINT('',(37.9,-4.8,145.));
#38141=CARTESIAN_POINT('',(38.,-4.8,144.9));
#38142=CARTESIAN_POINT('',(37.9,-5.25,145.));
#38143=CARTESIAN_POINT('Origin',(37.95,-4.8,144.2));
#38144=CARTESIAN_POINT('',(38.,-4.09999999999999,144.2));
#38145=CARTESIAN_POINT('',(38.,-4.09999999999999,144.2));
#38146=CARTESIAN_POINT('Origin',(37.9,-4.8,144.2));
#38147=CARTESIAN_POINT('Origin',(38.,-4.8,144.2));
#38148=CARTESIAN_POINT('Origin',(37.95,-4.05,137.5));
#38149=CARTESIAN_POINT('',(38.,-4.1,135.8));
#38150=CARTESIAN_POINT('',(38.,-4.1,137.5));
#38151=CARTESIAN_POINT('',(38.,-4.1,135.8));
#38152=CARTESIAN_POINT('Origin',(37.95,-4.8,135.8));
#38153=CARTESIAN_POINT('',(38.,-4.8,135.1));
#38154=CARTESIAN_POINT('',(37.9,-4.8,135.));
#38155=CARTESIAN_POINT('',(38.,-4.8,135.1));
#38156=CARTESIAN_POINT('Origin',(37.9,-4.8,135.8));
#38157=CARTESIAN_POINT('Origin',(38.,-4.8,135.8));
#38158=CARTESIAN_POINT('Origin',(37.95,-7.75,135.05));
#38159=CARTESIAN_POINT('',(38.,-7.75,135.1));
#38160=CARTESIAN_POINT('',(37.9,-7.75,135.));
#38161=CARTESIAN_POINT('Origin',(-38.,-4.8,135.8));
#38162=CARTESIAN_POINT('',(-38.,-4.8,135.));
#38163=CARTESIAN_POINT('',(-25.8,-4.8,135.));
#38164=CARTESIAN_POINT('',(-38.,-4.8,135.));
#38165=CARTESIAN_POINT('',(-37.9,-4.8,135.));
#38166=CARTESIAN_POINT('',(-38.,-4.8,135.));
#38167=CARTESIAN_POINT('Origin',(-37.9,-4.8,135.8));
#38168=CARTESIAN_POINT('Origin',(-38.,-9.,135.));
#38169=CARTESIAN_POINT('',(-38.,-8.2,135.));
#38170=CARTESIAN_POINT('Origin',(-38.,-8.2,135.8));
#38171=CARTESIAN_POINT('',(30.8485281374239,-9.,135.8));
#38172=CARTESIAN_POINT('',(-38.,-9.,135.8));
#38173=CARTESIAN_POINT('',(30.62442393624,-8.99442305443429,135.70570254201));
#38174=CARTESIAN_POINT('Ctrl Pts',(30.62442393624,-8.99442305443429,135.70570254201));
#38175=CARTESIAN_POINT('Ctrl Pts',(30.7010733797628,-8.99756721057679,135.732190956222));
#38176=CARTESIAN_POINT('Ctrl Pts',(30.7759616147067,-9.,135.763779566847));
#38177=CARTESIAN_POINT('Ctrl Pts',(30.8485281374239,-9.,135.8));
#38178=CARTESIAN_POINT('',(29.37557606376,-8.99442305443429,135.70570254201));
#38179=CARTESIAN_POINT('Ctrl Pts',(29.37557606376,-8.99442305443429,135.70570254201));
#38180=CARTESIAN_POINT('Ctrl Pts',(29.3968663992163,-8.99354972599348,135.698345055793));
#38181=CARTESIAN_POINT('Ctrl Pts',(29.418327451187,-8.9926309002887,135.69138245992));
#38182=CARTESIAN_POINT('Ctrl Pts',(29.5876626138109,-8.9849459908676,135.639432675438));
#38183=CARTESIAN_POINT('Ctrl Pts',(29.8198774693528,-8.97481364719588,135.600649477793));
#38184=CARTESIAN_POINT('Ctrl Pts',(30.1802232821902,-8.97487183787893,135.600774173325));
#38185=CARTESIAN_POINT('Ctrl Pts',(30.4123094665995,-8.98495128128084,135.639444028187));
#38186=CARTESIAN_POINT('Ctrl Pts',(30.5816752394099,-8.9926310079646,135.691382689721));
#38187=CARTESIAN_POINT('Ctrl Pts',(30.6031336007837,-8.99354972599348,135.698345055793));
#38188=CARTESIAN_POINT('Ctrl Pts',(30.62442393624,-8.99442305443429,135.70570254201));
#38189=CARTESIAN_POINT('',(29.1514718625761,-9.,135.8));
#38190=CARTESIAN_POINT('Ctrl Pts',(29.1514718625748,-9.,135.800000000001));
#38191=CARTESIAN_POINT('Ctrl Pts',(29.2240383852925,-9.00000000000003,135.763779566847));
#38192=CARTESIAN_POINT('Ctrl Pts',(29.2989266202368,-8.99756721057681,135.732190956222));
#38193=CARTESIAN_POINT('Ctrl Pts',(29.37557606376,-8.99442305443429,135.70570254201));
#38194=CARTESIAN_POINT('',(-29.1514718625761,-9.,135.8));
#38195=CARTESIAN_POINT('',(-38.,-9.,135.8));
#38196=CARTESIAN_POINT('',(-29.37557606376,-8.99442305443429,135.70570254201));
#38197=CARTESIAN_POINT('Ctrl Pts',(-29.37557606376,-8.99442305443429,135.70570254201));
#38198=CARTESIAN_POINT('Ctrl Pts',(-29.2989266202372,-8.99756721057679,
135.732190956222));
#38199=CARTESIAN_POINT('Ctrl Pts',(-29.2240383852933,-9.,135.763779566847));
#38200=CARTESIAN_POINT('Ctrl Pts',(-29.1514718625761,-9.,135.8));
#38201=CARTESIAN_POINT('',(-30.62442393624,-8.99442305443429,135.70570254201));
#38202=CARTESIAN_POINT('Ctrl Pts',(-30.62442393624,-8.99442305443429,135.70570254201));
#38203=CARTESIAN_POINT('Ctrl Pts',(-30.6031336007836,-8.99354972599348,
135.698345055793));
#38204=CARTESIAN_POINT('Ctrl Pts',(-30.5816983343991,-8.992618351102,135.691367354698));
#38205=CARTESIAN_POINT('Ctrl Pts',(-30.4860771888921,-8.98837705676011,
135.662197780903));
#38206=CARTESIAN_POINT('Ctrl Pts',(-30.3737545882272,-8.98306085361229,
135.635119083645));
#38207=CARTESIAN_POINT('Ctrl Pts',(-30.1448588692225,-8.97549018477832,
135.602654705543));
#38208=CARTESIAN_POINT('Ctrl Pts',(-29.8570705077091,-8.9729461125948,135.594307424048));
#38209=CARTESIAN_POINT('Ctrl Pts',(-29.5879619148511,-8.98495065878909,
135.639399710956));
#38210=CARTESIAN_POINT('Ctrl Pts',(-29.4183017766692,-8.99262938782785,
135.691384779087));
#38211=CARTESIAN_POINT('Ctrl Pts',(-29.3968663992164,-8.99354972599348,
135.698345055793));
#38212=CARTESIAN_POINT('Ctrl Pts',(-29.37557606376,-8.99442305443429,135.70570254201));
#38213=CARTESIAN_POINT('',(-30.8485281374239,-9.,135.8));
#38214=CARTESIAN_POINT('Ctrl Pts',(-30.8485281374251,-9.,135.800000000001));
#38215=CARTESIAN_POINT('Ctrl Pts',(-30.7759616147075,-9.00000000000003,
135.763779566847));
#38216=CARTESIAN_POINT('Ctrl Pts',(-30.7010733797632,-8.99756721057681,
135.732190956222));
#38217=CARTESIAN_POINT('Ctrl Pts',(-30.62442393624,-8.99442305443429,135.70570254201));
#38218=CARTESIAN_POINT('',(-37.9,-9.,135.8));
#38219=CARTESIAN_POINT('',(-38.,-9.,135.8));
#38220=CARTESIAN_POINT('',(-37.9,-8.2,135.));
#38221=CARTESIAN_POINT('Origin',(-37.9,-8.2,135.8));
#38222=CARTESIAN_POINT('',(-38.,-8.2,135.));
#38223=CARTESIAN_POINT('Origin',(38.,-6.5,140.));
#38224=CARTESIAN_POINT('',(38.,-8.5,144.));
#38225=CARTESIAN_POINT('',(38.,-8.5,136.));
#38226=CARTESIAN_POINT('',(38.,-8.5,137.8));
#38227=CARTESIAN_POINT('',(38.,-8.,144.5));
#38228=CARTESIAN_POINT('Origin',(38.,-8.,144.));
#38229=CARTESIAN_POINT('',(38.,-5.,144.5));
#38230=CARTESIAN_POINT('',(38.,-7.45,144.5));
#38231=CARTESIAN_POINT('',(38.,-4.50000000000002,144.));
#38232=CARTESIAN_POINT('Origin',(38.,-5.,144.));
#38233=CARTESIAN_POINT('',(38.,-4.5,136.));
#38234=CARTESIAN_POINT('',(38.,-4.5,142.2));
#38235=CARTESIAN_POINT('',(38.,-5.,135.5));
#38236=CARTESIAN_POINT('Origin',(38.,-5.,136.));
#38237=CARTESIAN_POINT('',(38.,-8.,135.5));
#38238=CARTESIAN_POINT('',(38.,-5.55,135.5));
#38239=CARTESIAN_POINT('Origin',(38.,-8.,136.));
#38240=CARTESIAN_POINT('Origin',(-37.95,-8.2,135.8));
#38241=CARTESIAN_POINT('',(-38.,-8.2,135.1));
#38242=CARTESIAN_POINT('',(-38.,-8.2,135.1));
#38243=CARTESIAN_POINT('',(-38.,-8.90000000000001,135.8));
#38244=CARTESIAN_POINT('',(-37.9,-9.,135.8));
#38245=CARTESIAN_POINT('Origin',(-38.,-8.2,135.8));
#38246=CARTESIAN_POINT('Origin',(-37.95,-7.75,135.05));
#38247=CARTESIAN_POINT('',(-38.,-4.8,135.1));
#38248=CARTESIAN_POINT('',(-38.,-7.75,135.1));
#38249=CARTESIAN_POINT('',(-38.,-4.8,135.1));
#38250=CARTESIAN_POINT('',(-37.9,-7.75,135.));
#38251=CARTESIAN_POINT('Origin',(-37.95,-4.8,135.8));
#38252=CARTESIAN_POINT('',(-38.,-4.09999999999999,135.8));
#38253=CARTESIAN_POINT('',(-38.,-4.09999999999999,135.8));
#38254=CARTESIAN_POINT('Origin',(-38.,-4.8,135.8));
#38255=CARTESIAN_POINT('Origin',(-37.95,-4.05,137.5));
#38256=CARTESIAN_POINT('',(-38.,-4.1,144.2));
#38257=CARTESIAN_POINT('',(-38.,-4.1,137.5));
#38258=CARTESIAN_POINT('',(-38.,-4.1,144.2));
#38259=CARTESIAN_POINT('Origin',(-37.95,-4.8,144.2));
#38260=CARTESIAN_POINT('',(-38.,-4.8,144.9));
#38261=CARTESIAN_POINT('',(-37.9,-4.8,145.));
#38262=CARTESIAN_POINT('',(-38.,-4.8,144.9));
#38263=CARTESIAN_POINT('Origin',(-37.9,-4.8,144.2));
#38264=CARTESIAN_POINT('Origin',(-38.,-4.8,144.2));
#38265=CARTESIAN_POINT('Origin',(-37.95,-5.25,144.95));
#38266=CARTESIAN_POINT('',(-38.,-8.2,144.9));
#38267=CARTESIAN_POINT('',(-38.,-5.25,144.9));
#38268=CARTESIAN_POINT('',(-38.,-8.2,144.9));
#38269=CARTESIAN_POINT('',(-37.9,-5.25,145.));
#38270=CARTESIAN_POINT('Origin',(-37.95,-8.2,144.2));
#38271=CARTESIAN_POINT('',(-38.,-8.90000000000001,144.2));
#38272=CARTESIAN_POINT('',(-38.,-8.90000000000001,144.2));
#38273=CARTESIAN_POINT('Origin',(-38.,-8.2,144.2));
#38274=CARTESIAN_POINT('Origin',(-37.95,-8.95,142.5));
#38275=CARTESIAN_POINT('',(-38.,-8.9,142.5));
#38276=CARTESIAN_POINT('',(-37.9,-9.,142.5));
#38277=CARTESIAN_POINT('Origin',(-38.,-4.,145.));
#38278=CARTESIAN_POINT('',(-38.,-4.8,145.));
#38279=CARTESIAN_POINT('Origin',(-38.,-9.,145.));
#38280=CARTESIAN_POINT('Origin',(-30.,-9.,142.5));
#38281=CARTESIAN_POINT('Origin',(-30.,-9.,137.5));
#38282=CARTESIAN_POINT('Origin',(30.,-9.,137.5));
#38283=CARTESIAN_POINT('',(3.47230558097363,-9.,138.054707050323));
#38284=CARTESIAN_POINT('',(2.71739415824413,-9.,138.770942211151));
#38285=CARTESIAN_POINT('Ctrl Pts',(3.47230558097363,-9.,138.054707050323));
#38286=CARTESIAN_POINT('Ctrl Pts',(3.00675420463085,-9.,138.281037330627));
#38287=CARTESIAN_POINT('Ctrl Pts',(2.71739415824413,-9.,138.770942211151));
#38288=CARTESIAN_POINT('',(2.42803601920605,-9.,139.997135639191));
#38289=CARTESIAN_POINT('Ctrl Pts',(2.71739415824413,-9.,138.770942211151));
#38290=CARTESIAN_POINT('Ctrl Pts',(2.42803601920605,-9.,139.260846614838));
#38291=CARTESIAN_POINT('Ctrl Pts',(2.42803601920605,-9.,139.997135639191));
#38292=CARTESIAN_POINT('',(3.00102452933788,-9.,141.598636388779));
#38293=CARTESIAN_POINT('Ctrl Pts',(2.42803601920605,-9.,139.997135639191));
#38294=CARTESIAN_POINT('Ctrl Pts',(2.42803601920605,-9.,141.025648593903));
#38295=CARTESIAN_POINT('Ctrl Pts',(3.00102452933788,-9.,141.598636388779));
#38296=CARTESIAN_POINT('',(4.59679441154003,-9.,142.171624183655));
#38297=CARTESIAN_POINT('Ctrl Pts',(3.00102452933788,-9.,141.598636388779));
#38298=CARTESIAN_POINT('Ctrl Pts',(3.57401113212109,-9.,142.171624183655));
#38299=CARTESIAN_POINT('Ctrl Pts',(4.59679441154003,-9.,142.171624183655));
#38300=CARTESIAN_POINT('',(6.2126200646162,-9.,141.60866355896));
#38301=CARTESIAN_POINT('Ctrl Pts',(4.59679441154003,-9.,142.171624183655));
#38302=CARTESIAN_POINT('Ctrl Pts',(5.64536122977734,-9.,142.171624183655));
#38303=CARTESIAN_POINT('Ctrl Pts',(6.2126200646162,-9.,141.60866355896));
#38304=CARTESIAN_POINT('',(6.77987699210644,-9.,140.031514644623));
#38305=CARTESIAN_POINT('Ctrl Pts',(6.2126200646162,-9.,141.60866355896));
#38306=CARTESIAN_POINT('Ctrl Pts',(6.77987699210644,-9.,141.045703411102));
#38307=CARTESIAN_POINT('Ctrl Pts',(6.77987699210644,-9.,140.031514644623));
#38308=CARTESIAN_POINT('',(6.53206090629101,-9.,138.823943138123));
#38309=CARTESIAN_POINT('Ctrl Pts',(6.77987699210644,-9.,140.031514644623));
#38310=CARTESIAN_POINT('Ctrl Pts',(6.77987699210644,-9.,139.29522562027));
#38311=CARTESIAN_POINT('Ctrl Pts',(6.53206090629101,-9.,138.823943138123));
#38312=CARTESIAN_POINT('',(5.81582669913769,-9.,138.090518951416));
#38313=CARTESIAN_POINT('Ctrl Pts',(6.53206090629101,-9.,138.823943138123));
#38314=CARTESIAN_POINT('Ctrl Pts',(6.28424291312695,-9.,138.352660655975));
#38315=CARTESIAN_POINT('Ctrl Pts',(5.81582669913769,-9.,138.090518951416));
#38316=CARTESIAN_POINT('',(4.64836339652538,-9.,137.828377246857));
#38317=CARTESIAN_POINT('Ctrl Pts',(5.81582669913769,-9.,138.090518951416));
#38318=CARTESIAN_POINT('Ctrl Pts',(5.3474085777998,-9.,137.828377246857));
#38319=CARTESIAN_POINT('Ctrl Pts',(4.64836339652538,-9.,137.828377246857));
#38320=CARTESIAN_POINT('Ctrl Pts',(4.64836339652538,-9.,137.828377246857));
#38321=CARTESIAN_POINT('Ctrl Pts',(3.93785886466503,-9.,137.828377246857));
#38322=CARTESIAN_POINT('Ctrl Pts',(3.47230558097363,-9.,138.054707050323));
#38323=CARTESIAN_POINT('',(-0.41684789955616,-9.,141.062892436981));
#38324=CARTESIAN_POINT('',(-1.74044962227345,-9.,141.062892436981));
#38325=CARTESIAN_POINT('',(-19.2084239497781,-9.,141.062892436981));
#38326=CARTESIAN_POINT('',(-1.74044962227345,-9.,142.10000038147));
#38327=CARTESIAN_POINT('',(-1.74044962227345,-9.,143.031446218491));
#38328=CARTESIAN_POINT('',(2.20457105338573,-9.,142.10000038147));
#38329=CARTESIAN_POINT('',(-19.8702248111367,-9.,142.10000038147));
#38330=CARTESIAN_POINT('',(2.20457105338573,-9.,141.062892436981));
#38331=CARTESIAN_POINT('',(2.20457105338573,-9.,143.550000190735));
#38332=CARTESIAN_POINT('',(0.880968376994133,-9.,141.062892436981));
#38333=CARTESIAN_POINT('',(-17.8977144733071,-9.,141.062892436981));
#38334=CARTESIAN_POINT('',(0.880968376994133,-9.,137.900000572205));
#38335=CARTESIAN_POINT('',(0.880968376994133,-9.,143.031446218491));
#38336=CARTESIAN_POINT('',(-0.41684789955616,-9.,137.900000572205));
#38337=CARTESIAN_POINT('',(-18.5595158115029,-9.,137.900000572205));
#38338=CARTESIAN_POINT('',(-0.41684789955616,-9.,141.450000286102));
#38339=CARTESIAN_POINT('',(-7.1838323622942,-9.,138.493042945862));
#38340=CARTESIAN_POINT('',(-7.42019005119801,-9.,139.127626895905));
#38341=CARTESIAN_POINT('Ctrl Pts',(-7.1838323622942,-9.,138.493042945862));
#38342=CARTESIAN_POINT('Ctrl Pts',(-7.33567447960377,-9.,138.725102901459));
#38343=CARTESIAN_POINT('Ctrl Pts',(-7.42019005119801,-9.,139.127626895905));
#38344=CARTESIAN_POINT('',(-7.50470562279224,-9.,140.01719045639));
#38345=CARTESIAN_POINT('Ctrl Pts',(-7.42019005119801,-9.,139.127626895905));
#38346=CARTESIAN_POINT('Ctrl Pts',(-7.50470562279224,-9.,139.53015089035));
#38347=CARTESIAN_POINT('Ctrl Pts',(-7.50470562279224,-9.,140.01719045639));
#38348=CARTESIAN_POINT('',(-7.07353182137012,-9.,141.693179368973));
#38349=CARTESIAN_POINT('Ctrl Pts',(-7.50470562279224,-9.,140.01719045639));
#38350=CARTESIAN_POINT('Ctrl Pts',(-7.50470562279224,-9.,141.214734554291));
#38351=CARTESIAN_POINT('Ctrl Pts',(-7.07353182137012,-9.,141.693179368973));
#38352=CARTESIAN_POINT('',(-5.75995798408985,-9.,142.171624183655));
#38353=CARTESIAN_POINT('Ctrl Pts',(-7.07353182137012,-9.,141.693179368973));
#38354=CARTESIAN_POINT('Ctrl Pts',(-6.64235849678516,-9.,142.171624183655));
#38355=CARTESIAN_POINT('Ctrl Pts',(-5.75995798408985,-9.,142.171624183655));
#38356=CARTESIAN_POINT('',(-5.06377764046192,-9.,142.067054271698));
#38357=CARTESIAN_POINT('Ctrl Pts',(-5.75995798408985,-9.,142.171624183655));
#38358=CARTESIAN_POINT('Ctrl Pts',(-5.3359467536211,-9.,142.171624183655));
#38359=CARTESIAN_POINT('Ctrl Pts',(-5.06377764046192,-9.,142.067054271698));
#38360=CARTESIAN_POINT('',(-4.61971254646778,-9.,141.794884681702));
#38361=CARTESIAN_POINT('Ctrl Pts',(-5.06377764046192,-9.,142.067054271698));
#38362=CARTESIAN_POINT('Ctrl Pts',(-4.79160852730274,-9.,141.962483882904));
#38363=CARTESIAN_POINT('Ctrl Pts',(-4.61971254646778,-9.,141.794884681702));
#38364=CARTESIAN_POINT('',(-4.34897585213184,-9.,141.442497253418));
#38365=CARTESIAN_POINT('Ctrl Pts',(-4.61971254646778,-9.,141.794884681702));
#38366=CARTESIAN_POINT('Ctrl Pts',(-4.44781656563282,-9.,141.627285718918));
#38367=CARTESIAN_POINT('Ctrl Pts',(-4.34897585213184,-9.,141.442497253418));
#38368=CARTESIAN_POINT('',(-4.18997164070606,-9.,141.011323928833));
#38369=CARTESIAN_POINT('Ctrl Pts',(-4.34897585213184,-9.,141.442497253418));
#38370=CARTESIAN_POINT('Ctrl Pts',(-4.25013513863087,-9.,141.2577085495));
#38371=CARTESIAN_POINT('Ctrl Pts',(-4.18997164070606,-9.,141.011323928833));
#38372=CARTESIAN_POINT('',(-4.07250948250294,-9.,140.031514644623));
#38373=CARTESIAN_POINT('Ctrl Pts',(-4.18997164070606,-9.,141.011323928833));
#38374=CARTESIAN_POINT('Ctrl Pts',(-4.07250948250294,-9.,140.541473865509));
#38375=CARTESIAN_POINT('Ctrl Pts',(-4.07250948250294,-9.,140.031514644623));
#38376=CARTESIAN_POINT('',(-4.45927591621876,-9.,138.358390808105));
#38377=CARTESIAN_POINT('Ctrl Pts',(-4.07250948250294,-9.,140.031514644623));
#38378=CARTESIAN_POINT('Ctrl Pts',(-4.07250948250294,-9.,138.888404369354));
#38379=CARTESIAN_POINT('Ctrl Pts',(-4.45927591621876,-9.,138.358390808105));
#38380=CARTESIAN_POINT('',(-5.7914721518755,-9.,137.828377246857));
#38381=CARTESIAN_POINT('Ctrl Pts',(-4.45927591621876,-9.,138.358390808105));
#38382=CARTESIAN_POINT('Ctrl Pts',(-4.84604234993458,-9.,137.828377246857));
#38383=CARTESIAN_POINT('Ctrl Pts',(-5.7914721518755,-9.,137.828377246857));
#38384=CARTESIAN_POINT('',(-6.64808912575245,-9.,137.997408390045));
#38385=CARTESIAN_POINT('Ctrl Pts',(-5.7914721518755,-9.,137.828377246857));
#38386=CARTESIAN_POINT('Ctrl Pts',(-6.32148618996143,-9.,137.828377246857));
#38387=CARTESIAN_POINT('Ctrl Pts',(-6.64808912575245,-9.,137.997408390045));
#38388=CARTESIAN_POINT('Ctrl Pts',(-6.64808912575245,-9.,137.997408390045));
#38389=CARTESIAN_POINT('Ctrl Pts',(-6.97469206154346,-9.,138.166440010071));
#38390=CARTESIAN_POINT('Ctrl Pts',(-7.1838323622942,-9.,138.493042945862));
#38391=CARTESIAN_POINT('',(-9.82530565559864,-9.,138.851160049438));
#38392=CARTESIAN_POINT('',(-8.00320501625538,-9.,138.851160049438));
#38393=CARTESIAN_POINT('',(-23.9126528277993,-9.,138.851160049438));
#38394=CARTESIAN_POINT('',(-8.00320501625538,-9.,137.900000572205));
#38395=CARTESIAN_POINT('',(-8.00320501625538,-9.,141.925580024719));
#38396=CARTESIAN_POINT('',(-11.5041598826647,-9.,137.900000572205));
#38397=CARTESIAN_POINT('',(-23.0016025081277,-9.,137.900000572205));
#38398=CARTESIAN_POINT('',(-11.1388804465532,-9.,138.875512123108));
#38399=CARTESIAN_POINT('Ctrl Pts',(-11.5041598826647,-9.,137.900000572205));
#38400=CARTESIAN_POINT('Ctrl Pts',(-11.4439961463213,-9.,138.41855430603));
#38401=CARTESIAN_POINT('Ctrl Pts',(-11.1388804465532,-9.,138.875512123108));
#38402=CARTESIAN_POINT('',(-9.99433727562428,-9.,139.954161167145));
#38403=CARTESIAN_POINT('Ctrl Pts',(-11.1388804465532,-9.,138.875512123108));
#38404=CARTESIAN_POINT('Ctrl Pts',(-10.833764269948,-9.,139.332469940186));
#38405=CARTESIAN_POINT('Ctrl Pts',(-9.99433727562428,-9.,139.954161167145));
#38406=CARTESIAN_POINT('',(-9.3382660895586,-9.,140.53287935257));
#38407=CARTESIAN_POINT('Ctrl Pts',(-9.99433727562428,-9.,139.954161167145));
#38408=CARTESIAN_POINT('Ctrl Pts',(-9.48151321709156,-9.,140.335197925568));
#38409=CARTESIAN_POINT('Ctrl Pts',(-9.3382660895586,-9.,140.53287935257));
#38410=CARTESIAN_POINT('',(-9.1950194388628,-9.,140.908185958862));
#38411=CARTESIAN_POINT('Ctrl Pts',(-9.3382660895586,-9.,140.53287935257));
#38412=CARTESIAN_POINT('Ctrl Pts',(-9.1950194388628,-9.,140.730559825897));
#38413=CARTESIAN_POINT('Ctrl Pts',(-9.1950194388628,-9.,140.908185958862));
#38414=CARTESIAN_POINT('',(-9.33683367073536,-9.,141.236221313477));
#38415=CARTESIAN_POINT('Ctrl Pts',(-9.1950194388628,-9.,140.908185958862));
#38416=CARTESIAN_POINT('Ctrl Pts',(-9.1950194388628,-9.,141.100136756897));
#38417=CARTESIAN_POINT('Ctrl Pts',(-9.33683367073536,-9.,141.236221313477));
#38418=CARTESIAN_POINT('',(-9.69351883232594,-9.,141.372305870056));
#38419=CARTESIAN_POINT('Ctrl Pts',(-9.33683367073536,-9.,141.236221313477));
#38420=CARTESIAN_POINT('Ctrl Pts',(-9.47864837944508,-9.,141.372305870056));
#38421=CARTESIAN_POINT('Ctrl Pts',(-9.69351883232594,-9.,141.372305870056));
#38422=CARTESIAN_POINT('',(-10.058798506856,-9.,141.231924057007));
#38423=CARTESIAN_POINT('Ctrl Pts',(-9.69351883232594,-9.,141.372305870056));
#38424=CARTESIAN_POINT('Ctrl Pts',(-9.91698379814625,-9.,141.372305870056));
#38425=CARTESIAN_POINT('Ctrl Pts',(-10.058798506856,-9.,141.231924057007));
#38426=CARTESIAN_POINT('',(-10.2493168860674,-9.,140.73628950119));
#38427=CARTESIAN_POINT('Ctrl Pts',(-10.058798506856,-9.,141.231924057007));
#38428=CARTESIAN_POINT('Ctrl Pts',(-10.2006127387285,-9.,141.09154176712));
#38429=CARTESIAN_POINT('Ctrl Pts',(-10.2493168860674,-9.,140.73628950119));
#38430=CARTESIAN_POINT('',(-11.4182116538286,-9.,140.830832958221));
#38431=CARTESIAN_POINT('',(-24.20578526978,-9.,141.865127447373));
#38432=CARTESIAN_POINT('',(-11.1660971194506,-9.,141.600068569183));
#38433=CARTESIAN_POINT('Ctrl Pts',(-11.4182116538286,-9.,140.830832958221));
#38434=CARTESIAN_POINT('Ctrl Pts',(-11.3494531661272,-9.,141.323601961136));
#38435=CARTESIAN_POINT('Ctrl Pts',(-11.1660971194506,-9.,141.600068569183));
#38436=CARTESIAN_POINT('',(-10.6489760428667,-9.,142.024079322815));
#38437=CARTESIAN_POINT('Ctrl Pts',(-11.1660971194506,-9.,141.600068569183));
#38438=CARTESIAN_POINT('Ctrl Pts',(-10.9827410727739,-9.,141.876535177231));
#38439=CARTESIAN_POINT('Ctrl Pts',(-10.6489760428667,-9.,142.024079322815));
#38440=CARTESIAN_POINT('',(-9.72503300011158,-9.,142.171623706818));
#38441=CARTESIAN_POINT('Ctrl Pts',(-10.6489760428667,-9.,142.024079322815));
#38442=CARTESIAN_POINT('Ctrl Pts',(-10.3152105361223,-9.,142.171623706818));
#38443=CARTESIAN_POINT('Ctrl Pts',(-9.72503300011158,-9.,142.171623706818));
#38444=CARTESIAN_POINT('',(-8.76671095192432,-9.,142.031241893768));
#38445=CARTESIAN_POINT('Ctrl Pts',(-9.72503300011158,-9.,142.171623706818));
#38446=CARTESIAN_POINT('Ctrl Pts',(-9.10907144844532,-9.,142.171623706818));
#38447=CARTESIAN_POINT('Ctrl Pts',(-8.76671095192432,-9.,142.031241893768));
#38448=CARTESIAN_POINT('',(-8.22810240089893,-9.,141.600068569183));
#38449=CARTESIAN_POINT('Ctrl Pts',(-8.76671095192432,-9.,142.031241893768));
#38450=CARTESIAN_POINT('Ctrl Pts',(-8.42435093224049,-9.,141.8908598423));
#38451=CARTESIAN_POINT('Ctrl Pts',(-8.22810240089893,-9.,141.600068569183));
#38452=CARTESIAN_POINT('',(-8.03185434639454,-9.,140.948295116425));
#38453=CARTESIAN_POINT('Ctrl Pts',(-8.22810240089893,-9.,141.600068569183));
#38454=CARTESIAN_POINT('Ctrl Pts',(-8.03185434639454,-9.,141.309277296066));
#38455=CARTESIAN_POINT('Ctrl Pts',(-8.03185434639454,-9.,140.948295116425));
#38456=CARTESIAN_POINT('',(-8.25675220787525,-9.,140.214870929718));
#38457=CARTESIAN_POINT('Ctrl Pts',(-8.03185434639454,-9.,140.948295116425));
#38458=CARTESIAN_POINT('Ctrl Pts',(-8.03185434639454,-9.,140.564393520355));
#38459=CARTESIAN_POINT('Ctrl Pts',(-8.25675220787525,-9.,140.214870929718));
#38460=CARTESIAN_POINT('',(-9.07469196617603,-9.,139.447067260742));
#38461=CARTESIAN_POINT('Ctrl Pts',(-8.25675220787525,-9.,140.214870929718));
#38462=CARTESIAN_POINT('Ctrl Pts',(-8.48165006935596,-9.,139.865348339081));
#38463=CARTESIAN_POINT('Ctrl Pts',(-9.07469196617603,-9.,139.447067260742));
#38464=CARTESIAN_POINT('',(-9.54597444832325,-9.,139.106139659882));
#38465=CARTESIAN_POINT('Ctrl Pts',(-9.07469196617603,-9.,139.447067260742));
#38466=CARTESIAN_POINT('Ctrl Pts',(-9.42707939445972,-9.,139.203547477722));
#38467=CARTESIAN_POINT('Ctrl Pts',(-9.54597444832325,-9.,139.106139659882));
#38468=CARTESIAN_POINT('Ctrl Pts',(-9.54597444832325,-9.,139.106139659882));
#38469=CARTESIAN_POINT('Ctrl Pts',(-9.66486950218678,-9.,139.008731842041));
#38470=CARTESIAN_POINT('Ctrl Pts',(-9.82530565559864,-9.,138.851160049438));
#38471=CARTESIAN_POINT('',(8.70797948539257,-9.,137.900000572205));
#38472=CARTESIAN_POINT('',(7.4875166863203,-9.,137.900000572205));
#38473=CARTESIAN_POINT('',(-14.6460102573037,-9.,137.900000572205));
#38474=CARTESIAN_POINT('',(7.4875166863203,-9.,142.10000038147));
#38475=CARTESIAN_POINT('',(7.4875166863203,-9.,141.450000286102));
#38476=CARTESIAN_POINT('',(8.69938497245312,-9.,142.10000038147));
#38477=CARTESIAN_POINT('',(-15.2562416568398,-9.,142.10000038147));
#38478=CARTESIAN_POINT('',(10.2808306664228,-9.,139.776356220245));
#38479=CARTESIAN_POINT('',(0.633198898756767,-9.,153.951780208601));
#38480=CARTESIAN_POINT('',(10.2808306664228,-9.,142.10000038147));
#38481=CARTESIAN_POINT('',(10.2808306664228,-9.,142.388178110123));
#38482=CARTESIAN_POINT('',(11.5041602104902,-9.,142.10000038147));
#38483=CARTESIAN_POINT('',(-13.8595846667886,-9.,142.10000038147));
#38484=CARTESIAN_POINT('',(11.5041602104902,-9.,137.900000572205));
#38485=CARTESIAN_POINT('',(11.5041602104902,-9.,143.550000190735));
#38486=CARTESIAN_POINT('',(10.2808306664228,-9.,137.900000572205));
#38487=CARTESIAN_POINT('',(-13.2479198947549,-9.,137.900000572205));
#38488=CARTESIAN_POINT('',(8.70797948539257,-9.,140.206097126007));
#38489=CARTESIAN_POINT('',(0.963975333484397,-9.,151.560268138963));
#38490=CARTESIAN_POINT('',(8.70797948539257,-9.,142.603048563004));
#38491=CARTESIAN_POINT('Origin',(-38.,-6.5,140.));
#38492=CARTESIAN_POINT('',(-38.,-8.5,136.));
#38493=CARTESIAN_POINT('',(-38.,-8.5,144.));
#38494=CARTESIAN_POINT('',(-38.,-8.5,137.8));
#38495=CARTESIAN_POINT('',(-38.,-8.,135.5));
#38496=CARTESIAN_POINT('Origin',(-38.,-8.,136.));
#38497=CARTESIAN_POINT('',(-38.,-5.,135.5));
#38498=CARTESIAN_POINT('',(-38.,-5.55,135.5));
#38499=CARTESIAN_POINT('',(-38.,-4.5,136.));
#38500=CARTESIAN_POINT('Origin',(-38.,-5.,136.));
#38501=CARTESIAN_POINT('',(-38.,-4.50000000000002,144.));
#38502=CARTESIAN_POINT('',(-38.,-4.5,142.2));
#38503=CARTESIAN_POINT('',(-38.,-5.,144.5));
#38504=CARTESIAN_POINT('Origin',(-38.,-5.,144.));
#38505=CARTESIAN_POINT('',(-38.,-8.,144.5));
#38506=CARTESIAN_POINT('',(-38.,-7.45,144.5));
#38507=CARTESIAN_POINT('Origin',(-38.,-8.,144.));
#38508=CARTESIAN_POINT('Origin',(-30.,-8.95,137.5));
#38509=CARTESIAN_POINT('',(-30.80386876177,-8.9,135.889473684211));
#38510=CARTESIAN_POINT('',(-30.8485281374239,-9.,135.8));
#38511=CARTESIAN_POINT('',(-31.8,-8.9,137.5));
#38512=CARTESIAN_POINT('Origin',(-30.,-8.9,137.5));
#38513=CARTESIAN_POINT('',(-29.19613123823,-8.9,135.889473684211));
#38514=CARTESIAN_POINT('Origin',(-30.,-8.9,137.5));
#38515=CARTESIAN_POINT('',(-29.19613123823,-8.9,135.889473684211));
#38516=CARTESIAN_POINT('Ctrl Pts',(-29.37557606376,-8.99442305443429,135.70570254201));
#38517=CARTESIAN_POINT('Ctrl Pts',(-29.3968663992164,-8.99354972599348,
135.698345055793));
#38518=CARTESIAN_POINT('Ctrl Pts',(-29.4183017766692,-8.99262938782785,
135.691384779087));
#38519=CARTESIAN_POINT('Ctrl Pts',(-29.5879619148511,-8.98495065878909,
135.639399710956));
#38520=CARTESIAN_POINT('Ctrl Pts',(-29.8570705077091,-8.9729461125948,135.594307424048));
#38521=CARTESIAN_POINT('Ctrl Pts',(-30.1448588692225,-8.97549018477832,
135.602654705543));
#38522=CARTESIAN_POINT('Ctrl Pts',(-30.3737545882272,-8.98306085361229,
135.635119083645));
#38523=CARTESIAN_POINT('Ctrl Pts',(-30.4860771888921,-8.98837705676011,
135.662197780903));
#38524=CARTESIAN_POINT('Ctrl Pts',(-30.5816983343991,-8.992618351102,135.691367354698));
#38525=CARTESIAN_POINT('Ctrl Pts',(-30.6031336007836,-8.99354972599348,
135.698345055793));
#38526=CARTESIAN_POINT('Ctrl Pts',(-30.62442393624,-8.99442305443429,135.70570254201));
#38527=CARTESIAN_POINT('Ctrl Pts',(-29.3865147164033,-8.96294870295619,
135.737135028007));
#38528=CARTESIAN_POINT('Ctrl Pts',(-29.4073401763186,-8.96237080371183,
135.729919445576));
#38529=CARTESIAN_POINT('Ctrl Pts',(-29.4283245697951,-8.96172080557183,
135.72309086562));
#38530=CARTESIAN_POINT('Ctrl Pts',(-29.5945002385617,-8.95618563279747,
135.671952952223));
#38531=CARTESIAN_POINT('Ctrl Pts',(-29.8591951245291,-8.94617870256798,
135.627077056189));
#38532=CARTESIAN_POINT('Ctrl Pts',(-30.1426747355265,-8.94833727126047,
135.635411682665));
#38533=CARTESIAN_POINT('Ctrl Pts',(-30.3677622830885,-8.95449993845067,
135.66762787594));
#38534=CARTESIAN_POINT('Ctrl Pts',(-30.4780284899699,-8.95865446655877,
135.694387451391));
#38535=CARTESIAN_POINT('Ctrl Pts',(-30.5716737136164,-8.96171637205332,
135.723071391253));
#38536=CARTESIAN_POINT('Ctrl Pts',(-30.5926609072949,-8.96236576597913,
135.729921064971));
#38537=CARTESIAN_POINT('Ctrl Pts',(-30.6134852835967,-8.96294870295619,
135.737135028007));
#38538=CARTESIAN_POINT('Ctrl Pts',(-29.3974533690467,-8.9314743514781,135.768567514003));
#38539=CARTESIAN_POINT('Ctrl Pts',(-29.4178165235133,-8.93117892228165,
135.761500915766));
#38540=CARTESIAN_POINT('Ctrl Pts',(-29.4383449903957,-8.93082558621927,
135.754789398524));
#38541=CARTESIAN_POINT('Ctrl Pts',(-29.6010478369904,-8.92735259191528,
135.704550691614));
#38542=CARTESIAN_POINT('Ctrl Pts',(-29.8613411523255,-8.91940114687363,
135.659840357084));
#38543=CARTESIAN_POINT('Ctrl Pts',(-30.1404740235453,-8.92117767633548,
135.668188953759));
#38544=CARTESIAN_POINT('Ctrl Pts',(-30.3617898553802,-8.92591554353793,
135.700139778803));
#38545=CARTESIAN_POINT('Ctrl Pts',(-30.4699427578485,-8.92894382168888,
135.726593040274));
#38546=CARTESIAN_POINT('Ctrl Pts',(-30.561657334651,-8.93081126900573,135.754772293159));
#38547=CARTESIAN_POINT('Ctrl Pts',(-30.5821823928732,-8.93118396001435,
135.761499296371));
#38548=CARTESIAN_POINT('Ctrl Pts',(-30.6025466309533,-8.9314743514781,135.768567514003));
#38549=CARTESIAN_POINT('Ctrl Pts',(-29.40839202169,-8.9,135.8));
#38550=CARTESIAN_POINT('Ctrl Pts',(-29.4282903006156,-8.9,135.793075305549));
#38551=CARTESIAN_POINT('Ctrl Pts',(-29.4483677835215,-8.89991700396325,
135.786495485057));
#38552=CARTESIAN_POINT('Ctrl Pts',(-29.6075861607011,-8.89858756592366,
135.737103932881));
#38553=CARTESIAN_POINT('Ctrl Pts',(-29.8634657691454,-8.89263373684681,
135.692609989225));
#38554=CARTESIAN_POINT('Ctrl Pts',(-30.1382898898493,-8.89402476281763,
135.700945930881));
#38555=CARTESIAN_POINT('Ctrl Pts',(-30.3557975502414,-8.89735462837631,
135.732648571097));
#38556=CARTESIAN_POINT('Ctrl Pts',(-30.4618940589263,-8.89922123148754,
135.758782710762));
#38557=CARTESIAN_POINT('Ctrl Pts',(-30.5516327138684,-8.89990928995705,
135.786476329714));
#38558=CARTESIAN_POINT('Ctrl Pts',(-30.5717096993844,-8.9,135.793075305549));
#38559=CARTESIAN_POINT('Ctrl Pts',(-30.59160797831,-8.9,135.8));
#38560=CARTESIAN_POINT('',(-30.59160797831,-8.9,135.8));
#38561=CARTESIAN_POINT('',(-30.59160797831,-8.9,135.8));
#38562=CARTESIAN_POINT('',(-29.40839202169,-8.9,135.8));
#38563=CARTESIAN_POINT('',(-29.37557606376,-8.99442305443429,135.70570254201));
#38564=CARTESIAN_POINT('Ctrl Pts',(-29.40839202169,-8.9,135.8));
#38565=CARTESIAN_POINT('Ctrl Pts',(-29.4282903006156,-8.9,135.793075305549));
#38566=CARTESIAN_POINT('Ctrl Pts',(-29.4483677835215,-8.89991700396325,
135.786495485057));
#38567=CARTESIAN_POINT('Ctrl Pts',(-29.6075861607011,-8.89858756592366,
135.737103932881));
#38568=CARTESIAN_POINT('Ctrl Pts',(-29.8634657691454,-8.89263373684681,
135.692609989225));
#38569=CARTESIAN_POINT('Ctrl Pts',(-30.1382898898493,-8.89402476281763,
135.700945930881));
#38570=CARTESIAN_POINT('Ctrl Pts',(-30.3557975502414,-8.89735462837631,
135.732648571097));
#38571=CARTESIAN_POINT('Ctrl Pts',(-30.4618940589263,-8.89922123148754,
135.758782710762));
#38572=CARTESIAN_POINT('Ctrl Pts',(-30.5516327138684,-8.89990928995705,
135.786476329714));
#38573=CARTESIAN_POINT('Ctrl Pts',(-30.5717096993844,-8.9,135.793075305549));
#38574=CARTESIAN_POINT('Ctrl Pts',(-30.59160797831,-8.9,135.8));
#38575=CARTESIAN_POINT('Ctrl Pts',(-29.1514718625761,-9.,135.8));
#38576=CARTESIAN_POINT('Ctrl Pts',(-29.2240383852933,-9.,135.763779566847));
#38577=CARTESIAN_POINT('Ctrl Pts',(-29.2989266202372,-8.99756721057679,
135.732190956222));
#38578=CARTESIAN_POINT('Ctrl Pts',(-29.37557606376,-8.99442305443429,135.70570254201));
#38579=CARTESIAN_POINT('Ctrl Pts',(-29.1663583211274,-8.96666666666667,
135.829824561404));
#38580=CARTESIAN_POINT('Ctrl Pts',(-29.2376517469549,-8.96666666666667,
135.794239574446));
#38581=CARTESIAN_POINT('Ctrl Pts',(-29.3112262464824,-8.96504480705119,
135.763211800971));
#38582=CARTESIAN_POINT('Ctrl Pts',(-29.3865147164034,-8.96294870295619,
135.737135028007));
#38583=CARTESIAN_POINT('Ctrl Pts',(-29.1812447796787,-8.93333333333333,
135.859649122807));
#38584=CARTESIAN_POINT('Ctrl Pts',(-29.2512651086164,-8.93333333333333,
135.824699582045));
#38585=CARTESIAN_POINT('Ctrl Pts',(-29.3235258727276,-8.9325224035256,135.79423264572));
#38586=CARTESIAN_POINT('Ctrl Pts',(-29.3974533690467,-8.9314743514781,135.768567514003));
#38587=CARTESIAN_POINT('Ctrl Pts',(-29.19613123823,-8.9,135.889473684211));
#38588=CARTESIAN_POINT('Ctrl Pts',(-29.2648784702779,-8.9,135.855159589644));
#38589=CARTESIAN_POINT('Ctrl Pts',(-29.3358254989728,-8.9,135.825253490469));
#38590=CARTESIAN_POINT('Ctrl Pts',(-29.40839202169,-8.9,135.8));
#38591=CARTESIAN_POINT('Ctrl Pts',(-29.19613123823,-8.9,135.889473684211));
#38592=CARTESIAN_POINT('Ctrl Pts',(-29.2648784702779,-8.9,135.855159589644));
#38593=CARTESIAN_POINT('Ctrl Pts',(-29.3358254989728,-8.9,135.825253490469));
#38594=CARTESIAN_POINT('Ctrl Pts',(-29.40839202169,-8.9,135.8));
#38595=CARTESIAN_POINT('Ctrl Pts',(-30.62442393624,-8.99442305443429,135.70570254201));
#38596=CARTESIAN_POINT('Ctrl Pts',(-30.7010733797632,-8.99756721057681,
135.732190956222));
#38597=CARTESIAN_POINT('Ctrl Pts',(-30.7759616147075,-9.00000000000003,
135.763779566847));
#38598=CARTESIAN_POINT('Ctrl Pts',(-30.8485281374251,-9.,135.800000000001));
#38599=CARTESIAN_POINT('Ctrl Pts',(-30.6134852835967,-8.96294870295619,
135.737135028007));
#38600=CARTESIAN_POINT('Ctrl Pts',(-30.688773753518,-8.96504480705121,135.763211800971));
#38601=CARTESIAN_POINT('Ctrl Pts',(-30.762348253046,-8.96666666666669,135.794239574446));
#38602=CARTESIAN_POINT('Ctrl Pts',(-30.8336416788738,-8.96666666666667,
135.829824561404));
#38603=CARTESIAN_POINT('Ctrl Pts',(-30.6025466309533,-8.9314743514781,135.768567514003));
#38604=CARTESIAN_POINT('Ctrl Pts',(-30.6764741272728,-8.9325224035256,135.79423264572));
#38605=CARTESIAN_POINT('Ctrl Pts',(-30.7487348913845,-8.93333333333334,
135.824699582045));
#38606=CARTESIAN_POINT('Ctrl Pts',(-30.8187552203225,-8.93333333333333,
135.859649122808));
#38607=CARTESIAN_POINT('Ctrl Pts',(-30.59160797831,-8.9,135.8));
#38608=CARTESIAN_POINT('Ctrl Pts',(-30.6641745010276,-8.9,135.825253490469));
#38609=CARTESIAN_POINT('Ctrl Pts',(-30.7351215297229,-8.9,135.855159589645));
#38610=CARTESIAN_POINT('Ctrl Pts',(-30.8038687617712,-8.9,135.889473684211));
#38611=CARTESIAN_POINT('Ctrl Pts',(-30.59160797831,-8.9,135.8));
#38612=CARTESIAN_POINT('Ctrl Pts',(-30.6641745010276,-8.9,135.825253490469));
#38613=CARTESIAN_POINT('Ctrl Pts',(-30.7351215297229,-8.9,135.855159589645));
#38614=CARTESIAN_POINT('Ctrl Pts',(-30.8038687617712,-8.9,135.889473684211));
#38615=CARTESIAN_POINT('Origin',(-30.,-9.1,137.5));
#38616=CARTESIAN_POINT('',(-31.8,-8.5,137.5));
#38617=CARTESIAN_POINT('',(-31.8,-9.1,137.5));
#38618=CARTESIAN_POINT('',(-28.8951880620293,-8.5,136.078947368421));
#38619=CARTESIAN_POINT('Origin',(-30.,-8.5,137.5));
#38620=CARTESIAN_POINT('',(-29.0050125628934,-8.5,136.));
#38621=CARTESIAN_POINT('Ctrl Pts',(-29.0050125628934,-8.5,136.));
#38622=CARTESIAN_POINT('Ctrl Pts',(-28.9674326867105,-8.5,136.024927669793));
#38623=CARTESIAN_POINT('Ctrl Pts',(-28.9307900499921,-8.5,136.051268237865));
#38624=CARTESIAN_POINT('Ctrl Pts',(-28.8951880620293,-8.5,136.078947368421));
#38625=CARTESIAN_POINT('',(-30.9949874371066,-8.5,136.));
#38626=CARTESIAN_POINT('Ctrl Pts',(-30.9949874371066,-8.49999999999999,
136.));
#38627=CARTESIAN_POINT('Ctrl Pts',(-30.9864258065899,-8.49999999999999,
135.994320856796));
#38628=CARTESIAN_POINT('Ctrl Pts',(-30.9778381230699,-8.49988813409469,
135.988729270797));
#38629=CARTESIAN_POINT('Ctrl Pts',(-30.9692255759031,-8.49967145659891,
135.98322540583));
#38630=CARTESIAN_POINT('Ctrl Pts',(-30.9575142878076,-8.49937681988719,
135.975741284465));
#38631=CARTESIAN_POINT('Ctrl Pts',(-30.9457625581667,-8.49890259856714,
135.968422529549));
#38632=CARTESIAN_POINT('Ctrl Pts',(-30.9339621958604,-8.49823351737353,
135.96125838821));
#38633=CARTESIAN_POINT('Ctrl Pts',(-30.7382389594249,-8.48713599907262,
135.842432466377));
#38634=CARTESIAN_POINT('Ctrl Pts',(-30.5325493637783,-8.43232113429654,
135.768015720853));
#38635=CARTESIAN_POINT('Ctrl Pts',(-30.3291860222081,-8.39687027010474,
135.730147139418));
#38636=CARTESIAN_POINT('Ctrl Pts',(-30.2613982416847,-8.38505331537414,
135.71752427894));
#38637=CARTESIAN_POINT('Ctrl Pts',(-30.1938689338364,-8.37538791626402,
135.708962325583));
#38638=CARTESIAN_POINT('Ctrl Pts',(-30.1265373999854,-8.36988598131025,
135.704221903279));
#38639=CARTESIAN_POINT('Ctrl Pts',(-30.1036817054724,-8.36801834905324,
135.702612766552));
#38640=CARTESIAN_POINT('Ctrl Pts',(-30.0808735113911,-8.36662503132802,
135.701446014506));
#38641=CARTESIAN_POINT('Ctrl Pts',(-30.058041456041,-8.3657453936638,135.700711749912));
#38642=CARTESIAN_POINT('Ctrl Pts',(-30.0470380871301,-8.36532147310216,
135.700357888462));
#38643=CARTESIAN_POINT('Ctrl Pts',(-30.0360440525282,-8.36501787270752,
135.700106267186));
#38644=CARTESIAN_POINT('Ctrl Pts',(-30.0250429177668,-8.36483405979588,
135.69995393212));
#38645=CARTESIAN_POINT('Ctrl Pts',(-29.9790828012595,-8.36406613330308,
135.699317512559));
#38646=CARTESIAN_POINT('Ctrl Pts',(-29.9332009560837,-8.36546505443064,
135.700441545649));
#38647=CARTESIAN_POINT('Ctrl Pts',(-29.8872148113109,-8.36886140284219,
135.703319027206));
#38648=CARTESIAN_POINT('Ctrl Pts',(-29.8534299813378,-8.37135661208795,
135.705433038408));
#38649=CARTESIAN_POINT('Ctrl Pts',(-29.8195500300793,-8.37490071039475,
135.708573055883));
#38650=CARTESIAN_POINT('Ctrl Pts',(-29.7857448394163,-8.37930108895748,
135.71256873066));
#38651=CARTESIAN_POINT('Ctrl Pts',(-29.5878064298017,-8.40506647934065,
135.73596447241));
#38652=CARTESIAN_POINT('Ctrl Pts',(-29.3817762259822,-8.46017177748972,
135.795991006845));
#38653=CARTESIAN_POINT('Ctrl Pts',(-29.190935014294,-8.48601923378606,135.891967734794));
#38654=CARTESIAN_POINT('Ctrl Pts',(-29.1273212770646,-8.49463505255151,
135.923959977444));
#38655=CARTESIAN_POINT('Ctrl Pts',(-29.0653952056276,-8.49999999999999,
135.95994668604));
#38656=CARTESIAN_POINT('Ctrl Pts',(-29.0050125628934,-8.49999999999999,
136.));
#38657=CARTESIAN_POINT('',(-31.1048119379707,-8.5,136.078947368421));
#38658=CARTESIAN_POINT('Ctrl Pts',(-31.1048119379707,-8.5,136.078947368421));
#38659=CARTESIAN_POINT('Ctrl Pts',(-31.0692099500079,-8.5,136.051268237865));
#38660=CARTESIAN_POINT('Ctrl Pts',(-31.0325673132895,-8.5,136.024927669793));
#38661=CARTESIAN_POINT('Ctrl Pts',(-30.9949874371066,-8.5,136.));
#38662=CARTESIAN_POINT('Origin',(-30.,-8.5,137.5));
#38663=CARTESIAN_POINT('Origin',(-30.,-8.95,142.5));
#38664=CARTESIAN_POINT('',(-29.19613123823,-8.9,144.110526315789));
#38665=CARTESIAN_POINT('',(-29.1514718625761,-9.,144.2));
#38666=CARTESIAN_POINT('',(-31.8,-8.9,142.5));
#38667=CARTESIAN_POINT('Origin',(-30.,-8.9,142.5));
#38668=CARTESIAN_POINT('',(-30.80386876177,-8.9,144.110526315789));
#38669=CARTESIAN_POINT('Origin',(-30.,-8.9,142.5));
#38670=CARTESIAN_POINT('',(-30.80386876177,-8.9,144.110526315789));
#38671=CARTESIAN_POINT('Ctrl Pts',(-30.62442393624,-8.99442305443429,144.29429745799));
#38672=CARTESIAN_POINT('Ctrl Pts',(-30.5471210576335,-8.99125209441902,
144.321011685441));
#38673=CARTESIAN_POINT('Ctrl Pts',(-30.3890975283267,-8.98340931878656,
144.364446023987));
#38674=CARTESIAN_POINT('Ctrl Pts',(-30.1466727558104,-8.97528496697549,
144.397455998416));
#38675=CARTESIAN_POINT('Ctrl Pts',(-29.917310908637,-8.97429943254969,144.401048817597));
#38676=CARTESIAN_POINT('Ctrl Pts',(-29.6784757526138,-8.98055560583611,
144.37677095198));
#38677=CARTESIAN_POINT('Ctrl Pts',(-29.5181405190621,-8.98818372075475,
144.339120021515));
#38678=CARTESIAN_POINT('Ctrl Pts',(-29.4183151210873,-8.99261764548661,
144.308633020031));
#38679=CARTESIAN_POINT('Ctrl Pts',(-29.3968663992163,-8.99354972599348,
144.301654944207));
#38680=CARTESIAN_POINT('Ctrl Pts',(-29.37557606376,-8.99442305443429,144.29429745799));
#38681=CARTESIAN_POINT('Ctrl Pts',(-30.6134852835967,-8.96294870295619,
144.262864971993));
#38682=CARTESIAN_POINT('Ctrl Pts',(-30.537876135733,-8.960832400444,144.289055422042));
#38683=CARTESIAN_POINT('Ctrl Pts',(-30.3829031149238,-8.95481445077649,
144.331914740378));
#38684=CARTESIAN_POINT('Ctrl Pts',(-30.1444415014392,-8.94813920653503,
144.364709891608));
#38685=CARTESIAN_POINT('Ctrl Pts',(-29.9185623382477,-8.94731537891439,
144.36828875045));
#38686=CARTESIAN_POINT('Ctrl Pts',(-29.6835143198945,-8.95249912929929,
144.344141487335));
#38687=CARTESIAN_POINT('Ctrl Pts',(-29.5261156183802,-8.95851695974801,
144.306903693678));
#38688=CARTESIAN_POINT('Ctrl Pts',(-29.4283364833029,-8.96171515071183,
144.276929968692));
#38689=CARTESIAN_POINT('Ctrl Pts',(-29.4073412881907,-8.96236610430249,
144.27007827294));
#38690=CARTESIAN_POINT('Ctrl Pts',(-29.3865147164033,-8.96294870295619,
144.262864971993));
#38691=CARTESIAN_POINT('Ctrl Pts',(-30.6025466309533,-8.9314743514781,144.231432485997));
#38692=CARTESIAN_POINT('Ctrl Pts',(-30.5286044265584,-8.93041969397501,
144.257099071301));
#38693=CARTESIAN_POINT('Ctrl Pts',(-30.3767148747571,-8.9262174145652,144.29938163169));
#38694=CARTESIAN_POINT('Ctrl Pts',(-30.1421910885359,-8.92099903862342,
144.331963749486));
#38695=CARTESIAN_POINT('Ctrl Pts',(-29.9198243048248,-8.9203341020548,144.335531895016));
#38696=CARTESIAN_POINT('Ctrl Pts',(-29.6885516308557,-8.92443685309091,
144.311509099425));
#38697=CARTESIAN_POINT('Ctrl Pts',(-29.5340873690899,-8.92885561901168,
144.274685263127));
#38698=CARTESIAN_POINT('Ctrl Pts',(-29.4383588129063,-8.93081117793894,
144.24522727937));
#38699=CARTESIAN_POINT('Ctrl Pts',(-29.4178154116412,-8.93118362169099,
144.238501365718));
#38700=CARTESIAN_POINT('Ctrl Pts',(-29.3974533690467,-8.9314743514781,144.231432485997));
#38701=CARTESIAN_POINT('Ctrl Pts',(-30.59160797831,-8.9,144.2));
#38702=CARTESIAN_POINT('Ctrl Pts',(-30.5193595046579,-8.9,144.225142807902));
#38703=CARTESIAN_POINT('Ctrl Pts',(-30.3705204613541,-8.89762254655513,
144.266850348081));
#38704=CARTESIAN_POINT('Ctrl Pts',(-30.1399598341647,-8.89385327818296,
144.299217642678));
#38705=CARTESIAN_POINT('Ctrl Pts',(-29.9210757344354,-8.8933500484195,144.302771827868));
#38706=CARTESIAN_POINT('Ctrl Pts',(-29.6935901981364,-8.89638037655408,
144.27887963478));
#38707=CARTESIAN_POINT('Ctrl Pts',(-29.542062468408,-8.89918885800494,144.242468935291));
#38708=CARTESIAN_POINT('Ctrl Pts',(-29.448380175122,-8.89990868316417,144.213524228031));
#38709=CARTESIAN_POINT('Ctrl Pts',(-29.4282903006156,-8.9,144.206924694451));
#38710=CARTESIAN_POINT('Ctrl Pts',(-29.40839202169,-8.9,144.2));
#38711=CARTESIAN_POINT('',(-29.40839202169,-8.9,144.2));
#38712=CARTESIAN_POINT('',(-29.40839202169,-8.9,144.2));
#38713=CARTESIAN_POINT('',(-30.59160797831,-8.9,144.2));
#38714=CARTESIAN_POINT('',(-30.62442393624,-8.99442305443429,144.29429745799));
#38715=CARTESIAN_POINT('Ctrl Pts',(-30.59160797831,-8.9,144.2));
#38716=CARTESIAN_POINT('Ctrl Pts',(-30.5193595046579,-8.9,144.225142807902));
#38717=CARTESIAN_POINT('Ctrl Pts',(-30.3705204613541,-8.89762254655513,
144.266850348081));
#38718=CARTESIAN_POINT('Ctrl Pts',(-30.1399598341647,-8.89385327818296,
144.299217642678));
#38719=CARTESIAN_POINT('Ctrl Pts',(-29.9210757344354,-8.8933500484195,144.302771827868));
#38720=CARTESIAN_POINT('Ctrl Pts',(-29.6935901981364,-8.89638037655408,
144.27887963478));
#38721=CARTESIAN_POINT('Ctrl Pts',(-29.542062468408,-8.89918885800494,144.242468935291));
#38722=CARTESIAN_POINT('Ctrl Pts',(-29.448380175122,-8.89990868316417,144.213524228031));
#38723=CARTESIAN_POINT('Ctrl Pts',(-29.4282903006156,-8.9,144.206924694451));
#38724=CARTESIAN_POINT('Ctrl Pts',(-29.40839202169,-8.9,144.2));
#38725=CARTESIAN_POINT('Ctrl Pts',(-30.8485281374239,-9.,144.2));
#38726=CARTESIAN_POINT('Ctrl Pts',(-30.7759616147067,-9.,144.236220433153));
#38727=CARTESIAN_POINT('Ctrl Pts',(-30.7010733797628,-8.99756721057679,
144.267809043778));
#38728=CARTESIAN_POINT('Ctrl Pts',(-30.62442393624,-8.99442305443429,144.29429745799));
#38729=CARTESIAN_POINT('Ctrl Pts',(-30.8336416788726,-8.96666666666667,
144.170175438596));
#38730=CARTESIAN_POINT('Ctrl Pts',(-30.7623482530451,-8.96666666666667,
144.205760425554));
#38731=CARTESIAN_POINT('Ctrl Pts',(-30.6887737535176,-8.96504480705119,
144.236788199029));
#38732=CARTESIAN_POINT('Ctrl Pts',(-30.6134852835966,-8.96294870295619,
144.262864971993));
#38733=CARTESIAN_POINT('Ctrl Pts',(-30.8187552203213,-8.93333333333333,
144.140350877193));
#38734=CARTESIAN_POINT('Ctrl Pts',(-30.7487348913836,-8.93333333333333,
144.175300417955));
#38735=CARTESIAN_POINT('Ctrl Pts',(-30.6764741272724,-8.9325224035256,144.20576735428));
#38736=CARTESIAN_POINT('Ctrl Pts',(-30.6025466309533,-8.9314743514781,144.231432485997));
#38737=CARTESIAN_POINT('Ctrl Pts',(-30.80386876177,-8.9,144.110526315789));
#38738=CARTESIAN_POINT('Ctrl Pts',(-30.7351215297221,-8.9,144.144840410356));
#38739=CARTESIAN_POINT('Ctrl Pts',(-30.6641745010272,-8.9,144.174746509531));
#38740=CARTESIAN_POINT('Ctrl Pts',(-30.59160797831,-8.9,144.2));
#38741=CARTESIAN_POINT('Ctrl Pts',(-30.80386876177,-8.9,144.110526315789));
#38742=CARTESIAN_POINT('Ctrl Pts',(-30.7351215297221,-8.9,144.144840410356));
#38743=CARTESIAN_POINT('Ctrl Pts',(-30.6641745010272,-8.9,144.174746509531));
#38744=CARTESIAN_POINT('Ctrl Pts',(-30.59160797831,-8.9,144.2));
#38745=CARTESIAN_POINT('Ctrl Pts',(-29.37557606376,-8.99442305443429,144.29429745799));
#38746=CARTESIAN_POINT('Ctrl Pts',(-29.2989266202368,-8.99756721057681,
144.267809043778));
#38747=CARTESIAN_POINT('Ctrl Pts',(-29.2240383852925,-9.00000000000003,
144.236220433153));
#38748=CARTESIAN_POINT('Ctrl Pts',(-29.1514718625749,-9.,144.199999999999));
#38749=CARTESIAN_POINT('Ctrl Pts',(-29.3865147164033,-8.96294870295619,
144.262864971993));
#38750=CARTESIAN_POINT('Ctrl Pts',(-29.311226246482,-8.96504480705121,144.236788199029));
#38751=CARTESIAN_POINT('Ctrl Pts',(-29.237651746954,-8.96666666666669,144.205760425554));
#38752=CARTESIAN_POINT('Ctrl Pts',(-29.1663583211262,-8.96666666666667,
144.170175438596));
#38753=CARTESIAN_POINT('Ctrl Pts',(-29.3974533690467,-8.9314743514781,144.231432485997));
#38754=CARTESIAN_POINT('Ctrl Pts',(-29.3235258727272,-8.9325224035256,144.20576735428));
#38755=CARTESIAN_POINT('Ctrl Pts',(-29.2512651086155,-8.93333333333334,
144.175300417955));
#38756=CARTESIAN_POINT('Ctrl Pts',(-29.1812447796775,-8.93333333333333,
144.140350877192));
#38757=CARTESIAN_POINT('Ctrl Pts',(-29.40839202169,-8.9,144.2));
#38758=CARTESIAN_POINT('Ctrl Pts',(-29.3358254989724,-8.9,144.174746509531));
#38759=CARTESIAN_POINT('Ctrl Pts',(-29.2648784702771,-8.9,144.144840410355));
#38760=CARTESIAN_POINT('Ctrl Pts',(-29.1961312382288,-8.9,144.110526315789));
#38761=CARTESIAN_POINT('Ctrl Pts',(-29.40839202169,-8.9,144.2));
#38762=CARTESIAN_POINT('Ctrl Pts',(-29.3358254989724,-8.9,144.174746509531));
#38763=CARTESIAN_POINT('Ctrl Pts',(-29.2648784702771,-8.9,144.144840410355));
#38764=CARTESIAN_POINT('Ctrl Pts',(-29.1961312382288,-8.9,144.110526315789));
#38765=CARTESIAN_POINT('Origin',(-30.,-9.1,142.5));
#38766=CARTESIAN_POINT('',(-31.8,-8.5,142.5));
#38767=CARTESIAN_POINT('',(-31.8,-9.1,142.5));
#38768=CARTESIAN_POINT('',(-31.1048119379707,-8.5,143.921052631579));
#38769=CARTESIAN_POINT('Origin',(-30.,-8.5,142.5));
#38770=CARTESIAN_POINT('',(-30.9949874371066,-8.5,144.));
#38771=CARTESIAN_POINT('Ctrl Pts',(-30.9949874371066,-8.5,144.));
#38772=CARTESIAN_POINT('Ctrl Pts',(-31.0325673132895,-8.5,143.975072330207));
#38773=CARTESIAN_POINT('Ctrl Pts',(-31.0692099500079,-8.5,143.948731762135));
#38774=CARTESIAN_POINT('Ctrl Pts',(-31.1048119379707,-8.5,143.921052631579));
#38775=CARTESIAN_POINT('',(-29.0050125628934,-8.5,144.));
#38776=CARTESIAN_POINT('Ctrl Pts',(-29.0050125628934,-8.5,144.));
#38777=CARTESIAN_POINT('Ctrl Pts',(-29.0135741934101,-8.5,144.005679143204));
#38778=CARTESIAN_POINT('Ctrl Pts',(-29.0221619253429,-8.4998882739462,144.011270538495));
#38779=CARTESIAN_POINT('Ctrl Pts',(-29.0307753006606,-8.49967147839431,
144.016774290117));
#38780=CARTESIAN_POINT('Ctrl Pts',(-29.0424877148706,-8.49937668115061,
144.024258257358));
#38781=CARTESIAN_POINT('Ctrl Pts',(-29.054233030776,-8.49890414205457,144.031576926818));
#38782=CARTESIAN_POINT('Ctrl Pts',(-29.0660434123263,-8.49823289869332,
144.038740617387));
#38783=CARTESIAN_POINT('Ctrl Pts',(-29.277590700997,-8.48620960270521,144.167056481715));
#38784=CARTESIAN_POINT('Ctrl Pts',(-29.5004115805678,-8.42327948228293,
144.243514249585));
#38785=CARTESIAN_POINT('Ctrl Pts',(-29.7197482645007,-8.38872354766437,
144.278132830397));
#38786=CARTESIAN_POINT('Ctrl Pts',(-29.7712146119589,-8.38061515600853,
144.286255921694));
#38787=CARTESIAN_POINT('Ctrl Pts',(-29.8223406852117,-8.37404368722705,
144.292034257043));
#38788=CARTESIAN_POINT('Ctrl Pts',(-29.8735668070041,-8.36986017962019,
144.295641194803));
#38789=CARTESIAN_POINT('Ctrl Pts',(-29.8964405677882,-8.36799213751804,
144.297251783865));
#38790=CARTESIAN_POINT('Ctrl Pts',(-29.9192352880058,-8.36659893094219,
144.298417568824));
#38791=CARTESIAN_POINT('Ctrl Pts',(-29.942070594606,-8.36571923963916,144.299151535527));
#38792=CARTESIAN_POINT('Ctrl Pts',(-29.95307553038,-8.36529529322757,144.299505253415));
#38793=CARTESIAN_POINT('Ctrl Pts',(-29.9640684060312,-8.36499139205626,
144.299757367469));
#38794=CARTESIAN_POINT('Ctrl Pts',(-29.9750704969496,-8.36480784914122,
144.299909021531));
#38795=CARTESIAN_POINT('Ctrl Pts',(-30.0210346080518,-8.36404105062979,
144.300542596022));
#38796=CARTESIAN_POINT('Ctrl Pts',(-30.0669049083367,-8.36543824175049,
144.299429100544));
#38797=CARTESIAN_POINT('Ctrl Pts',(-30.1129265755806,-8.36883370635998,
144.296534555326));
#38798=CARTESIAN_POINT('Ctrl Pts',(-30.1467375029954,-8.37132826629937,
144.294408007895));
#38799=CARTESIAN_POINT('Ctrl Pts',(-30.1805106645095,-8.37487119501038,
144.291330477666));
#38800=CARTESIAN_POINT('Ctrl Pts',(-30.2144446411448,-8.37927237236399,
144.287258125721));
#38801=CARTESIAN_POINT('Ctrl Pts',(-30.2556816511839,-8.384620740363,144.282309350639));
#38802=CARTESIAN_POINT('Ctrl Pts',(-30.2969770291942,-8.39120800293779,
144.275903976857));
#38803=CARTESIAN_POINT('Ctrl Pts',(-30.3383389567193,-8.39854217138171,
144.267993613037));
#38804=CARTESIAN_POINT('Ctrl Pts',(-30.4505209105317,-8.41843392679202,
144.246539098663));
#38805=CARTESIAN_POINT('Ctrl Pts',(-30.5643728486618,-8.4439522552059,144.21351409447));
#38806=CARTESIAN_POINT('Ctrl Pts',(-30.6753972898983,-8.46431943599457,
144.168549294019));
#38807=CARTESIAN_POINT('Ctrl Pts',(-30.7309095105166,-8.4745030263889,144.146066893794));
#38808=CARTESIAN_POINT('Ctrl Pts',(-30.7857148569115,-8.48339882987693,
144.120599544504));
#38809=CARTESIAN_POINT('Ctrl Pts',(-30.8389884141093,-8.4897730732797,144.092537510857));
#38810=CARTESIAN_POINT('Ctrl Pts',(-30.8922619713072,-8.49614731668247,
144.064475477209));
#38811=CARTESIAN_POINT('Ctrl Pts',(-30.9440037393079,-8.5,144.033818759205));
#38812=CARTESIAN_POINT('Ctrl Pts',(-30.9949874371066,-8.5,144.));
#38813=CARTESIAN_POINT('',(-28.8951880620293,-8.5,143.921052631579));
#38814=CARTESIAN_POINT('Ctrl Pts',(-28.8951880620293,-8.5,143.921052631579));
#38815=CARTESIAN_POINT('Ctrl Pts',(-28.9307900499921,-8.5,143.948731762135));
#38816=CARTESIAN_POINT('Ctrl Pts',(-28.9674326867105,-8.5,143.975072330207));
#38817=CARTESIAN_POINT('Ctrl Pts',(-29.0050125628934,-8.5,144.));
#38818=CARTESIAN_POINT('Origin',(-30.,-8.5,142.5));
#38819=CARTESIAN_POINT('Origin',(-37.95,-8.45,137.8));
#38820=CARTESIAN_POINT('',(-37.9,-8.4,144.));
#38821=CARTESIAN_POINT('',(-38.,-8.5,144.));
#38822=CARTESIAN_POINT('',(-37.9,-8.4,136.));
#38823=CARTESIAN_POINT('',(-37.9,-8.4,137.8));
#38824=CARTESIAN_POINT('',(-37.9,-8.4,136.));
#38825=CARTESIAN_POINT('Origin',(-37.95,-8.,144.));
#38826=CARTESIAN_POINT('',(-37.9,-8.,144.4));
#38827=CARTESIAN_POINT('',(-38.,-8.,144.5));
#38828=CARTESIAN_POINT('Origin',(-37.9,-8.,144.));
#38829=CARTESIAN_POINT('Origin',(-37.95,-7.45,144.45));
#38830=CARTESIAN_POINT('',(-37.9,-5.,144.4));
#38831=CARTESIAN_POINT('',(-38.,-5.,144.5));
#38832=CARTESIAN_POINT('',(-37.9,-7.45,144.4));
#38833=CARTESIAN_POINT('Origin',(-37.95,-5.,144.));
#38834=CARTESIAN_POINT('',(-38.,-4.50000000000002,144.));
#38835=CARTESIAN_POINT('Origin',(-37.9,-5.,144.));
#38836=CARTESIAN_POINT('Origin',(-37.95,-4.55,142.2));
#38837=CARTESIAN_POINT('',(-38.,-4.5,136.));
#38838=CARTESIAN_POINT('Origin',(-37.95,-5.,136.));
#38839=CARTESIAN_POINT('',(-37.9,-5.,135.6));
#38840=CARTESIAN_POINT('',(-38.,-5.,135.5));
#38841=CARTESIAN_POINT('Origin',(-37.9,-5.,136.));
#38842=CARTESIAN_POINT('Origin',(-37.95,-5.55,135.55));
#38843=CARTESIAN_POINT('',(-37.9,-8.,135.6));
#38844=CARTESIAN_POINT('',(-38.,-8.,135.5));
#38845=CARTESIAN_POINT('',(-37.9,-5.55,135.6));
#38846=CARTESIAN_POINT('Origin',(-37.95,-8.,136.));
#38847=CARTESIAN_POINT('Origin',(-37.9,-8.,136.));
#38848=CARTESIAN_POINT('Origin',(-38.,-5.,136.));
#38849=CARTESIAN_POINT('',(37.9,-5.,135.6));
#38850=CARTESIAN_POINT('',(-38.,-5.,135.6));
#38851=CARTESIAN_POINT('Origin',(37.9,-5.,136.));
#38852=CARTESIAN_POINT('Origin',(-38.,-4.6,135.6));
#38853=CARTESIAN_POINT('',(37.9,-8.,135.6));
#38854=CARTESIAN_POINT('',(-38.,-8.,135.6));
#38855=CARTESIAN_POINT('',(37.9,-5.55,135.6));
#38856=CARTESIAN_POINT('Origin',(-38.,-8.,136.));
#38857=CARTESIAN_POINT('',(-31.1661903789691,-8.4,136.));
#38858=CARTESIAN_POINT('',(-38.,-8.4,136.));
#38859=CARTESIAN_POINT('',(-31.0500544632573,-8.39129047171135,135.916983334517));
#38860=CARTESIAN_POINT('Ctrl Pts',(-31.0500544632573,-8.39129047171135,
135.916983334517));
#38861=CARTESIAN_POINT('Ctrl Pts',(-31.0899798045429,-8.39678689624297,
135.942890163407));
#38862=CARTESIAN_POINT('Ctrl Pts',(-31.1286105027861,-8.4,135.970783139968));
#38863=CARTESIAN_POINT('Ctrl Pts',(-31.166190378969,-8.4,136.));
#38864=CARTESIAN_POINT('',(-30.6614250203353,-8.29999999989176,135.735424868771));
#38865=CARTESIAN_POINT('Ctrl Pts',(-30.6618330135182,-8.30010233118054,
135.73532232755));
#38866=CARTESIAN_POINT('Ctrl Pts',(-30.7752047623485,-8.33157740613288,
135.770950841461));
#38867=CARTESIAN_POINT('Ctrl Pts',(-30.884493794383,-8.3621158090145,135.818341931664));
#38868=CARTESIAN_POINT('Ctrl Pts',(-30.9900545348086,-8.38157398223887,
135.880001956661));
#38869=CARTESIAN_POINT('Ctrl Pts',(-31.0016998407262,-8.38372057934385,
135.886804200101));
#38870=CARTESIAN_POINT('Ctrl Pts',(-31.013252101184,-8.38570733772648,135.893774692507));
#38871=CARTESIAN_POINT('Ctrl Pts',(-31.024762336812,-8.38753570208381,135.900923965067));
#38872=CARTESIAN_POINT('Ctrl Pts',(-31.0332270288628,-8.3888802915207,135.906181580337));
#38873=CARTESIAN_POINT('Ctrl Pts',(-31.0416572725171,-8.39013445090618,
135.911534549944));
#38874=CARTESIAN_POINT('Ctrl Pts',(-31.0500544632573,-8.39129047171137,
135.916983334517));
#38875=CARTESIAN_POINT('',(-29.338574981678,-8.29999999933447,135.735424868139));
#38876=CARTESIAN_POINT('Ctrl Pts',(-29.3385596675635,-8.29990288566524,
135.735450246581));
#38877=CARTESIAN_POINT('Ctrl Pts',(-29.4711775868139,-8.26307573905372,
135.693849975405));
#38878=CARTESIAN_POINT('Ctrl Pts',(-29.611005553036,-8.22475878909839,135.667443669536));
#38879=CARTESIAN_POINT('Ctrl Pts',(-29.7931525647518,-8.19595429131125,
135.651012005817));
#38880=CARTESIAN_POINT('Ctrl Pts',(-29.8314984033175,-8.19115568892357,
135.648342005979));
#38881=CARTESIAN_POINT('Ctrl Pts',(-29.9227100335579,-8.1831020607658,135.644103777034));
#38882=CARTESIAN_POINT('Ctrl Pts',(-29.9758741206228,-8.181174644247,135.64315190657));
#38883=CARTESIAN_POINT('Ctrl Pts',(-30.0416997940909,-8.18248038026117,
135.64382121028));
#38884=CARTESIAN_POINT('Ctrl Pts',(-30.0543921192683,-8.18289720095008,
135.644034674493));
#38885=CARTESIAN_POINT('Ctrl Pts',(-30.0933973998097,-8.18468277370442,
135.644958149228));
#38886=CARTESIAN_POINT('Ctrl Pts',(-30.1195781812265,-8.18659342326112,
135.64594828709));
#38887=CARTESIAN_POINT('Ctrl Pts',(-30.222494885632,-8.19662294325124,135.651344091598));
#38888=CARTESIAN_POINT('Ctrl Pts',(-30.3995380489843,-8.22753019248229,
135.668504490131));
#38889=CARTESIAN_POINT('Ctrl Pts',(-30.5675222793608,-8.27391945427504,
135.705706123533));
#38890=CARTESIAN_POINT('Ctrl Pts',(-30.6614853063865,-8.30000579887016,
135.73521309706));
#38891=CARTESIAN_POINT('',(-28.9499455367427,-8.39129047171135,135.916983334517));
#38892=CARTESIAN_POINT('Ctrl Pts',(-28.9499455367427,-8.39129047171135,
135.916983334517));
#38893=CARTESIAN_POINT('Ctrl Pts',(-29.0091684344659,-8.38313739956724,
135.878554671711));
#38894=CARTESIAN_POINT('Ctrl Pts',(-29.1339653847047,-8.35700091284832,
135.8092868271));
#38895=CARTESIAN_POINT('Ctrl Pts',(-29.2681120801237,-8.31946572940262,
135.757548608233));
#38896=CARTESIAN_POINT('Ctrl Pts',(-29.3385596675635,-8.29990288566524,
135.735450246581));
#38897=CARTESIAN_POINT('',(-28.9245839795016,-8.39448466110874,135.933804440104));
#38898=CARTESIAN_POINT('Ctrl Pts',(-28.9245903551729,-8.3944848309362,135.933813086825));
#38899=CARTESIAN_POINT('Ctrl Pts',(-28.9329848414562,-8.39352977637814,
135.928117215014));
#38900=CARTESIAN_POINT('Ctrl Pts',(-28.9414357816817,-8.39246198897255,
135.922505160033));
#38901=CARTESIAN_POINT('Ctrl Pts',(-28.9499455367427,-8.39129047171135,
135.916983334517));
#38902=CARTESIAN_POINT('',(-28.8338096210309,-8.4,136.));
#38903=CARTESIAN_POINT('Ctrl Pts',(-28.8338096210309,-8.4,136.));
#38904=CARTESIAN_POINT('Ctrl Pts',(-28.8633796585678,-8.39999999999971,
135.977010471143));
#38905=CARTESIAN_POINT('Ctrl Pts',(-28.8936003083676,-8.39801061970484,
135.954840619426));
#38906=CARTESIAN_POINT('Ctrl Pts',(-28.9245903551729,-8.3944848309362,135.933813086825));
#38907=CARTESIAN_POINT('',(28.8338096210309,-8.4,136.));
#38908=CARTESIAN_POINT('',(-38.,-8.4,136.));
#38909=CARTESIAN_POINT('',(28.9499455367427,-8.39129047171135,135.916983334517));
#38910=CARTESIAN_POINT('Ctrl Pts',(28.9499455367427,-8.39129047171135,135.916983334517));
#38911=CARTESIAN_POINT('Ctrl Pts',(28.9100201954571,-8.39678689624297,135.942890163407));
#38912=CARTESIAN_POINT('Ctrl Pts',(28.8713894972139,-8.4,135.970783139968));
#38913=CARTESIAN_POINT('Ctrl Pts',(28.833809621031,-8.4,136.));
#38914=CARTESIAN_POINT('',(29.3385749796647,-8.29999999989174,135.735424868771));
#38915=CARTESIAN_POINT('Ctrl Pts',(29.3382719538198,-8.30022274522941,135.735429427059));
#38916=CARTESIAN_POINT('Ctrl Pts',(29.2248680044857,-8.33165798240388,135.771014610257));
#38917=CARTESIAN_POINT('Ctrl Pts',(29.1154899444758,-8.36206527659851,135.81832752607));
#38918=CARTESIAN_POINT('Ctrl Pts',(29.009946342934,-8.3815714458719,135.880001863018));
#38919=CARTESIAN_POINT('Ctrl Pts',(28.9983029277528,-8.38372333783055,135.886805685331));
#38920=CARTESIAN_POINT('Ctrl Pts',(28.9867484811824,-8.38570649135595,135.893774768811));
#38921=CARTESIAN_POINT('Ctrl Pts',(28.9752381881508,-8.38753539124472,135.900924108674));
#38922=CARTESIAN_POINT('Ctrl Pts',(28.966773453885,-8.38888037451444,135.90618177344));
#38923=CARTESIAN_POINT('Ctrl Pts',(28.9583427274828,-8.39013445090615,135.911534549944));
#38924=CARTESIAN_POINT('Ctrl Pts',(28.9499455367427,-8.39129047171135,135.916983334517));
#38925=CARTESIAN_POINT('',(30.6614250183219,-8.29999999933448,135.735424868139));
#38926=CARTESIAN_POINT('Ctrl Pts',(30.661439935235,-8.29988734177344,135.735464277796));
#38927=CARTESIAN_POINT('Ctrl Pts',(30.4942644053416,-8.25334841832887,135.683085800293));
#38928=CARTESIAN_POINT('Ctrl Pts',(30.3161740152865,-8.20438420621798,135.655279343636));
#38929=CARTESIAN_POINT('Ctrl Pts',(30.0774858946058,-8.1831094502482,135.644290152174));
#38930=CARTESIAN_POINT('Ctrl Pts',(30.0242680337758,-8.18121722147009,135.643309689515));
#38931=CARTESIAN_POINT('Ctrl Pts',(29.9584452353951,-8.1825139216413,135.643982887837));
#38932=CARTESIAN_POINT('Ctrl Pts',(29.9457556588889,-8.18293453051425,135.644194467675));
#38933=CARTESIAN_POINT('Ctrl Pts',(29.8489117254301,-8.18734058685009,135.646496412784));
#38934=CARTESIAN_POINT('Ctrl Pts',(29.6834526291903,-8.20996395514133,135.657893063385));
#38935=CARTESIAN_POINT('Ctrl Pts',(29.4880416126676,-8.25873808016239,135.692585803548));
#38936=CARTESIAN_POINT('Ctrl Pts',(29.3751527057733,-8.28999956547834,135.723864269662));
#38937=CARTESIAN_POINT('Ctrl Pts',(29.3385835586903,-8.30013636951601,135.735331680823));
#38938=CARTESIAN_POINT('',(31.0500544632573,-8.39129047171135,135.916983334517));
#38939=CARTESIAN_POINT('Ctrl Pts',(31.0500544632573,-8.39129047171135,135.916983334517));
#38940=CARTESIAN_POINT('Ctrl Pts',(31.0166500895793,-8.38669177291417,135.895307843082));
#38941=CARTESIAN_POINT('Ctrl Pts',(30.9494673877353,-8.37449857575747,135.855365180714));
#38942=CARTESIAN_POINT('Ctrl Pts',(30.8206580127449,-8.34434635533052,135.791526200842));
#38943=CARTESIAN_POINT('Ctrl Pts',(30.7231771409772,-8.31707396647592,135.754807424752));
#38944=CARTESIAN_POINT('Ctrl Pts',(30.661439935235,-8.29988734177344,135.735464277796));
#38945=CARTESIAN_POINT('',(31.0754160204892,-8.3944846611077,135.933804440098));
#38946=CARTESIAN_POINT('Ctrl Pts',(31.0754096448179,-8.39448483093516,135.933813086818));
#38947=CARTESIAN_POINT('Ctrl Pts',(31.0670151585377,-8.39352977637736,135.92811721501));
#38948=CARTESIAN_POINT('Ctrl Pts',(31.0585642183152,-8.39246198897212,135.922505160031));
#38949=CARTESIAN_POINT('Ctrl Pts',(31.0500544632573,-8.39129047171135,135.916983334517));
#38950=CARTESIAN_POINT('',(31.1661903789691,-8.4,136.));
#38951=CARTESIAN_POINT('Ctrl Pts',(31.1661903789691,-8.4,136.));
#38952=CARTESIAN_POINT('Ctrl Pts',(31.1366203414292,-8.39999999999971,135.977010471141));
#38953=CARTESIAN_POINT('Ctrl Pts',(31.1063996916264,-8.39801061970445,135.954840619422));
#38954=CARTESIAN_POINT('Ctrl Pts',(31.0754096448179,-8.39448483093516,135.933813086818));
#38955=CARTESIAN_POINT('',(37.9,-8.4,136.));
#38956=CARTESIAN_POINT('',(-38.,-8.4,136.));
#38957=CARTESIAN_POINT('Origin',(37.9,-8.,136.));
#38958=CARTESIAN_POINT('Origin',(-38.,-8.4,135.6));
#38959=CARTESIAN_POINT('',(-31.1661903789691,-8.4,144.));
#38960=CARTESIAN_POINT('',(-38.,-8.4,144.));
#38961=CARTESIAN_POINT('',(-28.8338096210309,-8.4,144.));
#38962=CARTESIAN_POINT('Origin',(-30.,-8.4,142.5));
#38963=CARTESIAN_POINT('',(28.8338096210309,-8.4,144.));
#38964=CARTESIAN_POINT('',(-38.,-8.4,144.));
#38965=CARTESIAN_POINT('',(31.1661903789691,-8.4,144.));
#38966=CARTESIAN_POINT('Origin',(30.,-8.4,142.5));
#38967=CARTESIAN_POINT('',(37.9,-8.4,144.));
#38968=CARTESIAN_POINT('',(-38.,-8.4,144.));
#38969=CARTESIAN_POINT('',(37.9,-8.4,137.8));
#38970=CARTESIAN_POINT('Origin',(30.,-8.4,137.5));
#38971=CARTESIAN_POINT('Origin',(-30.,-8.4,137.5));
#38972=CARTESIAN_POINT('Ctrl Pts',(-31.0500544632573,-8.39129047171135,
135.916983334517));
#38973=CARTESIAN_POINT('Ctrl Pts',(-31.0416572725172,-8.39013445090615,
135.911534549944));
#38974=CARTESIAN_POINT('Ctrl Pts',(-31.0332270288628,-8.38888029152067,
135.906181580337));
#38975=CARTESIAN_POINT('Ctrl Pts',(-31.013252101184,-8.38570733772645,135.893774692507));
#38976=CARTESIAN_POINT('Ctrl Pts',(-31.0016998407262,-8.38372057934382,
135.8868042001));
#38977=CARTESIAN_POINT('Ctrl Pts',(-30.7969030955286,-8.34597008112092,
135.767178547824));
#38978=CARTESIAN_POINT('Ctrl Pts',(-30.522724535098,-8.24903543084407,135.680444681186));
#38979=CARTESIAN_POINT('Ctrl Pts',(-30.222494885632,-8.19662294325124,135.651344091598));
#38980=CARTESIAN_POINT('Ctrl Pts',(-30.1195781812265,-8.18659342326112,
135.64594828709));
#38981=CARTESIAN_POINT('Ctrl Pts',(-30.0933973998097,-8.18468277370442,
135.644958149228));
#38982=CARTESIAN_POINT('Ctrl Pts',(-30.0543921192683,-8.18289720095008,
135.644034674493));
#38983=CARTESIAN_POINT('Ctrl Pts',(-30.0416997940909,-8.18248038026117,
135.64382121028));
#38984=CARTESIAN_POINT('Ctrl Pts',(-29.9758741206228,-8.181174644247,135.64315190657));
#38985=CARTESIAN_POINT('Ctrl Pts',(-29.9227100335579,-8.1831020607658,135.644103777034));
#38986=CARTESIAN_POINT('Ctrl Pts',(-29.8314984033175,-8.19115568892357,
135.648342005979));
#38987=CARTESIAN_POINT('Ctrl Pts',(-29.7931525647518,-8.19595429131125,
135.651012005817));
#38988=CARTESIAN_POINT('Ctrl Pts',(-29.5343055319322,-8.23688803331351,
135.67436285499));
#38989=CARTESIAN_POINT('Ctrl Pts',(-29.2537770277665,-8.33190850945494,
135.742786049171));
#38990=CARTESIAN_POINT('Ctrl Pts',(-29.0091684344659,-8.38313739956724,
135.878554671711));
#38991=CARTESIAN_POINT('Ctrl Pts',(-28.9499455367427,-8.39129047171135,
135.916983334517));
#38992=CARTESIAN_POINT('Ctrl Pts',(-31.0316987878737,-8.4275269811409,135.944655556345));
#38993=CARTESIAN_POINT('Ctrl Pts',(-31.0232517541167,-8.42675447068797,
135.939129772415));
#38994=CARTESIAN_POINT('Ctrl Pts',(-31.0147571834097,-8.42588545326909,
135.933697780808));
#38995=CARTESIAN_POINT('Ctrl Pts',(-30.9946844630235,-8.42359293603059,
135.921096409853));
#38996=CARTESIAN_POINT('Ctrl Pts',(-30.9830404840594,-8.42211931541815,
135.914010922128));
#38997=CARTESIAN_POINT('Ctrl Pts',(-30.7774143949989,-8.39302212150258,
135.792260131074));
#38998=CARTESIAN_POINT('Ctrl Pts',(-30.5031878030179,-8.3040138295315,135.701370817207));
#38999=CARTESIAN_POINT('Ctrl Pts',(-30.2129394147106,-8.25623003142082,
135.670553593881));
#39000=CARTESIAN_POINT('Ctrl Pts',(-30.1143200141462,-8.24706050714476,
135.66484117304));
#39001=CARTESIAN_POINT('Ctrl Pts',(-30.0892414365264,-8.24533390764359,
135.663791948758));
#39002=CARTESIAN_POINT('Ctrl Pts',(-30.0519718185279,-8.24370245708564,
135.662813622192));
#39003=CARTESIAN_POINT('Ctrl Pts',(-30.0398405940584,-8.24332623806909,
135.662587713749));
#39004=CARTESIAN_POINT('Ctrl Pts',(-29.9769739071425,-8.24213517042753,
135.66187745256));
#39005=CARTESIAN_POINT('Ctrl Pts',(-29.9262337381129,-8.24389460327267,
135.662889336926));
#39006=CARTESIAN_POINT('Ctrl Pts',(-29.8388361258893,-8.25121736432484,
135.667375770243));
#39007=CARTESIAN_POINT('Ctrl Pts',(-29.8019759732395,-8.25561494071629,
135.670207472664));
#39008=CARTESIAN_POINT('Ctrl Pts',(-29.552197652623,-8.29287747645484,135.69488233382));
#39009=CARTESIAN_POINT('Ctrl Pts',(-29.2735131217218,-8.38080329713423,
135.767194847034));
#39010=CARTESIAN_POINT('Ctrl Pts',(-29.0279258537172,-8.42207265865228,
135.90569558041));
#39011=CARTESIAN_POINT('Ctrl Pts',(-28.9683012121262,-8.4275269811409,135.944655556345));
#39012=CARTESIAN_POINT('Ctrl Pts',(-31.0133431124902,-8.46376349057045,
135.972327778172));
#39013=CARTESIAN_POINT('Ctrl Pts',(-31.0048313249904,-8.46337998021818,
135.966725634326));
#39014=CARTESIAN_POINT('Ctrl Pts',(-30.996307968523,-8.46288297234629,135.961213070326));
#39015=CARTESIAN_POINT('Ctrl Pts',(-30.9760819259681,-8.46149122158306,
135.948419567118));
#39016=CARTESIAN_POINT('Ctrl Pts',(-30.9644219148336,-8.46050386249282,
135.941215807521));
#39017=CARTESIAN_POINT('Ctrl Pts',(-30.7577276599546,-8.44008395869097,
135.817350883126));
#39018=CARTESIAN_POINT('Ctrl Pts',(-30.4835228973095,-8.3590711140171,135.722284002991));
#39019=CARTESIAN_POINT('Ctrl Pts',(-30.2034244047578,-8.31578082809446,
135.6897528233));
#39020=CARTESIAN_POINT('Ctrl Pts',(-30.1089398725528,-8.30755126516961,
135.683719880602));
#39021=CARTESIAN_POINT('Ctrl Pts',(-30.0850294746744,-8.30597389738886,
135.682612214976));
#39022=CARTESIAN_POINT('Ctrl Pts',(-30.0494583878705,-8.30451621696662,
135.681578940764));
#39023=CARTESIAN_POINT('Ctrl Pts',(-30.0379032525606,-8.30417201489962,
135.681339763716));
#39024=CARTESIAN_POINT('Ctrl Pts',(-29.9779830147398,-8.30310560712257,
135.68059196657));
#39025=CARTESIAN_POINT('Ctrl Pts',(-29.9296772515286,-8.30467251192379,
135.681655985758));
#39026=CARTESIAN_POINT('Ctrl Pts',(-29.846092258766,-8.31129493668671,135.686399274144));
#39027=CARTESIAN_POINT('Ctrl Pts',(-29.8107266215916,-8.31524006098973,
135.689377589036));
#39028=CARTESIAN_POINT('Ctrl Pts',(-29.5699143091109,-8.34907703619935,
135.71544499358));
#39029=CARTESIAN_POINT('Ctrl Pts',(-29.2933633974204,-8.42964542252681,
135.791591053793));
#39030=CARTESIAN_POINT('Ctrl Pts',(-29.0466377863763,-8.46106474091497,
135.93280577734));
#39031=CARTESIAN_POINT('Ctrl Pts',(-28.9866568875098,-8.46376349057045,
135.972327778172));
#39032=CARTESIAN_POINT('Ctrl Pts',(-30.9949874371066,-8.5,136.));
#39033=CARTESIAN_POINT('Ctrl Pts',(-30.9864258065899,-8.5,135.994320856796));
#39034=CARTESIAN_POINT('Ctrl Pts',(-30.9778381230699,-8.4998881340947,135.988729270797));
#39035=CARTESIAN_POINT('Ctrl Pts',(-30.9575142878075,-8.4993768198872,135.975741284465));
#39036=CARTESIAN_POINT('Ctrl Pts',(-30.9457625581667,-8.49890259856716,
135.968422529549));
#39037=CARTESIAN_POINT('Ctrl Pts',(-30.7382389594249,-8.48713599907263,
135.842432466377));
#39038=CARTESIAN_POINT('Ctrl Pts',(-30.4639861652294,-8.41404951270454,
135.743210139011));
#39039=CARTESIAN_POINT('Ctrl Pts',(-30.1938689338364,-8.37538791626404,
135.708962325583));
#39040=CARTESIAN_POINT('Ctrl Pts',(-30.1036817054724,-8.36801834905326,
135.702612766552));
#39041=CARTESIAN_POINT('Ctrl Pts',(-30.0808735113911,-8.36662503132804,
135.701446014506));
#39042=CARTESIAN_POINT('Ctrl Pts',(-30.0470380871301,-8.36532147310218,
135.700357888462));
#39043=CARTESIAN_POINT('Ctrl Pts',(-30.0360440525282,-8.36501787270754,
135.700106267186));
#39044=CARTESIAN_POINT('Ctrl Pts',(-29.9790828012595,-8.3640661333031,135.699317512559));
#39045=CARTESIAN_POINT('Ctrl Pts',(-29.9332009560837,-8.36546505443066,
135.700441545649));
#39046=CARTESIAN_POINT('Ctrl Pts',(-29.8534299813378,-8.37135661208798,
135.705433038408));
#39047=CARTESIAN_POINT('Ctrl Pts',(-29.8195500300793,-8.37490071039478,
135.708573055883));
#39048=CARTESIAN_POINT('Ctrl Pts',(-29.5878064298017,-8.40506647934067,
135.73596447241));
#39049=CARTESIAN_POINT('Ctrl Pts',(-29.3130994913757,-8.4785402102061,135.815999851656));
#39050=CARTESIAN_POINT('Ctrl Pts',(-29.0653952056276,-8.5,135.95994668604));
#39051=CARTESIAN_POINT('Ctrl Pts',(-29.0050125628934,-8.5,136.));
#39052=CARTESIAN_POINT('',(-31.0500544632573,-8.39129047171135,135.916983334517));
#39053=CARTESIAN_POINT('',(-29.0050125628934,-8.5,136.));
#39054=CARTESIAN_POINT('Origin',(-30.,-8.45,137.5));
#39055=CARTESIAN_POINT('',(-28.8338096210309,-8.4,136.));
#39056=CARTESIAN_POINT('',(-31.1048119379707,-8.5,136.078947368421));
#39057=CARTESIAN_POINT('Ctrl Pts',(-28.9499455367427,-8.39129047171135,
135.916983334517));
#39058=CARTESIAN_POINT('Ctrl Pts',(-28.9100201948423,-8.39678689632762,
135.942890163806));
#39059=CARTESIAN_POINT('Ctrl Pts',(-28.8713894960226,-8.40000000009859,
135.970783140825));
#39060=CARTESIAN_POINT('Ctrl Pts',(-28.8338096192947,-8.4,136.00000000135));
#39061=CARTESIAN_POINT('Ctrl Pts',(-28.9683012121262,-8.4275269811409,135.944655556345));
#39062=CARTESIAN_POINT('Ctrl Pts',(-28.9291576919387,-8.43119126421841,
135.970235999263));
#39063=CARTESIAN_POINT('Ctrl Pts',(-28.8911896803029,-8.43333333339906,
135.997611506775));
#39064=CARTESIAN_POINT('Ctrl Pts',(-28.854269099658,-8.43333333333333,136.0263157908));
#39065=CARTESIAN_POINT('Ctrl Pts',(-28.9866568875098,-8.46376349057045,
135.972327778172));
#39066=CARTESIAN_POINT('Ctrl Pts',(-28.9482951890352,-8.46559563210921,
135.99758183472));
#39067=CARTESIAN_POINT('Ctrl Pts',(-28.9109898645832,-8.46666666669953,
136.024439872726));
#39068=CARTESIAN_POINT('Ctrl Pts',(-28.8747285800212,-8.46666666666667,
136.05263158025));
#39069=CARTESIAN_POINT('Ctrl Pts',(-29.0050125628934,-8.5,136.));
#39070=CARTESIAN_POINT('Ctrl Pts',(-28.9674326861317,-8.5,136.024927670177));
#39071=CARTESIAN_POINT('Ctrl Pts',(-28.9307900488635,-8.5,136.051268238676));
#39072=CARTESIAN_POINT('Ctrl Pts',(-28.8951880603845,-8.5,136.0789473697));
#39073=CARTESIAN_POINT('Ctrl Pts',(-31.166190378969,-8.4,136.));
#39074=CARTESIAN_POINT('Ctrl Pts',(-31.1286105027861,-8.4,135.970783139968));
#39075=CARTESIAN_POINT('Ctrl Pts',(-31.0899798045429,-8.39678689624297,
135.942890163407));
#39076=CARTESIAN_POINT('Ctrl Pts',(-31.0500544632573,-8.39129047171135,
135.916983334517));
#39077=CARTESIAN_POINT('Ctrl Pts',(-31.1457308986363,-8.43333333333333,
136.026315789474));
#39078=CARTESIAN_POINT('Ctrl Pts',(-31.1088103185267,-8.43333333333333,
135.997611505934));
#39079=CARTESIAN_POINT('Ctrl Pts',(-31.0708423074584,-8.43119126416198,
135.970235998869));
#39080=CARTESIAN_POINT('Ctrl Pts',(-31.0316987878737,-8.4275269811409,135.944655556345));
#39081=CARTESIAN_POINT('Ctrl Pts',(-31.1252714183035,-8.46666666666667,
136.052631578947));
#39082=CARTESIAN_POINT('Ctrl Pts',(-31.0890101342673,-8.46666666666667,
136.024439871899));
#39083=CARTESIAN_POINT('Ctrl Pts',(-31.051704810374,-8.46559563208099,135.997581834331));
#39084=CARTESIAN_POINT('Ctrl Pts',(-31.0133431124902,-8.46376349057045,
135.972327778172));
#39085=CARTESIAN_POINT('Ctrl Pts',(-31.1048119379707,-8.5,136.078947368421));
#39086=CARTESIAN_POINT('Ctrl Pts',(-31.0692099500079,-8.5,136.051268237865));
#39087=CARTESIAN_POINT('Ctrl Pts',(-31.0325673132895,-8.5,136.024927669793));
#39088=CARTESIAN_POINT('Ctrl Pts',(-30.9949874371066,-8.5,136.));
#39089=CARTESIAN_POINT('Origin',(37.95,-8.45,137.8));
#39090=CARTESIAN_POINT('',(37.9,-8.4,144.));
#39091=CARTESIAN_POINT('',(38.,-8.5,136.));
#39092=CARTESIAN_POINT('Origin',(37.95,-8.,144.));
#39093=CARTESIAN_POINT('',(37.9,-8.,144.4));
#39094=CARTESIAN_POINT('Origin',(37.9,-8.,144.));
#39095=CARTESIAN_POINT('',(37.9,-8.,144.4));
#39096=CARTESIAN_POINT('Origin',(37.95,-7.45,144.45));
#39097=CARTESIAN_POINT('',(37.9,-5.,144.4));
#39098=CARTESIAN_POINT('',(37.9,-5.,144.4));
#39099=CARTESIAN_POINT('',(37.9,-7.45,144.4));
#39100=CARTESIAN_POINT('Origin',(37.95,-5.,144.));
#39101=CARTESIAN_POINT('Origin',(37.9,-5.,144.));
#39102=CARTESIAN_POINT('',(37.9,-4.6,144.));
#39103=CARTESIAN_POINT('Origin',(37.95,-4.55,142.2));
#39104=CARTESIAN_POINT('',(37.9,-4.6,136.));
#39105=CARTESIAN_POINT('Origin',(37.95,-5.,136.));
#39106=CARTESIAN_POINT('',(37.9,-5.,135.6));
#39107=CARTESIAN_POINT('Origin',(37.95,-5.55,135.55));
#39108=CARTESIAN_POINT('',(37.9,-8.,135.6));
#39109=CARTESIAN_POINT('Origin',(37.95,-8.,136.));
#39110=CARTESIAN_POINT('Origin',(-38.,-5.,144.));
#39111=CARTESIAN_POINT('',(-38.,-5.,144.4));
#39112=CARTESIAN_POINT('Origin',(-38.,-8.4,144.4));
#39113=CARTESIAN_POINT('',(-38.,-8.,144.4));
#39114=CARTESIAN_POINT('Origin',(-38.,-8.,144.));
#39115=CARTESIAN_POINT('',(31.0500544632573,-8.39129047171135,144.083016665483));
#39116=CARTESIAN_POINT('Ctrl Pts',(31.0500544632573,-8.39129047171134,144.083016665483));
#39117=CARTESIAN_POINT('Ctrl Pts',(31.0899798045429,-8.39678689624297,144.057109836593));
#39118=CARTESIAN_POINT('Ctrl Pts',(31.1286105027861,-8.4,144.029216860032));
#39119=CARTESIAN_POINT('Ctrl Pts',(31.166190378969,-8.4,144.));
#39120=CARTESIAN_POINT('',(30.6614250203353,-8.29999999989175,144.264575131229));
#39121=CARTESIAN_POINT('Ctrl Pts',(30.6618125705925,-8.30021236907056,144.264595259035));
#39122=CARTESIAN_POINT('Ctrl Pts',(30.7752011548794,-8.33164973325584,144.228998875671));
#39123=CARTESIAN_POINT('Ctrl Pts',(30.8844471797781,-8.36205371033993,144.18170673564));
#39124=CARTESIAN_POINT('Ctrl Pts',(30.990050453113,-8.38157059509137,144.120000581026));
#39125=CARTESIAN_POINT('Ctrl Pts',(31.0017004511988,-8.38372366916582,144.113193248635));
#39126=CARTESIAN_POINT('Ctrl Pts',(31.0132504414343,-8.38570616125813,144.106226170536));
#39127=CARTESIAN_POINT('Ctrl Pts',(31.0247614073442,-8.38753522038424,144.099076369329));
#39128=CARTESIAN_POINT('Ctrl Pts',(31.0332266364484,-8.38888032075799,144.093818365289));
#39129=CARTESIAN_POINT('Ctrl Pts',(31.0416572725171,-8.39013445090616,144.088465450056));
#39130=CARTESIAN_POINT('Ctrl Pts',(31.0500544632573,-8.39129047171136,144.083016665483));
#39131=CARTESIAN_POINT('',(29.338574981678,-8.29999999933449,144.264575131861));
#39132=CARTESIAN_POINT('Ctrl Pts',(29.3385708495646,-8.29992765643484,144.264531198596));
#39133=CARTESIAN_POINT('Ctrl Pts',(29.4712387553426,-8.2631077339495,144.306139218458));
#39134=CARTESIAN_POINT('Ctrl Pts',(29.61111819365,-8.22479704106424,144.332544752617));
#39135=CARTESIAN_POINT('Ctrl Pts',(29.7743380762458,-8.1989686017083,144.347220946225));
#39136=CARTESIAN_POINT('Ctrl Pts',(29.8124450528999,-8.19359284366967,144.350292014722));
#39137=CARTESIAN_POINT('Ctrl Pts',(29.8508694789328,-8.18947694445684,144.352489515548));
#39138=CARTESIAN_POINT('Ctrl Pts',(29.8965215329261,-8.18546023959715,144.35462295684));
#39139=CARTESIAN_POINT('Ctrl Pts',(29.949327590037,-8.18215812697606,144.356319671809));
#39140=CARTESIAN_POINT('Ctrl Pts',(30.0025425983683,-8.18173837270729,144.356528098816));
#39141=CARTESIAN_POINT('Ctrl Pts',(30.0386195894541,-8.18245156556629,144.356161937062));
#39142=CARTESIAN_POINT('Ctrl Pts',(30.0513226380827,-8.18282772898188,144.355968145438));
#39143=CARTESIAN_POINT('Ctrl Pts',(30.0640055623709,-8.18336746578261,144.355691316105));
#39144=CARTESIAN_POINT('Ctrl Pts',(30.2356236626453,-8.19124684145658,144.351553122611));
#39145=CARTESIAN_POINT('Ctrl Pts',(30.4360870224364,-8.23769662979138,144.328510834346));
#39146=CARTESIAN_POINT('Ctrl Pts',(30.6248943138717,-8.28997674496655,144.276175839712));
#39147=CARTESIAN_POINT('Ctrl Pts',(30.6614381003711,-8.30010854638129,144.264712770237));
#39148=CARTESIAN_POINT('',(28.9499455367427,-8.39129047171135,144.083016665483));
#39149=CARTESIAN_POINT('Ctrl Pts',(28.9499455367427,-8.39129047171135,144.083016665483));
#39150=CARTESIAN_POINT('Ctrl Pts',(29.0091684344659,-8.38313739956724,144.121445328289));
#39151=CARTESIAN_POINT('Ctrl Pts',(29.1339413896373,-8.35700182937075,144.190695469215));
#39152=CARTESIAN_POINT('Ctrl Pts',(29.2681157510772,-8.31948137780997,144.242434692888));
#39153=CARTESIAN_POINT('Ctrl Pts',(29.3385708495646,-8.29992765643484,144.264531198596));
#39154=CARTESIAN_POINT('',(28.9245839794983,-8.39448466110912,144.066195559894));
#39155=CARTESIAN_POINT('Ctrl Pts',(28.9245903551696,-8.39448483093658,144.066186913173));
#39156=CARTESIAN_POINT('Ctrl Pts',(28.932984841454,-8.39352977637842,144.071882784984));
#39157=CARTESIAN_POINT('Ctrl Pts',(28.9414357816806,-8.39246198897271,144.077494839966));
#39158=CARTESIAN_POINT('Ctrl Pts',(28.9499455367427,-8.39129047171135,144.083016665483));
#39159=CARTESIAN_POINT('Ctrl Pts',(28.8338096210309,-8.4,144.));
#39160=CARTESIAN_POINT('Ctrl Pts',(28.8633796585668,-8.39999999999971,144.022989528856));
#39161=CARTESIAN_POINT('Ctrl Pts',(28.8936003083654,-8.39801061970499,144.045159380572));
#39162=CARTESIAN_POINT('Ctrl Pts',(28.9245903551696,-8.39448483093658,144.066186913173));
#39163=CARTESIAN_POINT('',(-28.9499455367427,-8.39129047171135,144.083016665483));
#39164=CARTESIAN_POINT('Ctrl Pts',(-28.9499455367427,-8.39129047171135,
144.083016665483));
#39165=CARTESIAN_POINT('Ctrl Pts',(-28.9100201954571,-8.39678689624297,
144.057109836593));
#39166=CARTESIAN_POINT('Ctrl Pts',(-28.8713894972139,-8.4,144.029216860032));
#39167=CARTESIAN_POINT('Ctrl Pts',(-28.833809621031,-8.4,144.));
#39168=CARTESIAN_POINT('',(-29.3385749796646,-8.29999999989175,144.264575131229));
#39169=CARTESIAN_POINT('Ctrl Pts',(-29.3383110933769,-8.30003007418734,
144.264639748776));
#39170=CARTESIAN_POINT('Ctrl Pts',(-29.2249006798342,-8.33151072678332,
144.229030421918));
#39171=CARTESIAN_POINT('Ctrl Pts',(-29.1155604606526,-8.36207385241182,
144.181653095174));
#39172=CARTESIAN_POINT('Ctrl Pts',(-29.009948502526,-8.38157138568459,144.119997209092));
#39173=CARTESIAN_POINT('Ctrl Pts',(-28.9982975463468,-8.38372232493232,
144.113195422252));
#39174=CARTESIAN_POINT('Ctrl Pts',(-28.9867489659987,-8.38570638741796,
144.10622492921));
#39175=CARTESIAN_POINT('Ctrl Pts',(-28.9752381128004,-8.38753526296663,
144.099075788646));
#39176=CARTESIAN_POINT('Ctrl Pts',(-28.9667729665849,-8.38888022833652,
144.093818270446));
#39177=CARTESIAN_POINT('Ctrl Pts',(-28.9583427274829,-8.39013445090614,
144.088465450056));
#39178=CARTESIAN_POINT('Ctrl Pts',(-28.9499455367427,-8.39129047171134,
144.083016665483));
#39179=CARTESIAN_POINT('',(-30.6614250183219,-8.29999999933447,144.264575131861));
#39180=CARTESIAN_POINT('Ctrl Pts',(-30.6614343690749,-8.30004553356604,
144.264645137541));
#39181=CARTESIAN_POINT('Ctrl Pts',(-30.5707184122875,-8.27491838180028,
144.293105800203));
#39182=CARTESIAN_POINT('Ctrl Pts',(-30.4769220075146,-8.24904042442226,
144.314236285244));
#39183=CARTESIAN_POINT('Ctrl Pts',(-30.3362573241971,-8.21797318024007,
144.335720743413));
#39184=CARTESIAN_POINT('Ctrl Pts',(-30.2909203211106,-8.20912670855604,
144.341198190437));
#39185=CARTESIAN_POINT('Ctrl Pts',(-30.2069857608087,-8.19595190722736,
144.348893235529));
#39186=CARTESIAN_POINT('Ctrl Pts',(-30.1687494835259,-8.19113640094687,
144.351508081756));
#39187=CARTESIAN_POINT('Ctrl Pts',(-30.0774739256815,-8.18309698929938,
144.355772172055));
#39188=CARTESIAN_POINT('Ctrl Pts',(-30.0243207374447,-8.18117200076953,
144.35671442715));
#39189=CARTESIAN_POINT('Ctrl Pts',(-29.9584929581617,-8.18247823187435,
144.356048044385));
#39190=CARTESIAN_POINT('Ctrl Pts',(-29.945800622645,-8.18289510415931,144.355834150072));
#39191=CARTESIAN_POINT('Ctrl Pts',(-29.9067939860508,-8.18468265252138,
144.354910990812));
#39192=CARTESIAN_POINT('Ctrl Pts',(-29.8806159996987,-8.18658920666495,
144.35392173636));
#39193=CARTESIAN_POINT('Ctrl Pts',(-29.7961080426536,-8.19484695032281,
144.349486882414));
#39194=CARTESIAN_POINT('Ctrl Pts',(-29.7387539667785,-8.2037212977524,144.344577795757));
#39195=CARTESIAN_POINT('Ctrl Pts',(-29.5636487905334,-8.23768920458241,
144.322949985584));
#39196=CARTESIAN_POINT('Ctrl Pts',(-29.4491527367723,-8.26926273488951,
144.29942619088));
#39197=CARTESIAN_POINT('Ctrl Pts',(-29.3385291537654,-8.29996954488366,
144.264708200695));
#39198=CARTESIAN_POINT('',(-31.0500544632573,-8.39129047171135,144.083016665483));
#39199=CARTESIAN_POINT('Ctrl Pts',(-31.0500544632573,-8.39129047171135,
144.083016665483));
#39200=CARTESIAN_POINT('Ctrl Pts',(-31.0000499887335,-8.38440647744572,
144.115463660888));
#39201=CARTESIAN_POINT('Ctrl Pts',(-30.8980141119118,-8.36393098595595,
144.173469870658));
#39202=CARTESIAN_POINT('Ctrl Pts',(-30.7654955980711,-8.32889312403532,
144.230056244874));
#39203=CARTESIAN_POINT('Ctrl Pts',(-30.6852039930454,-8.3066294132943,144.257187802874));
#39204=CARTESIAN_POINT('Ctrl Pts',(-30.6614343690749,-8.30004553356604,
144.264645137541));
#39205=CARTESIAN_POINT('',(-31.0754160204959,-8.39448466110846,144.066195559898));
#39206=CARTESIAN_POINT('Ctrl Pts',(-31.0754096448245,-8.39448483093591,
144.066186913177));
#39207=CARTESIAN_POINT('Ctrl Pts',(-31.0670151585421,-8.39352977637793,
144.071882784987));
#39208=CARTESIAN_POINT('Ctrl Pts',(-31.0585642183174,-8.39246198897244,
144.077494839967));
#39209=CARTESIAN_POINT('Ctrl Pts',(-31.0500544632573,-8.39129047171135,
144.083016665483));
#39210=CARTESIAN_POINT('Ctrl Pts',(-31.1661903789691,-8.4,144.));
#39211=CARTESIAN_POINT('Ctrl Pts',(-31.1366203414314,-8.3999999999997,144.022989528858));
#39212=CARTESIAN_POINT('Ctrl Pts',(-31.1063996916308,-8.39801061970473,
144.045159380575));
#39213=CARTESIAN_POINT('Ctrl Pts',(-31.0754096448245,-8.39448483093591,
144.066186913177));
#39214=CARTESIAN_POINT('Ctrl Pts',(31.0500544632573,-8.39129047171135,144.083016665483));
#39215=CARTESIAN_POINT('Ctrl Pts',(31.0416572725172,-8.39013445090615,144.088465450056));
#39216=CARTESIAN_POINT('Ctrl Pts',(31.0332266364484,-8.38888032075798,144.093818365289));
#39217=CARTESIAN_POINT('Ctrl Pts',(31.0132504414343,-8.38570616125812,144.106226170536));
#39218=CARTESIAN_POINT('Ctrl Pts',(31.0017004511988,-8.38372366916581,144.113193248635));
#39219=CARTESIAN_POINT('Ctrl Pts',(30.8502989952168,-8.35574267317688,144.201660218991));
#39220=CARTESIAN_POINT('Ctrl Pts',(30.558037054575,-8.2659539292109,144.314493271249));
#39221=CARTESIAN_POINT('Ctrl Pts',(30.2356236626453,-8.19124684145658,144.351553122611));
#39222=CARTESIAN_POINT('Ctrl Pts',(30.0640055623709,-8.18336746578261,144.355691316105));
#39223=CARTESIAN_POINT('Ctrl Pts',(30.0513226380827,-8.18282772898188,144.355968145438));
#39224=CARTESIAN_POINT('Ctrl Pts',(30.0386195894541,-8.18245156556629,144.356161937062));
#39225=CARTESIAN_POINT('Ctrl Pts',(30.0025425983683,-8.18173837270729,144.356528098816));
#39226=CARTESIAN_POINT('Ctrl Pts',(29.949327590037,-8.18215812697606,144.356319671809));
#39227=CARTESIAN_POINT('Ctrl Pts',(29.8965215329261,-8.18546023959715,144.35462295684));
#39228=CARTESIAN_POINT('Ctrl Pts',(29.8508694789328,-8.18947694445684,144.352489515548));
#39229=CARTESIAN_POINT('Ctrl Pts',(29.8124450528999,-8.19359284366967,144.350292014722));
#39230=CARTESIAN_POINT('Ctrl Pts',(29.7743380762458,-8.1989686017083,144.347220946225));
#39231=CARTESIAN_POINT('Ctrl Pts',(29.5344604689754,-8.23692760605077,144.325651942801));
#39232=CARTESIAN_POINT('Ctrl Pts',(29.2537520091736,-8.33190569493299,144.257191468094));
#39233=CARTESIAN_POINT('Ctrl Pts',(29.0091684344659,-8.38313739956724,144.121445328289));
#39234=CARTESIAN_POINT('Ctrl Pts',(28.9499455367427,-8.39129047171135,144.083016665483));
#39235=CARTESIAN_POINT('Ctrl Pts',(31.0316987878737,-8.4275269811409,144.055344443655));
#39236=CARTESIAN_POINT('Ctrl Pts',(31.0232527754724,-8.42675875494622,144.060869589794));
#39237=CARTESIAN_POINT('Ctrl Pts',(31.0147553444553,-8.42587943776685,144.066303064911));
#39238=CARTESIAN_POINT('Ctrl Pts',(30.9946853864034,-8.42360243871762,144.07890286189));
#39239=CARTESIAN_POINT('Ctrl Pts',(30.9830372481524,-8.42210831653301,144.085988643756));
#39240=CARTESIAN_POINT('Ctrl Pts',(30.8310662630449,-8.40062314502122,144.176010199841));
#39241=CARTESIAN_POINT('Ctrl Pts',(30.5383283564013,-8.32003419197623,144.292952674175));
#39242=CARTESIAN_POINT('Ctrl Pts',(30.2247435582948,-8.25116314278318,144.33256898185));
#39243=CARTESIAN_POINT('Ctrl Pts',(30.0611760154067,-8.24414097291916,144.336897172084));
#39244=CARTESIAN_POINT('Ctrl Pts',(30.0490244691322,-8.24363821830494,144.337194280782));
#39245=CARTESIAN_POINT('Ctrl Pts',(30.0369088739531,-8.24330388773372,144.337397022135));
#39246=CARTESIAN_POINT('Ctrl Pts',(30.0024432035511,-8.24265189581713,144.337786084088));
#39247=CARTESIAN_POINT('Ctrl Pts',(29.9516451181674,-8.24303779805442,144.337563550915));
#39248=CARTESIAN_POINT('Ctrl Pts',(29.9011427210787,-8.24603722149251,144.335767184191));
#39249=CARTESIAN_POINT('Ctrl Pts',(29.857399378596,-8.2497015555049,144.333505775426));
#39250=CARTESIAN_POINT('Ctrl Pts',(29.8205273527128,-8.25344039474353,144.331181766681));
#39251=CARTESIAN_POINT('Ctrl Pts',(29.7838223086098,-8.25836498371357,144.327927772113));
#39252=CARTESIAN_POINT('Ctrl Pts',(29.5523533776709,-8.29291263025922,144.305133904073));
#39253=CARTESIAN_POINT('Ctrl Pts',(29.2734876151046,-8.38080321331592,144.232781780034));
#39254=CARTESIAN_POINT('Ctrl Pts',(29.0279259955364,-8.42207186623694,144.094304677965));
#39255=CARTESIAN_POINT('Ctrl Pts',(28.9683012121263,-8.4275269811409,144.055344443655));
#39256=CARTESIAN_POINT('Ctrl Pts',(31.0133431124902,-8.46376349057045,144.027672221828));
#39257=CARTESIAN_POINT('Ctrl Pts',(31.0048303036347,-8.46337569595993,144.033275003465));
#39258=CARTESIAN_POINT('Ctrl Pts',(30.9963094453813,-8.4628889223465,144.038785971762));
#39259=CARTESIAN_POINT('Ctrl Pts',(30.9760797687839,-8.46148171290697,144.051582436227));
#39260=CARTESIAN_POINT('Ctrl Pts',(30.9644249961142,-8.46051430961044,144.058780581885));
#39261=CARTESIAN_POINT('Ctrl Pts',(30.811663986886,-8.44541570746616,144.150365816204));
#39262=CARTESIAN_POINT('Ctrl Pts',(30.5184370781297,-8.37405874016662,144.271435163949));
#39263=CARTESIAN_POINT('Ctrl Pts',(30.2145450560986,-8.31126754234417,144.313519514008));
#39264=CARTESIAN_POINT('Ctrl Pts',(30.0580521168044,-8.30480713431659,144.318143569817));
#39265=CARTESIAN_POINT('Ctrl Pts',(30.0465137000413,-8.30437370070772,144.318450715706));
#39266=CARTESIAN_POINT('Ctrl Pts',(30.034933916069,-8.30406014627328,144.318669166289));
#39267=CARTESIAN_POINT('Ctrl Pts',(30.0020987157711,-8.30347844330574,144.31907802629));
#39268=CARTESIAN_POINT('Ctrl Pts',(29.9537071077953,-8.30381904774098,144.318845302261));
#39269=CARTESIAN_POINT('Ctrl Pts',(29.9055195030814,-8.30653012524895,144.316944860243));
#39270=CARTESIAN_POINT('Ctrl Pts',(29.8636848030784,-8.30982716472501,144.3145602471));
#39271=CARTESIAN_POINT('Ctrl Pts',(29.8283694070157,-8.31322211431118,144.31209976428));
#39272=CARTESIAN_POINT('Ctrl Pts',(29.7930638488286,-8.31764796375963,144.308677235497));
#39273=CARTESIAN_POINT('Ctrl Pts',(29.5699541610066,-8.3490326254289,144.284592127057));
#39274=CARTESIAN_POINT('Ctrl Pts',(29.2933240301876,-8.42964020165404,144.20838609147));
#39275=CARTESIAN_POINT('Ctrl Pts',(29.0466376445571,-8.4610655333303,144.067193964284));
#39276=CARTESIAN_POINT('Ctrl Pts',(28.9866568875098,-8.46376349057045,144.027672221828));
#39277=CARTESIAN_POINT('Ctrl Pts',(30.9949874371066,-8.5,144.));
#39278=CARTESIAN_POINT('Ctrl Pts',(30.9864258065899,-8.5,144.005679143204));
#39279=CARTESIAN_POINT('Ctrl Pts',(30.9778381533882,-8.49988803935537,144.011270671384));
#39280=CARTESIAN_POINT('Ctrl Pts',(30.957514713753,-8.49937799036647,144.024259127581));
#39281=CARTESIAN_POINT('Ctrl Pts',(30.9457617930679,-8.49889895697764,144.031575977005));
#39282=CARTESIAN_POINT('Ctrl Pts',(30.7924312547142,-8.4902961793105,144.124715797054));
#39283=CARTESIAN_POINT('Ctrl Pts',(30.4987283799559,-8.42813900293195,144.249894566875));
#39284=CARTESIAN_POINT('Ctrl Pts',(30.203664951748,-8.37118384367076,144.294535373247));
#39285=CARTESIAN_POINT('Ctrl Pts',(30.0552225698401,-8.36558064145315,144.299349425796));
#39286=CARTESIAN_POINT('Ctrl Pts',(30.0442155310909,-8.36518419003078,144.29967685105));
#39287=CARTESIAN_POINT('Ctrl Pts',(30.033223200568,-8.36491246844071,144.299904251363));
#39288=CARTESIAN_POINT('Ctrl Pts',(30.0019993209539,-8.36439196641558,144.300336011563));
#39289=CARTESIAN_POINT('Ctrl Pts',(29.9560246359257,-8.36469871881934,144.300089181366));
#39290=CARTESIAN_POINT('Ctrl Pts',(29.910140691234,-8.36710710714431,144.298089087593));
#39291=CARTESIAN_POINT('Ctrl Pts',(29.8702147027416,-8.37005177577307,144.295576506978));
#39292=CARTESIAN_POINT('Ctrl Pts',(29.8364517068287,-8.37306966538504,144.29298951624));
#39293=CARTESIAN_POINT('Ctrl Pts',(29.8025480811926,-8.3770443457649,144.289384061385));
#39294=CARTESIAN_POINT('Ctrl Pts',(29.5878470697021,-8.40501764963735,144.264074088329));
#39295=CARTESIAN_POINT('Ctrl Pts',(29.3130596361187,-8.47853772003697,144.18397640341));
#39296=CARTESIAN_POINT('Ctrl Pts',(29.0653952056276,-8.5,144.04005331396));
#39297=CARTESIAN_POINT('Ctrl Pts',(29.0050125628934,-8.5,144.));
#39298=CARTESIAN_POINT('',(31.0500544632573,-8.39129047171135,144.083016665483));
#39299=CARTESIAN_POINT('',(29.0050125628934,-8.5,144.));
#39300=CARTESIAN_POINT('Origin',(30.,-8.45,142.5));
#39301=CARTESIAN_POINT('',(28.8338096210309,-8.4,144.));
#39302=CARTESIAN_POINT('',(31.1048119379707,-8.5,143.921052631579));
#39303=CARTESIAN_POINT('Ctrl Pts',(28.9499455367427,-8.39129047171135,144.083016665483));
#39304=CARTESIAN_POINT('Ctrl Pts',(28.9100201948423,-8.39678689632762,144.057109836194));
#39305=CARTESIAN_POINT('Ctrl Pts',(28.8713894960226,-8.40000000009859,144.029216859175));
#39306=CARTESIAN_POINT('Ctrl Pts',(28.8338096192948,-8.4,143.99999999865));
#39307=CARTESIAN_POINT('Ctrl Pts',(28.9683012121263,-8.4275269811409,144.055344443655));
#39308=CARTESIAN_POINT('Ctrl Pts',(28.9291576919388,-8.43119126421841,144.029764000737));
#39309=CARTESIAN_POINT('Ctrl Pts',(28.8911896803029,-8.43333333339906,144.002388493225));
#39310=CARTESIAN_POINT('Ctrl Pts',(28.854269099658,-8.43333333333333,143.9736842092));
#39311=CARTESIAN_POINT('Ctrl Pts',(28.9866568875098,-8.46376349057045,144.027672221828));
#39312=CARTESIAN_POINT('Ctrl Pts',(28.9482951890352,-8.46559563210921,144.00241816528));
#39313=CARTESIAN_POINT('Ctrl Pts',(28.9109898645832,-8.46666666669953,143.975560127274));
#39314=CARTESIAN_POINT('Ctrl Pts',(28.8747285800213,-8.46666666666667,143.94736841975));
#39315=CARTESIAN_POINT('Ctrl Pts',(29.0050125628934,-8.5,144.));
#39316=CARTESIAN_POINT('Ctrl Pts',(28.9674326861317,-8.5,143.975072329823));
#39317=CARTESIAN_POINT('Ctrl Pts',(28.9307900488635,-8.5,143.948731761324));
#39318=CARTESIAN_POINT('Ctrl Pts',(28.8951880603845,-8.5,143.9210526303));
#39319=CARTESIAN_POINT('Ctrl Pts',(31.166190378969,-8.4,144.));
#39320=CARTESIAN_POINT('Ctrl Pts',(31.1286105027861,-8.4,144.029216860032));
#39321=CARTESIAN_POINT('Ctrl Pts',(31.0899798045429,-8.39678689624297,144.057109836593));
#39322=CARTESIAN_POINT('Ctrl Pts',(31.0500544632573,-8.39129047171134,144.083016665483));
#39323=CARTESIAN_POINT('Ctrl Pts',(31.1457308986363,-8.43333333333333,143.973684210526));
#39324=CARTESIAN_POINT('Ctrl Pts',(31.1088103185267,-8.43333333333333,144.002388494066));
#39325=CARTESIAN_POINT('Ctrl Pts',(31.0708423074584,-8.43119126416198,144.029764001131));
#39326=CARTESIAN_POINT('Ctrl Pts',(31.0316987878737,-8.4275269811409,144.055344443655));
#39327=CARTESIAN_POINT('Ctrl Pts',(31.1252714183035,-8.46666666666667,143.947368421053));
#39328=CARTESIAN_POINT('Ctrl Pts',(31.0890101342673,-8.46666666666667,143.975560128101));
#39329=CARTESIAN_POINT('Ctrl Pts',(31.051704810374,-8.46559563208099,144.002418165669));
#39330=CARTESIAN_POINT('Ctrl Pts',(31.0133431124902,-8.46376349057045,144.027672221828));
#39331=CARTESIAN_POINT('Ctrl Pts',(31.1048119379707,-8.5,143.921052631579));
#39332=CARTESIAN_POINT('Ctrl Pts',(31.0692099500079,-8.5,143.948731762135));
#39333=CARTESIAN_POINT('Ctrl Pts',(31.0325673132895,-8.5,143.975072330207));
#39334=CARTESIAN_POINT('Ctrl Pts',(30.9949874371066,-8.5,144.));
#39335=CARTESIAN_POINT('Ctrl Pts',(-28.9499455367427,-8.39129047171135,
144.083016665483));
#39336=CARTESIAN_POINT('Ctrl Pts',(-28.9583427274828,-8.39013445090614,
144.088465450056));
#39337=CARTESIAN_POINT('Ctrl Pts',(-28.9667729665848,-8.38888022833652,
144.093818270446));
#39338=CARTESIAN_POINT('Ctrl Pts',(-28.9867489659987,-8.38570638741796,
144.10622492921));
#39339=CARTESIAN_POINT('Ctrl Pts',(-28.9982975463468,-8.38372232493232,
144.113195422252));
#39340=CARTESIAN_POINT('Ctrl Pts',(-29.2186401675363,-8.34304381026164,
144.241830661973));
#39341=CARTESIAN_POINT('Ctrl Pts',(-29.4418894510009,-8.26130877991199,
144.30791109331));
#39342=CARTESIAN_POINT('Ctrl Pts',(-29.7387539667785,-8.2037212977524,144.344577795757));
#39343=CARTESIAN_POINT('Ctrl Pts',(-29.7961080426536,-8.19484695032281,
144.349486882414));
#39344=CARTESIAN_POINT('Ctrl Pts',(-29.8806159996987,-8.18658920666495,
144.35392173636));
#39345=CARTESIAN_POINT('Ctrl Pts',(-29.9067939860508,-8.18468265252138,
144.354910990812));
#39346=CARTESIAN_POINT('Ctrl Pts',(-29.945800622645,-8.18289510415931,144.355834150072));
#39347=CARTESIAN_POINT('Ctrl Pts',(-29.9584929581617,-8.18247823187435,
144.356048044385));
#39348=CARTESIAN_POINT('Ctrl Pts',(-30.0243207374447,-8.18117200076953,
144.35671442715));
#39349=CARTESIAN_POINT('Ctrl Pts',(-30.0774739256815,-8.18309698929938,
144.355772172055));
#39350=CARTESIAN_POINT('Ctrl Pts',(-30.1687494835259,-8.19113640094687,
144.351508081756));
#39351=CARTESIAN_POINT('Ctrl Pts',(-30.2069857608087,-8.19595190722736,
144.348893235529));
#39352=CARTESIAN_POINT('Ctrl Pts',(-30.2909203211106,-8.20912670855604,
144.341198190437));
#39353=CARTESIAN_POINT('Ctrl Pts',(-30.3362573241971,-8.21797318024007,
144.335720743413));
#39354=CARTESIAN_POINT('Ctrl Pts',(-30.5020752162372,-8.25459576965121,
144.310394503157));
#39355=CARTESIAN_POINT('Ctrl Pts',(-30.6785437628854,-8.30590308055624,
144.267185314179));
#39356=CARTESIAN_POINT('Ctrl Pts',(-30.8980141119118,-8.36393098595595,
144.173469870658));
#39357=CARTESIAN_POINT('Ctrl Pts',(-31.0000499887335,-8.38440647744572,
144.115463660888));
#39358=CARTESIAN_POINT('Ctrl Pts',(-31.0500544632573,-8.39129047171135,
144.083016665483));
#39359=CARTESIAN_POINT('Ctrl Pts',(-28.9683012121262,-8.4275269811409,144.055344443655));
#39360=CARTESIAN_POINT('Ctrl Pts',(-28.9767493819959,-8.42675549228855,
144.060870258443));
#39361=CARTESIAN_POINT('Ctrl Pts',(-28.9852412077866,-8.42588395004709,
144.066302026648));
#39362=CARTESIAN_POINT('Ctrl Pts',(-29.0053194448347,-8.42359452300562,
144.078903287352));
#39363=CARTESIAN_POINT('Ctrl Pts',(-29.0169530524388,-8.42211782206045,
144.085988617456));
#39364=CARTESIAN_POINT('Ctrl Pts',(-29.2382331610903,-8.39077316976861,
144.216909192503));
#39365=CARTESIAN_POINT('Ctrl Pts',(-29.461356759406,-8.31521293772752,144.286451078415));
#39366=CARTESIAN_POINT('Ctrl Pts',(-29.749585494796,-8.26271593529331,144.325132711801));
#39367=CARTESIAN_POINT('Ctrl Pts',(-29.8048435404432,-8.25457093527495,
144.330334839234));
#39368=CARTESIAN_POINT('Ctrl Pts',(-29.8858928226077,-8.24707060474715,
144.335028465043));
#39369=CARTESIAN_POINT('Ctrl Pts',(-29.9109385934974,-8.24532469917957,
144.336077514689));
#39370=CARTESIAN_POINT('Ctrl Pts',(-29.948225057183,-8.2437038171456,144.337055022579));
#39371=CARTESIAN_POINT('Ctrl Pts',(-29.9603509120841,-8.24332251105181,
144.337281796721));
#39372=CARTESIAN_POINT('Ctrl Pts',(-30.0232223452457,-8.24213657114161,
144.337987844979));
#39373=CARTESIAN_POINT('Ctrl Pts',(-30.073949242754,-8.24388416139077,144.336988263353));
#39374=CARTESIAN_POINT('Ctrl Pts',(-30.1614126316311,-8.25120466871815,
144.332472186435));
#39375=CARTESIAN_POINT('Ctrl Pts',(-30.1981600720549,-8.25559824756781,
144.329702532905));
#39376=CARTESIAN_POINT('Ctrl Pts',(-30.2791744174637,-8.26762595023983,
144.32156645137));
#39377=CARTESIAN_POINT('Ctrl Pts',(-30.323163151243,-8.27572554982767,144.315778125701));
#39378=CARTESIAN_POINT('Ctrl Pts',(-30.4848913781063,-8.30919937251611,
144.289109186482));
#39379=CARTESIAN_POINT('Ctrl Pts',(-30.6594654545242,-8.35615409386017,
144.243787223357));
#39380=CARTESIAN_POINT('Ctrl Pts',(-30.87884927204,-8.40671689444657,144.147356675181));
#39381=CARTESIAN_POINT('Ctrl Pts',(-30.9813729272218,-8.4229080086506,144.088243385872));
#39382=CARTESIAN_POINT('Ctrl Pts',(-31.0316987878737,-8.4275269811409,144.055344443655));
#39383=CARTESIAN_POINT('Ctrl Pts',(-28.9866568875098,-8.46376349057045,
144.027672221828));
#39384=CARTESIAN_POINT('Ctrl Pts',(-28.995167538897,-8.46337895861759,144.033274334817));
#39385=CARTESIAN_POINT('Ctrl Pts',(-29.0036936841412,-8.46288455223563,
144.038786782293));
#39386=CARTESIAN_POINT('Ctrl Pts',(-29.0239172360346,-8.46148854556296,
144.051579899216));
#39387=CARTESIAN_POINT('Ctrl Pts',(-29.035577524684,-8.46050864492644,144.058783731614));
#39388=CARTESIAN_POINT('Ctrl Pts',(-29.257997707443,-8.43848024319824,144.191977951185));
#39389=CARTESIAN_POINT('Ctrl Pts',(-29.4809442721626,-8.3693753244674,144.26497426448));
#39390=CARTESIAN_POINT('Ctrl Pts',(-29.7603830839415,-8.32162051846762,
144.305701005651));
#39391=CARTESIAN_POINT('Ctrl Pts',(-29.8136051874221,-8.31431970227491,
144.311186300222));
#39392=CARTESIAN_POINT('Ctrl Pts',(-29.8911637448792,-8.30751073943584,
144.316145055182));
#39393=CARTESIAN_POINT('Ctrl Pts',(-29.9150906805591,-8.30595688428399,
144.317251044948));
#39394=CARTESIAN_POINT('Ctrl Pts',(-29.950651095842,-8.30448658024128,144.318284380908));
#39395=CARTESIAN_POINT('Ctrl Pts',(-29.9622104521088,-8.3041471128788,144.318523615133));
#39396=CARTESIAN_POINT('Ctrl Pts',(-30.0221330002508,-8.30307648025771,
144.319269178193));
#39397=CARTESIAN_POINT('Ctrl Pts',(-30.0704295912641,-8.3046510696591,144.318213009246));
#39398=CARTESIAN_POINT('Ctrl Pts',(-30.1540743548903,-8.31125999852809,
144.313443903216));
#39399=CARTESIAN_POINT('Ctrl Pts',(-30.1893363532634,-8.31522485466993,
144.310521180289));
#39400=CARTESIAN_POINT('Ctrl Pts',(-30.2674275548308,-8.32612149867921,
144.301941089706));
#39401=CARTESIAN_POINT('Ctrl Pts',(-30.3100712021484,-8.3334556333502,144.295846594569));
#39402=CARTESIAN_POINT('Ctrl Pts',(-30.4677047486626,-8.36383032392711,
144.267824415337));
#39403=CARTESIAN_POINT('Ctrl Pts',(-30.640377126088,-8.40646040610892,144.220399683195));
#39404=CARTESIAN_POINT('Ctrl Pts',(-30.8596850431782,-8.44950872487433,
144.121245390691));
#39405=CARTESIAN_POINT('Ctrl Pts',(-30.9626808008196,-8.46149846879512,
144.061039034221));
#39406=CARTESIAN_POINT('Ctrl Pts',(-31.0133431124902,-8.46376349057045,
144.027672221828));
#39407=CARTESIAN_POINT('Ctrl Pts',(-29.0050125628934,-8.5,144.));
#39408=CARTESIAN_POINT('Ctrl Pts',(-29.0135741934101,-8.5,144.005679143204));
#39409=CARTESIAN_POINT('Ctrl Pts',(-29.0221619253429,-8.4998882739462,144.011270538495));
#39410=CARTESIAN_POINT('Ctrl Pts',(-29.0424877148706,-8.49937668115061,
144.024258257358));
#39411=CARTESIAN_POINT('Ctrl Pts',(-29.054233030776,-8.49890414205457,144.031576926818));
#39412=CARTESIAN_POINT('Ctrl Pts',(-29.277590700997,-8.48620960270521,144.167056481715));
#39413=CARTESIAN_POINT('Ctrl Pts',(-29.5004115805678,-8.42327948228293,
144.243514249585));
#39414=CARTESIAN_POINT('Ctrl Pts',(-29.7712146119589,-8.38061515600853,
144.286255921694));
#39415=CARTESIAN_POINT('Ctrl Pts',(-29.8223406852117,-8.37404368722705,
144.292034257043));
#39416=CARTESIAN_POINT('Ctrl Pts',(-29.8964405677882,-8.36799213751804,
144.297251783865));
#39417=CARTESIAN_POINT('Ctrl Pts',(-29.9192352880058,-8.36659893094219,
144.298417568824));
#39418=CARTESIAN_POINT('Ctrl Pts',(-29.95307553038,-8.36529529322757,144.299505253415));
#39419=CARTESIAN_POINT('Ctrl Pts',(-29.9640684060312,-8.36499139205626,
144.299757367469));
#39420=CARTESIAN_POINT('Ctrl Pts',(-30.0210346080518,-8.36404105062979,
144.300542596022));
#39421=CARTESIAN_POINT('Ctrl Pts',(-30.0669049083367,-8.36543824175049,
144.299429100544));
#39422=CARTESIAN_POINT('Ctrl Pts',(-30.1467375029954,-8.37132826629937,
144.294408007895));
#39423=CARTESIAN_POINT('Ctrl Pts',(-30.1805106645095,-8.37487119501038,
144.291330477666));
#39424=CARTESIAN_POINT('Ctrl Pts',(-30.2556816511839,-8.384620740363,144.282309350639));
#39425=CARTESIAN_POINT('Ctrl Pts',(-30.2969770291942,-8.39120800293779,
144.275903976857));
#39426=CARTESIAN_POINT('Ctrl Pts',(-30.4505209105317,-8.41843392679202,
144.246539098663));
#39427=CARTESIAN_POINT('Ctrl Pts',(-30.6212988177268,-8.45671141941285,
144.197001592374));
#39428=CARTESIAN_POINT('Ctrl Pts',(-30.8405202033064,-8.49229463336495,
144.095132195214));
#39429=CARTESIAN_POINT('Ctrl Pts',(-30.9440037393079,-8.5,144.033818759205));
#39430=CARTESIAN_POINT('Ctrl Pts',(-30.9949874371066,-8.5,144.));
#39431=CARTESIAN_POINT('',(-28.9499455367427,-8.39129047171135,144.083016665483));
#39432=CARTESIAN_POINT('',(-30.9949874371066,-8.5,144.));
#39433=CARTESIAN_POINT('Origin',(-30.,-8.45,142.5));
#39434=CARTESIAN_POINT('',(-31.1661903789691,-8.4,144.));
#39435=CARTESIAN_POINT('',(-28.8951880620293,-8.5,143.921052631579));
#39436=CARTESIAN_POINT('Ctrl Pts',(-31.0500544632573,-8.39129047171135,
144.083016665483));
#39437=CARTESIAN_POINT('Ctrl Pts',(-31.0899798051577,-8.39678689632762,
144.057109836194));
#39438=CARTESIAN_POINT('Ctrl Pts',(-31.1286105039774,-8.40000000009859,
144.029216859175));
#39439=CARTESIAN_POINT('Ctrl Pts',(-31.1661903807052,-8.4,143.99999999865));
#39440=CARTESIAN_POINT('Ctrl Pts',(-31.0316987878738,-8.4275269811409,144.055344443655));
#39441=CARTESIAN_POINT('Ctrl Pts',(-31.0708423080613,-8.43119126421841,
144.029764000737));
#39442=CARTESIAN_POINT('Ctrl Pts',(-31.1088103196971,-8.43333333339906,
144.002388493225));
#39443=CARTESIAN_POINT('Ctrl Pts',(-31.145730900342,-8.43333333333333,143.9736842092));
#39444=CARTESIAN_POINT('Ctrl Pts',(-31.0133431124902,-8.46376349057045,
144.027672221828));
#39445=CARTESIAN_POINT('Ctrl Pts',(-31.0517048109648,-8.46559563210921,
144.00241816528));
#39446=CARTESIAN_POINT('Ctrl Pts',(-31.0890101354168,-8.46666666669953,
143.975560127274));
#39447=CARTESIAN_POINT('Ctrl Pts',(-31.1252714199787,-8.46666666666667,
143.94736841975));
#39448=CARTESIAN_POINT('Ctrl Pts',(-30.9949874371066,-8.5,144.));
#39449=CARTESIAN_POINT('Ctrl Pts',(-31.0325673138683,-8.5,143.975072329823));
#39450=CARTESIAN_POINT('Ctrl Pts',(-31.0692099511365,-8.5,143.948731761324));
#39451=CARTESIAN_POINT('Ctrl Pts',(-31.1048119396155,-8.5,143.9210526303));
#39452=CARTESIAN_POINT('Ctrl Pts',(-28.833809621031,-8.4,144.));
#39453=CARTESIAN_POINT('Ctrl Pts',(-28.8713894972139,-8.4,144.029216860032));
#39454=CARTESIAN_POINT('Ctrl Pts',(-28.9100201954571,-8.39678689624297,
144.057109836593));
#39455=CARTESIAN_POINT('Ctrl Pts',(-28.9499455367427,-8.39129047171135,
144.083016665483));
#39456=CARTESIAN_POINT('Ctrl Pts',(-28.8542691013637,-8.43333333333333,
143.973684210526));
#39457=CARTESIAN_POINT('Ctrl Pts',(-28.8911896814733,-8.43333333333333,
144.002388494066));
#39458=CARTESIAN_POINT('Ctrl Pts',(-28.9291576925416,-8.43119126416198,
144.029764001131));
#39459=CARTESIAN_POINT('Ctrl Pts',(-28.9683012121263,-8.4275269811409,144.055344443655));
#39460=CARTESIAN_POINT('Ctrl Pts',(-28.8747285816965,-8.46666666666667,
143.947368421053));
#39461=CARTESIAN_POINT('Ctrl Pts',(-28.9109898657327,-8.46666666666667,
143.975560128101));
#39462=CARTESIAN_POINT('Ctrl Pts',(-28.948295189626,-8.46559563208099,144.002418165669));
#39463=CARTESIAN_POINT('Ctrl Pts',(-28.9866568875098,-8.46376349057045,
144.027672221828));
#39464=CARTESIAN_POINT('Ctrl Pts',(-28.8951880620293,-8.5,143.921052631579));
#39465=CARTESIAN_POINT('Ctrl Pts',(-28.9307900499921,-8.5,143.948731762135));
#39466=CARTESIAN_POINT('Ctrl Pts',(-28.9674326867105,-8.5,143.975072330207));
#39467=CARTESIAN_POINT('Ctrl Pts',(-29.0050125628934,-8.5,144.));
#39468=CARTESIAN_POINT('Origin',(30.,-8.95,137.5));
#39469=CARTESIAN_POINT('',(29.19613123823,-8.9,135.889473684211));
#39470=CARTESIAN_POINT('',(29.1514718625761,-9.,135.8));
#39471=CARTESIAN_POINT('',(28.2,-8.9,137.5));
#39472=CARTESIAN_POINT('Origin',(30.,-8.9,137.5));
#39473=CARTESIAN_POINT('',(30.80386876177,-8.9,135.889473684211));
#39474=CARTESIAN_POINT('Origin',(30.,-8.9,137.5));
#39475=CARTESIAN_POINT('',(30.80386876177,-8.9,135.889473684211));
#39476=CARTESIAN_POINT('Ctrl Pts',(30.62442393624,-8.99442305443429,135.70570254201));
#39477=CARTESIAN_POINT('Ctrl Pts',(30.6031336007837,-8.99354972599348,135.698345055793));
#39478=CARTESIAN_POINT('Ctrl Pts',(30.5816752394099,-8.9926310079646,135.691382689721));
#39479=CARTESIAN_POINT('Ctrl Pts',(30.4123094665995,-8.98495128128084,135.639444028187));
#39480=CARTESIAN_POINT('Ctrl Pts',(30.1802232821902,-8.97487183787893,135.600774173325));
#39481=CARTESIAN_POINT('Ctrl Pts',(29.8198774693528,-8.97481364719588,135.600649477793));
#39482=CARTESIAN_POINT('Ctrl Pts',(29.5876626138109,-8.9849459908676,135.639432675438));
#39483=CARTESIAN_POINT('Ctrl Pts',(29.418327451187,-8.9926309002887,135.69138245992));
#39484=CARTESIAN_POINT('Ctrl Pts',(29.3968663992163,-8.99354972599348,135.698345055793));
#39485=CARTESIAN_POINT('Ctrl Pts',(29.37557606376,-8.99442305443429,135.70570254201));
#39486=CARTESIAN_POINT('Ctrl Pts',(30.6134852835967,-8.96294870295619,135.737135028007));
#39487=CARTESIAN_POINT('Ctrl Pts',(30.5926585146851,-8.96237089086999,135.729918298573));
#39488=CARTESIAN_POINT('Ctrl Pts',(30.5716540370928,-8.96172231480688,135.723090172466));
#39489=CARTESIAN_POINT('Ctrl Pts',(30.4057627068959,-8.95618694003155,135.671989821309));
#39490=CARTESIAN_POINT('Ctrl Pts',(30.1774809150283,-8.94781763959254,135.633524301555));
#39491=CARTESIAN_POINT('Ctrl Pts',(29.8226191720034,-8.94775803303614,135.63340083736));
#39492=CARTESIAN_POINT('Ctrl Pts',(29.5942099936947,-8.9561825817824,135.671977657887));
#39493=CARTESIAN_POINT('Ctrl Pts',(29.4283485325563,-8.96172203669287,135.723090090889));
#39494=CARTESIAN_POINT('Ctrl Pts',(29.4073415857357,-8.96237102991341,135.729918177652));
#39495=CARTESIAN_POINT('Ctrl Pts',(29.3865147164033,-8.96294870295619,135.737135028007));
#39496=CARTESIAN_POINT('Ctrl Pts',(30.6025466309533,-8.9314743514781,135.768567514004));
#39497=CARTESIAN_POINT('Ctrl Pts',(30.582184785483,-8.93117883512348,135.761502062769));
#39498=CARTESIAN_POINT('Ctrl Pts',(30.5616314866267,-8.93082738428349,135.754786613407));
#39499=CARTESIAN_POINT('Ctrl Pts',(30.3992200288979,-8.92734716856885,135.704598391766));
#39500=CARTESIAN_POINT('Ctrl Pts',(30.1747360509691,-8.92072266060556,135.666303758425));
#39501=CARTESIAN_POINT('Ctrl Pts',(29.8253607851682,-8.92068624425422,135.666171804744));
#39502=CARTESIAN_POINT('Ctrl Pts',(29.6007527034052,-8.9273427984036,135.704587303278));
#39503=CARTESIAN_POINT('Ctrl Pts',(29.4383712024403,-8.93082748462833,135.75478622414));
#39504=CARTESIAN_POINT('Ctrl Pts',(29.4178151140962,-8.93117869608006,135.761502183691));
#39505=CARTESIAN_POINT('Ctrl Pts',(29.3974533690467,-8.9314743514781,135.768567514004));
#39506=CARTESIAN_POINT('Ctrl Pts',(30.59160797831,-8.9,135.8));
#39507=CARTESIAN_POINT('Ctrl Pts',(30.5717096993844,-8.9,135.793075305549));
#39508=CARTESIAN_POINT('Ctrl Pts',(30.5516102843096,-8.89991869112576,135.786494096152));
#39509=CARTESIAN_POINT('Ctrl Pts',(30.3926732691942,-8.89858282731956,135.737144184887));
#39510=CARTESIAN_POINT('Ctrl Pts',(30.1719936838072,-8.89366846231917,135.699053886655));
#39511=CARTESIAN_POINT('Ctrl Pts',(29.8281024878188,-8.89363063009448,135.698923164311));
#39512=CARTESIAN_POINT('Ctrl Pts',(29.607300083289,-8.8985793893184,135.737132285728));
#39513=CARTESIAN_POINT('Ctrl Pts',(29.4483922838095,-8.8999186210325,135.78649385511));
#39514=CARTESIAN_POINT('Ctrl Pts',(29.4282903006156,-8.9,135.793075305549));
#39515=CARTESIAN_POINT('Ctrl Pts',(29.40839202169,-8.9,135.8));
#39516=CARTESIAN_POINT('',(29.40839202169,-8.9,135.8));
#39517=CARTESIAN_POINT('',(29.40839202169,-8.9,135.8));
#39518=CARTESIAN_POINT('',(30.59160797831,-8.9,135.8));
#39519=CARTESIAN_POINT('',(30.62442393624,-8.99442305443429,135.70570254201));
#39520=CARTESIAN_POINT('Ctrl Pts',(30.59160797831,-8.9,135.8));
#39521=CARTESIAN_POINT('Ctrl Pts',(30.5717096993844,-8.9,135.793075305549));
#39522=CARTESIAN_POINT('Ctrl Pts',(30.5516102843096,-8.89991869112576,135.786494096152));
#39523=CARTESIAN_POINT('Ctrl Pts',(30.3926732691942,-8.89858282731956,135.737144184887));
#39524=CARTESIAN_POINT('Ctrl Pts',(30.1719936838072,-8.89366846231917,135.699053886655));
#39525=CARTESIAN_POINT('Ctrl Pts',(29.8281024878188,-8.89363063009448,135.698923164311));
#39526=CARTESIAN_POINT('Ctrl Pts',(29.607300083289,-8.8985793893184,135.737132285728));
#39527=CARTESIAN_POINT('Ctrl Pts',(29.4483922838095,-8.8999186210325,135.78649385511));
#39528=CARTESIAN_POINT('Ctrl Pts',(29.4282903006156,-8.9,135.793075305549));
#39529=CARTESIAN_POINT('Ctrl Pts',(29.40839202169,-8.9,135.8));
#39530=CARTESIAN_POINT('Ctrl Pts',(30.8485281374239,-9.,135.8));
#39531=CARTESIAN_POINT('Ctrl Pts',(30.7759616147067,-9.,135.763779566847));
#39532=CARTESIAN_POINT('Ctrl Pts',(30.7010733797628,-8.99756721057679,135.732190956222));
#39533=CARTESIAN_POINT('Ctrl Pts',(30.62442393624,-8.99442305443429,135.70570254201));
#39534=CARTESIAN_POINT('Ctrl Pts',(30.8336416788726,-8.96666666666667,135.829824561404));
#39535=CARTESIAN_POINT('Ctrl Pts',(30.7623482530451,-8.96666666666667,135.794239574446));
#39536=CARTESIAN_POINT('Ctrl Pts',(30.6887737535176,-8.96504480705119,135.763211800971));
#39537=CARTESIAN_POINT('Ctrl Pts',(30.6134852835966,-8.96294870295619,135.737135028007));
#39538=CARTESIAN_POINT('Ctrl Pts',(30.8187552203213,-8.93333333333333,135.859649122807));
#39539=CARTESIAN_POINT('Ctrl Pts',(30.7487348913836,-8.93333333333333,135.824699582045));
#39540=CARTESIAN_POINT('Ctrl Pts',(30.6764741272724,-8.9325224035256,135.79423264572));
#39541=CARTESIAN_POINT('Ctrl Pts',(30.6025466309533,-8.9314743514781,135.768567514003));
#39542=CARTESIAN_POINT('Ctrl Pts',(30.80386876177,-8.9,135.889473684211));
#39543=CARTESIAN_POINT('Ctrl Pts',(30.7351215297221,-8.9,135.855159589644));
#39544=CARTESIAN_POINT('Ctrl Pts',(30.6641745010272,-8.9,135.825253490469));
#39545=CARTESIAN_POINT('Ctrl Pts',(30.59160797831,-8.9,135.8));
#39546=CARTESIAN_POINT('Ctrl Pts',(30.80386876177,-8.9,135.889473684211));
#39547=CARTESIAN_POINT('Ctrl Pts',(30.7351215297221,-8.9,135.855159589644));
#39548=CARTESIAN_POINT('Ctrl Pts',(30.6641745010272,-8.9,135.825253490469));
#39549=CARTESIAN_POINT('Ctrl Pts',(30.59160797831,-8.9,135.8));
#39550=CARTESIAN_POINT('Ctrl Pts',(29.37557606376,-8.99442305443429,135.70570254201));
#39551=CARTESIAN_POINT('Ctrl Pts',(29.2989266202368,-8.99756721057681,135.732190956222));
#39552=CARTESIAN_POINT('Ctrl Pts',(29.2240383852925,-9.00000000000003,135.763779566847));
#39553=CARTESIAN_POINT('Ctrl Pts',(29.1514718625748,-9.,135.800000000001));
#39554=CARTESIAN_POINT('Ctrl Pts',(29.3865147164033,-8.96294870295619,135.737135028007));
#39555=CARTESIAN_POINT('Ctrl Pts',(29.311226246482,-8.96504480705121,135.763211800971));
#39556=CARTESIAN_POINT('Ctrl Pts',(29.237651746954,-8.96666666666669,135.794239574446));
#39557=CARTESIAN_POINT('Ctrl Pts',(29.1663583211262,-8.96666666666667,135.829824561404));
#39558=CARTESIAN_POINT('Ctrl Pts',(29.3974533690467,-8.9314743514781,135.768567514003));
#39559=CARTESIAN_POINT('Ctrl Pts',(29.3235258727272,-8.9325224035256,135.79423264572));
#39560=CARTESIAN_POINT('Ctrl Pts',(29.2512651086155,-8.93333333333334,135.824699582045));
#39561=CARTESIAN_POINT('Ctrl Pts',(29.1812447796775,-8.93333333333333,135.859649122808));
#39562=CARTESIAN_POINT('Ctrl Pts',(29.40839202169,-8.9,135.8));
#39563=CARTESIAN_POINT('Ctrl Pts',(29.3358254989724,-8.9,135.825253490469));
#39564=CARTESIAN_POINT('Ctrl Pts',(29.2648784702771,-8.9,135.855159589645));
#39565=CARTESIAN_POINT('Ctrl Pts',(29.1961312382288,-8.9,135.889473684211));
#39566=CARTESIAN_POINT('Ctrl Pts',(29.40839202169,-8.9,135.8));
#39567=CARTESIAN_POINT('Ctrl Pts',(29.3358254989724,-8.9,135.825253490469));
#39568=CARTESIAN_POINT('Ctrl Pts',(29.2648784702771,-8.9,135.855159589645));
#39569=CARTESIAN_POINT('Ctrl Pts',(29.1961312382288,-8.9,135.889473684211));
#39570=CARTESIAN_POINT('Origin',(30.,-9.1,137.5));
#39571=CARTESIAN_POINT('',(28.2,-8.5,137.5));
#39572=CARTESIAN_POINT('',(28.2,-9.1,137.5));
#39573=CARTESIAN_POINT('',(31.1048119379707,-8.5,136.078947368421));
#39574=CARTESIAN_POINT('Origin',(30.,-8.5,137.5));
#39575=CARTESIAN_POINT('',(30.9949874371066,-8.5,136.));
#39576=CARTESIAN_POINT('Ctrl Pts',(30.9949874371066,-8.5,136.));
#39577=CARTESIAN_POINT('Ctrl Pts',(31.0325673132895,-8.5,136.024927669793));
#39578=CARTESIAN_POINT('Ctrl Pts',(31.0692099500079,-8.5,136.051268237865));
#39579=CARTESIAN_POINT('Ctrl Pts',(31.1048119379707,-8.5,136.078947368421));
#39580=CARTESIAN_POINT('',(29.0050125628934,-8.5,136.));
#39581=CARTESIAN_POINT('Ctrl Pts',(29.0050125628934,-8.5,136.));
#39582=CARTESIAN_POINT('Ctrl Pts',(29.0135741934101,-8.5,135.994320856796));
#39583=CARTESIAN_POINT('Ctrl Pts',(29.0221618811589,-8.49988793030325,135.988729425776));
#39584=CARTESIAN_POINT('Ctrl Pts',(29.0307750735035,-8.49967127651924,135.983225511632));
#39585=CARTESIAN_POINT('Ctrl Pts',(29.0424872389076,-8.49937667205062,135.975741323395));
#39586=CARTESIAN_POINT('Ctrl Pts',(29.0542337966699,-8.49890119353724,135.968423775377));
#39587=CARTESIAN_POINT('Ctrl Pts',(29.066042131988,-8.49823342511236,135.961258249725));
#39588=CARTESIAN_POINT('Ctrl Pts',(29.2076929772396,-8.49022298509104,135.875301784412));
#39589=CARTESIAN_POINT('Ctrl Pts',(29.3542317404519,-8.45928673703359,135.812713237712));
#39590=CARTESIAN_POINT('Ctrl Pts',(29.5016114139668,-8.42940336594084,135.770275800662));
#39591=CARTESIAN_POINT('Ctrl Pts',(29.5753012507243,-8.41446168039446,135.749057082136));
#39592=CARTESIAN_POINT('Ctrl Pts',(29.6492013150574,-8.39978321408925,135.732876141023));
#39593=CARTESIAN_POINT('Ctrl Pts',(29.7226173155667,-8.38828909107063,135.721416376084));
#39594=CARTESIAN_POINT('Ctrl Pts',(29.7960333160761,-8.37679496805201,135.709956611145));
#39595=CARTESIAN_POINT('Ctrl Pts',(29.8689652527616,-8.36848518831997,135.70321802238));
#39596=CARTESIAN_POINT('Ctrl Pts',(29.9419406646202,-8.36568846720679,135.700861053488));
#39597=CARTESIAN_POINT('Ctrl Pts',(29.9529448634599,-8.36526674056701,135.700505638511));
#39598=CARTESIAN_POINT('Ctrl Pts',(29.9639419471384,-8.36496215917836,135.700256622351));
#39599=CARTESIAN_POINT('Ctrl Pts',(29.9749386829878,-8.36477724654198,135.700102740572));
#39600=CARTESIAN_POINT('Ctrl Pts',(30.0208804218919,-8.3640047256615,135.699459859213));
#39601=CARTESIAN_POINT('Ctrl Pts',(30.0668878418323,-8.36543091711432,135.700630195523));
#39602=CARTESIAN_POINT('Ctrl Pts',(30.1127314030004,-8.36878946104138,135.703461047636));
#39603=CARTESIAN_POINT('Ctrl Pts',(30.3351972997306,-8.3850875292412,135.717198376017));
#39604=CARTESIAN_POINT('Ctrl Pts',(30.5671516888088,-8.45070494455055,135.774596783944));
#39605=CARTESIAN_POINT('Ctrl Pts',(30.7847295199563,-8.4825308206938,135.880027800313));
#39606=CARTESIAN_POINT('Ctrl Pts',(30.8209924918142,-8.48783513338434,135.897599636374));
#39607=CARTESIAN_POINT('Ctrl Pts',(30.8568561148407,-8.49220079220915,135.916505711559));
#39608=CARTESIAN_POINT('Ctrl Pts',(30.8918402206784,-8.49524200886307,135.936457835556));
#39609=CARTESIAN_POINT('Ctrl Pts',(30.9268243265161,-8.49828322551699,135.956409959553));
#39610=CARTESIAN_POINT('Ctrl Pts',(30.9609289151649,-8.5,135.977408132361));
#39611=CARTESIAN_POINT('Ctrl Pts',(30.9949874371066,-8.5,136.));
#39612=CARTESIAN_POINT('',(28.8951880620293,-8.5,136.078947368421));
#39613=CARTESIAN_POINT('Ctrl Pts',(28.8951880620293,-8.5,136.078947368421));
#39614=CARTESIAN_POINT('Ctrl Pts',(28.9307900499921,-8.5,136.051268237865));
#39615=CARTESIAN_POINT('Ctrl Pts',(28.9674326867105,-8.5,136.024927669793));
#39616=CARTESIAN_POINT('Ctrl Pts',(29.0050125628934,-8.5,136.));
#39617=CARTESIAN_POINT('Origin',(30.,-8.5,137.5));
#39618=CARTESIAN_POINT('Ctrl Pts',(28.9499455367427,-8.39129047171135,135.916983334517));
#39619=CARTESIAN_POINT('Ctrl Pts',(28.9583427274828,-8.39013445090615,135.911534549944));
#39620=CARTESIAN_POINT('Ctrl Pts',(28.966773453885,-8.38888037451443,135.90618177344));
#39621=CARTESIAN_POINT('Ctrl Pts',(28.9867484811824,-8.38570649135595,135.893774768811));
#39622=CARTESIAN_POINT('Ctrl Pts',(28.9983029277528,-8.38372333783055,135.886805685331));
#39623=CARTESIAN_POINT('Ctrl Pts',(29.1496188333912,-8.35575770442387,135.798384331373));
#39624=CARTESIAN_POINT('Ctrl Pts',(29.3692004391356,-8.28840055446218,135.713684542132));
#39625=CARTESIAN_POINT('Ctrl Pts',(29.6834526291903,-8.20996395514133,135.657893063385));
#39626=CARTESIAN_POINT('Ctrl Pts',(29.8489117254301,-8.18734058685009,135.646496412784));
#39627=CARTESIAN_POINT('Ctrl Pts',(29.9457556588889,-8.18293453051425,135.644194467675));
#39628=CARTESIAN_POINT('Ctrl Pts',(29.9584452353951,-8.1825139216413,135.643982887837));
#39629=CARTESIAN_POINT('Ctrl Pts',(30.0242680337758,-8.18121722147009,135.643309689515));
#39630=CARTESIAN_POINT('Ctrl Pts',(30.0774858946058,-8.1831094502482,135.644290152174));
#39631=CARTESIAN_POINT('Ctrl Pts',(30.384921872483,-8.21051184206819,135.658444492213));
#39632=CARTESIAN_POINT('Ctrl Pts',(30.6646630172529,-8.30783041470181,135.714213805079));
#39633=CARTESIAN_POINT('Ctrl Pts',(30.9494673877353,-8.37449857575747,135.855365180714));
#39634=CARTESIAN_POINT('Ctrl Pts',(31.0166500895793,-8.38669177291417,135.895307843082));
#39635=CARTESIAN_POINT('Ctrl Pts',(31.0500544632573,-8.39129047171135,135.916983334517));
#39636=CARTESIAN_POINT('Ctrl Pts',(28.9683012121263,-8.4275269811409,135.944655556345));
#39637=CARTESIAN_POINT('Ctrl Pts',(28.9767512906506,-8.42675709109451,135.939129896694));
#39638=CARTESIAN_POINT('Ctrl Pts',(28.9852390066968,-8.4258818399906,135.933697798623));
#39639=CARTESIAN_POINT('Ctrl Pts',(29.0053236866455,-8.42359861525567,135.921096795532));
#39640=CARTESIAN_POINT('Ctrl Pts',(29.0169525628858,-8.42211353739763,135.914012004032));
#39641=CARTESIAN_POINT('Ctrl Pts',(29.1689418008863,-8.40060124330269,135.824022942103));
#39642=CARTESIAN_POINT('Ctrl Pts',(29.3886577290161,-8.34023513638336,135.736269283873));
#39643=CARTESIAN_POINT('Ctrl Pts',(29.6966772130805,-8.26836461579283,135.677498762874));
#39644=CARTESIAN_POINT('Ctrl Pts',(29.8556490282664,-8.24775662303134,135.66541162577));
#39645=CARTESIAN_POINT('Ctrl Pts',(29.948172947781,-8.2437387547405,135.662972846865));
#39646=CARTESIAN_POINT('Ctrl Pts',(29.9603137751968,-8.24336666009415,135.662751533393));
#39647=CARTESIAN_POINT('Ctrl Pts',(30.0231268608963,-8.24214649464565,135.662025763747));
#39648=CARTESIAN_POINT('Ctrl Pts',(30.0740271395939,-8.24394907919365,135.66308988012));
#39649=CARTESIAN_POINT('Ctrl Pts',(30.3681174445248,-8.26856605876248,135.677985805289));
#39650=CARTESIAN_POINT('Ctrl Pts',(30.645085372046,-8.35906005048207,135.737526267015));
#39651=CARTESIAN_POINT('Ctrl Pts',(30.9305485522613,-8.41521263899238,135.882055224341));
#39652=CARTESIAN_POINT('Ctrl Pts',(30.9980718670533,-8.42441502706281,135.922670002529));
#39653=CARTESIAN_POINT('Ctrl Pts',(31.0316987878737,-8.4275269811409,135.944655556345));
#39654=CARTESIAN_POINT('Ctrl Pts',(28.9866568875098,-8.46376349057045,135.972327778172));
#39655=CARTESIAN_POINT('Ctrl Pts',(28.9951656302423,-8.46337735981164,135.966725510047));
#39656=CARTESIAN_POINT('Ctrl Pts',(29.0036963283471,-8.46288646482709,135.961213400593));
#39657=CARTESIAN_POINT('Ctrl Pts',(29.0239120334445,-8.4614845481509,135.948419296674));
#39658=CARTESIAN_POINT('Ctrl Pts',(29.0355841615369,-8.46051099397016,135.941217456675));
#39659=CARTESIAN_POINT('Ctrl Pts',(29.1883700097445,-8.44537944621221,135.849663173682));
#39660=CARTESIAN_POINT('Ctrl Pts',(29.4080438321775,-8.39198403108369,135.758834222622));
#39661=CARTESIAN_POINT('Ctrl Pts',(29.7098767955004,-8.32670408713254,135.697089500421));
#39662=CARTESIAN_POINT('Ctrl Pts',(29.8622279499253,-8.30806915213872,135.684302809393));
#39663=CARTESIAN_POINT('Ctrl Pts',(29.9505275745679,-8.30446251634076,135.681727259321));
#39664=CARTESIAN_POINT('Ctrl Pts',(29.9620734073366,-8.30410942072552,135.681487976795));
#39665=CARTESIAN_POINT('Ctrl Pts',(30.0220215947714,-8.30307545248594,135.680743784981));
#39666=CARTESIAN_POINT('Ctrl Pts',(30.0703465968442,-8.30459128816887,135.681830467577));
#39667=CARTESIAN_POINT('Ctrl Pts',(30.3520017276888,-8.32703331254691,135.69765706294));
#39668=CARTESIAN_POINT('Ctrl Pts',(30.6253883988622,-8.41041154465518,135.760850723329));
#39669=CARTESIAN_POINT('Ctrl Pts',(30.9116385733412,-8.45585238779906,135.908721743118));
#39670=CARTESIAN_POINT('Ctrl Pts',(30.9795071376909,-8.46227674585136,135.950045972915));
#39671=CARTESIAN_POINT('Ctrl Pts',(31.0133431124902,-8.46376349057045,135.972327778172));
#39672=CARTESIAN_POINT('Ctrl Pts',(29.0050125628934,-8.5,136.));
#39673=CARTESIAN_POINT('Ctrl Pts',(29.0135741934101,-8.5,135.994320856796));
#39674=CARTESIAN_POINT('Ctrl Pts',(29.0221618811589,-8.49988793030325,135.988729425776));
#39675=CARTESIAN_POINT('Ctrl Pts',(29.0424872389076,-8.49937667205062,135.975741323395));
#39676=CARTESIAN_POINT('Ctrl Pts',(29.0542337966699,-8.49890119353724,135.968423775377));
#39677=CARTESIAN_POINT('Ctrl Pts',(29.2076929772396,-8.49022298509104,135.875301784412));
#39678=CARTESIAN_POINT('Ctrl Pts',(29.4275011220581,-8.44381861300487,135.781418964363));
#39679=CARTESIAN_POINT('Ctrl Pts',(29.7231013793905,-8.38510474778405,135.71669519991));
#39680=CARTESIAN_POINT('Ctrl Pts',(29.8689652527616,-8.36848518831997,135.70321802238));
#39681=CARTESIAN_POINT('Ctrl Pts',(29.9529448634599,-8.36526674056701,135.700505638511));
#39682=CARTESIAN_POINT('Ctrl Pts',(29.9639419471384,-8.36496215917836,135.700256622351));
#39683=CARTESIAN_POINT('Ctrl Pts',(30.0208804218919,-8.3640047256615,135.699459859213));
#39684=CARTESIAN_POINT('Ctrl Pts',(30.0668878418323,-8.36543091711432,135.700630195523));
#39685=CARTESIAN_POINT('Ctrl Pts',(30.3351972997306,-8.3850875292412,135.717198376017));
#39686=CARTESIAN_POINT('Ctrl Pts',(30.6058107536552,-8.46164118043544,135.784163185266));
#39687=CARTESIAN_POINT('Ctrl Pts',(30.8927197378672,-8.49656645103397,135.935411786744));
#39688=CARTESIAN_POINT('Ctrl Pts',(30.9609289151649,-8.5,135.977408132361));
#39689=CARTESIAN_POINT('Ctrl Pts',(30.9949874371066,-8.5,136.));
#39690=CARTESIAN_POINT('',(28.9499455367427,-8.39129047171135,135.916983334517));
#39691=CARTESIAN_POINT('',(30.9949874371066,-8.5,136.));
#39692=CARTESIAN_POINT('Origin',(30.,-8.45,137.5));
#39693=CARTESIAN_POINT('',(31.1661903789691,-8.4,136.));
#39694=CARTESIAN_POINT('',(28.8951880620293,-8.5,136.078947368421));
#39695=CARTESIAN_POINT('Ctrl Pts',(31.0500544632573,-8.39129047171135,135.916983334517));
#39696=CARTESIAN_POINT('Ctrl Pts',(31.0899798051577,-8.39678689632762,135.942890163806));
#39697=CARTESIAN_POINT('Ctrl Pts',(31.1286105039774,-8.40000000009859,135.970783140825));
#39698=CARTESIAN_POINT('Ctrl Pts',(31.1661903807052,-8.4,136.00000000135));
#39699=CARTESIAN_POINT('Ctrl Pts',(31.0316987878737,-8.4275269811409,135.944655556345));
#39700=CARTESIAN_POINT('Ctrl Pts',(31.0708423080612,-8.43119126421841,135.970235999263));
#39701=CARTESIAN_POINT('Ctrl Pts',(31.1088103196971,-8.43333333339906,135.997611506775));
#39702=CARTESIAN_POINT('Ctrl Pts',(31.145730900342,-8.43333333333333,136.0263157908));
#39703=CARTESIAN_POINT('Ctrl Pts',(31.0133431124902,-8.46376349057045,135.972327778172));
#39704=CARTESIAN_POINT('Ctrl Pts',(31.0517048109648,-8.46559563210921,135.99758183472));
#39705=CARTESIAN_POINT('Ctrl Pts',(31.0890101354168,-8.46666666669953,136.024439872726));
#39706=CARTESIAN_POINT('Ctrl Pts',(31.1252714199787,-8.46666666666667,136.05263158025));
#39707=CARTESIAN_POINT('Ctrl Pts',(30.9949874371066,-8.5,136.));
#39708=CARTESIAN_POINT('Ctrl Pts',(31.0325673138683,-8.5,136.024927670177));
#39709=CARTESIAN_POINT('Ctrl Pts',(31.0692099511365,-8.5,136.051268238676));
#39710=CARTESIAN_POINT('Ctrl Pts',(31.1048119396155,-8.5,136.0789473697));
#39711=CARTESIAN_POINT('Ctrl Pts',(28.833809621031,-8.4,136.));
#39712=CARTESIAN_POINT('Ctrl Pts',(28.8713894972139,-8.4,135.970783139968));
#39713=CARTESIAN_POINT('Ctrl Pts',(28.9100201954571,-8.39678689624297,135.942890163407));
#39714=CARTESIAN_POINT('Ctrl Pts',(28.9499455367427,-8.39129047171135,135.916983334517));
#39715=CARTESIAN_POINT('Ctrl Pts',(28.8542691013637,-8.43333333333333,136.026315789474));
#39716=CARTESIAN_POINT('Ctrl Pts',(28.8911896814733,-8.43333333333333,135.997611505934));
#39717=CARTESIAN_POINT('Ctrl Pts',(28.9291576925416,-8.43119126416198,135.970235998869));
#39718=CARTESIAN_POINT('Ctrl Pts',(28.9683012121263,-8.4275269811409,135.944655556345));
#39719=CARTESIAN_POINT('Ctrl Pts',(28.8747285816965,-8.46666666666667,136.052631578947));
#39720=CARTESIAN_POINT('Ctrl Pts',(28.9109898657327,-8.46666666666667,136.024439871899));
#39721=CARTESIAN_POINT('Ctrl Pts',(28.948295189626,-8.46559563208099,135.997581834331));
#39722=CARTESIAN_POINT('Ctrl Pts',(28.9866568875098,-8.46376349057045,135.972327778172));
#39723=CARTESIAN_POINT('Ctrl Pts',(28.8951880620293,-8.5,136.078947368421));
#39724=CARTESIAN_POINT('Ctrl Pts',(28.9307900499921,-8.5,136.051268237865));
#39725=CARTESIAN_POINT('Ctrl Pts',(28.9674326867105,-8.5,136.024927669793));
#39726=CARTESIAN_POINT('Ctrl Pts',(29.0050125628934,-8.5,136.));
#39727=CARTESIAN_POINT('Origin',(-37.95,8.2,135.8));
#39728=CARTESIAN_POINT('',(-38.,8.90000000000001,135.8));
#39729=CARTESIAN_POINT('',(-37.9,9.,135.8));
#39730=CARTESIAN_POINT('',(-38.,8.90000000000001,135.8));
#39731=CARTESIAN_POINT('',(-37.9,8.2,135.));
#39732=CARTESIAN_POINT('Origin',(-37.9,8.2,135.8));
#39733=CARTESIAN_POINT('',(-38.,8.2,135.1));
#39734=CARTESIAN_POINT('',(-37.9,8.2,135.));
#39735=CARTESIAN_POINT('Origin',(-38.,8.2,135.8));
#39736=CARTESIAN_POINT('Origin',(-37.95,8.95,137.5));
#39737=CARTESIAN_POINT('',(-38.,8.9,144.2));
#39738=CARTESIAN_POINT('',(-37.9,9.,144.2));
#39739=CARTESIAN_POINT('',(-38.,8.9,144.2));
#39740=CARTESIAN_POINT('',(-37.9,9.,137.5));
#39741=CARTESIAN_POINT('',(-38.,8.9,137.5));
#39742=CARTESIAN_POINT('Origin',(-37.95,8.2,144.2));
#39743=CARTESIAN_POINT('',(-38.,8.2,144.9));
#39744=CARTESIAN_POINT('',(-37.9,8.2,145.));
#39745=CARTESIAN_POINT('',(-38.,8.2,144.9));
#39746=CARTESIAN_POINT('Origin',(-37.9,8.2,144.2));
#39747=CARTESIAN_POINT('Origin',(-38.,8.2,144.2));
#39748=CARTESIAN_POINT('Origin',(-37.95,7.75,144.95));
#39749=CARTESIAN_POINT('',(-38.,4.8,144.9));
#39750=CARTESIAN_POINT('',(-37.9,4.8,145.));
#39751=CARTESIAN_POINT('',(-38.,4.8,144.9));
#39752=CARTESIAN_POINT('',(-37.9,7.75,145.));
#39753=CARTESIAN_POINT('',(-38.,7.75,144.9));
#39754=CARTESIAN_POINT('Origin',(-37.95,4.8,144.2));
#39755=CARTESIAN_POINT('',(-38.,4.09999999999999,144.2));
#39756=CARTESIAN_POINT('',(-38.,4.09999999999999,144.2));
#39757=CARTESIAN_POINT('Origin',(-37.9,4.8,144.2));
#39758=CARTESIAN_POINT('Origin',(-38.,4.8,144.2));
#39759=CARTESIAN_POINT('Origin',(-37.95,4.05,142.5));
#39760=CARTESIAN_POINT('',(-38.,4.1,135.8));
#39761=CARTESIAN_POINT('',(-38.,4.1,135.8));
#39762=CARTESIAN_POINT('',(-38.,4.1,142.5));
#39763=CARTESIAN_POINT('Origin',(-37.95,4.8,135.8));
#39764=CARTESIAN_POINT('',(-38.,4.8,135.1));
#39765=CARTESIAN_POINT('',(-37.9,4.8,135.));
#39766=CARTESIAN_POINT('',(-38.,4.8,135.1));
#39767=CARTESIAN_POINT('Origin',(-37.9,4.8,135.8));
#39768=CARTESIAN_POINT('Origin',(-38.,4.8,135.8));
#39769=CARTESIAN_POINT('Origin',(-37.95,5.25,135.05));
#39770=CARTESIAN_POINT('',(-37.9,5.25,135.));
#39771=CARTESIAN_POINT('',(-38.,5.25,135.1));
#39772=CARTESIAN_POINT('Origin',(-38.,4.8,135.8));
#39773=CARTESIAN_POINT('',(-25.8,4.8,135.));
#39774=CARTESIAN_POINT('',(-38.,4.8,135.));
#39775=CARTESIAN_POINT('',(-38.,4.8,135.));
#39776=CARTESIAN_POINT('',(37.9,4.8,135.));
#39777=CARTESIAN_POINT('',(-38.,4.8,135.));
#39778=CARTESIAN_POINT('Origin',(37.9,4.8,135.8));
#39779=CARTESIAN_POINT('Origin',(-38.,4.,135.));
#39780=CARTESIAN_POINT('',(-25.8,8.2,135.));
#39781=CARTESIAN_POINT('',(-38.,8.2,135.));
#39782=CARTESIAN_POINT('',(-25.8,6.5,135.));
#39783=CARTESIAN_POINT('Origin',(-38.,8.2,135.8));
#39784=CARTESIAN_POINT('',(-30.8485281374239,9.,135.8));
#39785=CARTESIAN_POINT('',(-38.,9.,135.8));
#39786=CARTESIAN_POINT('',(-30.62442393624,8.99442305443429,135.70570254201));
#39787=CARTESIAN_POINT('Ctrl Pts',(-30.62442393624,8.99442305443429,135.70570254201));
#39788=CARTESIAN_POINT('Ctrl Pts',(-30.7010733797628,8.99756721057679,135.732190956222));
#39789=CARTESIAN_POINT('Ctrl Pts',(-30.7759616147067,9.,135.763779566847));
#39790=CARTESIAN_POINT('Ctrl Pts',(-30.8485281374239,9.,135.8));
#39791=CARTESIAN_POINT('',(-29.37557606376,8.99442305443429,135.70570254201));
#39792=CARTESIAN_POINT('Ctrl Pts',(-29.37557606376,8.99442305443429,135.70570254201));
#39793=CARTESIAN_POINT('Ctrl Pts',(-29.3968663992163,8.99354972599348,135.698345055793));
#39794=CARTESIAN_POINT('Ctrl Pts',(-29.418327451187,8.9926309002887,135.691382459919));
#39795=CARTESIAN_POINT('Ctrl Pts',(-29.5876626138109,8.9849459908676,135.639432675438));
#39796=CARTESIAN_POINT('Ctrl Pts',(-29.8198774693527,8.97481364719588,135.600649477793));
#39797=CARTESIAN_POINT('Ctrl Pts',(-30.1802232821902,8.97487183787893,135.600774173325));
#39798=CARTESIAN_POINT('Ctrl Pts',(-30.4123094665995,8.98495128128084,135.639444028187));
#39799=CARTESIAN_POINT('Ctrl Pts',(-30.5816752394099,8.99263100796461,135.691382689721));
#39800=CARTESIAN_POINT('Ctrl Pts',(-30.6031336007837,8.99354972599348,135.698345055793));
#39801=CARTESIAN_POINT('Ctrl Pts',(-30.62442393624,8.99442305443429,135.70570254201));
#39802=CARTESIAN_POINT('',(-29.1514718625761,9.,135.8));
#39803=CARTESIAN_POINT('Ctrl Pts',(-29.1514718625749,9.,135.800000000001));
#39804=CARTESIAN_POINT('Ctrl Pts',(-29.2240383852925,9.00000000000003,135.763779566847));
#39805=CARTESIAN_POINT('Ctrl Pts',(-29.2989266202368,8.99756721057681,135.732190956222));
#39806=CARTESIAN_POINT('Ctrl Pts',(-29.37557606376,8.99442305443429,135.70570254201));
#39807=CARTESIAN_POINT('',(29.1514718625761,9.,135.8));
#39808=CARTESIAN_POINT('',(-38.,9.,135.8));
#39809=CARTESIAN_POINT('',(29.37557606376,8.99442305443429,135.70570254201));
#39810=CARTESIAN_POINT('Ctrl Pts',(29.37557606376,8.99442305443429,135.70570254201));
#39811=CARTESIAN_POINT('Ctrl Pts',(29.2989266202372,8.99756721057679,135.732190956222));
#39812=CARTESIAN_POINT('Ctrl Pts',(29.2240383852933,9.,135.763779566847));
#39813=CARTESIAN_POINT('Ctrl Pts',(29.1514718625761,9.,135.8));
#39814=CARTESIAN_POINT('',(30.62442393624,8.99442305443429,135.70570254201));
#39815=CARTESIAN_POINT('Ctrl Pts',(30.62442393624,8.99442305443429,135.70570254201));
#39816=CARTESIAN_POINT('Ctrl Pts',(30.6031336007837,8.99354972599348,135.698345055793));
#39817=CARTESIAN_POINT('Ctrl Pts',(30.581672548813,8.99263090028869,135.69138245992));
#39818=CARTESIAN_POINT('Ctrl Pts',(30.4123373861891,8.9849459908676,135.639432675438));
#39819=CARTESIAN_POINT('Ctrl Pts',(30.1801225306472,8.97481364719588,135.600649477793));
#39820=CARTESIAN_POINT('Ctrl Pts',(29.8197767178098,8.97487183787893,135.600774173325));
#39821=CARTESIAN_POINT('Ctrl Pts',(29.5876905334005,8.98495128128084,135.639444028187));
#39822=CARTESIAN_POINT('Ctrl Pts',(29.4183247605901,8.99263100796461,135.691382689721));
#39823=CARTESIAN_POINT('Ctrl Pts',(29.3968663992163,8.99354972599348,135.698345055793));
#39824=CARTESIAN_POINT('Ctrl Pts',(29.37557606376,8.99442305443429,135.70570254201));
#39825=CARTESIAN_POINT('',(30.8485281374239,9.,135.8));
#39826=CARTESIAN_POINT('Ctrl Pts',(30.8485281374252,9.,135.800000000001));
#39827=CARTESIAN_POINT('Ctrl Pts',(30.7759616147075,9.00000000000003,135.763779566847));
#39828=CARTESIAN_POINT('Ctrl Pts',(30.7010733797633,8.99756721057681,135.732190956222));
#39829=CARTESIAN_POINT('Ctrl Pts',(30.62442393624,8.99442305443429,135.70570254201));
#39830=CARTESIAN_POINT('',(37.9,9.,135.8));
#39831=CARTESIAN_POINT('',(-38.,9.,135.8));
#39832=CARTESIAN_POINT('',(37.9,8.2,135.));
#39833=CARTESIAN_POINT('Origin',(37.9,8.2,135.8));
#39834=CARTESIAN_POINT('',(-38.,8.2,135.));
#39835=CARTESIAN_POINT('',(-38.,8.2,135.));
#39836=CARTESIAN_POINT('Origin',(-38.,6.5,140.));
#39837=CARTESIAN_POINT('',(-38.,8.5,144.));
#39838=CARTESIAN_POINT('',(-38.,8.5,136.));
#39839=CARTESIAN_POINT('',(-38.,8.5,142.2));
#39840=CARTESIAN_POINT('',(-38.,8.,144.5));
#39841=CARTESIAN_POINT('Origin',(-38.,8.,144.));
#39842=CARTESIAN_POINT('',(-38.,5.,144.5));
#39843=CARTESIAN_POINT('',(-38.,5.55,144.5));
#39844=CARTESIAN_POINT('',(-38.,4.5,144.));
#39845=CARTESIAN_POINT('Origin',(-38.,5.,144.));
#39846=CARTESIAN_POINT('',(-38.,4.50000000000002,136.));
#39847=CARTESIAN_POINT('',(-38.,4.5,137.8));
#39848=CARTESIAN_POINT('',(-38.,5.,135.5));
#39849=CARTESIAN_POINT('Origin',(-38.,5.,136.));
#39850=CARTESIAN_POINT('',(-38.,8.,135.5));
#39851=CARTESIAN_POINT('',(-38.,7.45,135.5));
#39852=CARTESIAN_POINT('Origin',(-38.,8.,136.));
#39853=CARTESIAN_POINT('Origin',(37.95,8.2,135.8));
#39854=CARTESIAN_POINT('',(38.,8.2,135.1));
#39855=CARTESIAN_POINT('',(38.,8.2,135.1));
#39856=CARTESIAN_POINT('',(38.,8.90000000000001,135.8));
#39857=CARTESIAN_POINT('',(37.9,9.,135.8));
#39858=CARTESIAN_POINT('Origin',(38.,8.2,135.8));
#39859=CARTESIAN_POINT('Origin',(37.95,5.25,135.05));
#39860=CARTESIAN_POINT('',(38.,4.8,135.1));
#39861=CARTESIAN_POINT('',(38.,5.25,135.1));
#39862=CARTESIAN_POINT('',(38.,4.8,135.1));
#39863=CARTESIAN_POINT('',(37.9,5.25,135.));
#39864=CARTESIAN_POINT('Origin',(37.95,4.8,135.8));
#39865=CARTESIAN_POINT('',(38.,4.09999999999999,135.8));
#39866=CARTESIAN_POINT('',(38.,4.09999999999999,135.8));
#39867=CARTESIAN_POINT('Origin',(38.,4.8,135.8));
#39868=CARTESIAN_POINT('Origin',(37.95,4.05,142.5));
#39869=CARTESIAN_POINT('',(38.,4.1,144.2));
#39870=CARTESIAN_POINT('',(38.,4.1,142.5));
#39871=CARTESIAN_POINT('',(38.,4.1,144.2));
#39872=CARTESIAN_POINT('Origin',(37.95,4.8,144.2));
#39873=CARTESIAN_POINT('',(38.,4.8,144.9));
#39874=CARTESIAN_POINT('',(37.9,4.8,145.));
#39875=CARTESIAN_POINT('',(38.,4.8,144.9));
#39876=CARTESIAN_POINT('Origin',(37.9,4.8,144.2));
#39877=CARTESIAN_POINT('Origin',(38.,4.8,144.2));
#39878=CARTESIAN_POINT('Origin',(37.95,7.75,144.95));
#39879=CARTESIAN_POINT('',(38.,8.2,144.9));
#39880=CARTESIAN_POINT('',(38.,7.75,144.9));
#39881=CARTESIAN_POINT('',(37.9,8.2,145.));
#39882=CARTESIAN_POINT('',(38.,8.2,144.9));
#39883=CARTESIAN_POINT('',(37.9,7.75,145.));
#39884=CARTESIAN_POINT('Origin',(37.95,8.2,144.2));
#39885=CARTESIAN_POINT('',(38.,8.90000000000001,144.2));
#39886=CARTESIAN_POINT('',(37.9,9.,144.2));
#39887=CARTESIAN_POINT('',(38.,8.90000000000001,144.2));
#39888=CARTESIAN_POINT('Origin',(37.9,8.2,144.2));
#39889=CARTESIAN_POINT('Origin',(38.,8.2,144.2));
#39890=CARTESIAN_POINT('Origin',(37.95,8.95,137.5));
#39891=CARTESIAN_POINT('',(38.,8.9,137.5));
#39892=CARTESIAN_POINT('',(37.9,9.,137.5));
#39893=CARTESIAN_POINT('Origin',(-38.,9.,145.));
#39894=CARTESIAN_POINT('',(-38.,4.8,145.));
#39895=CARTESIAN_POINT('',(-38.,8.2,145.));
#39896=CARTESIAN_POINT('Origin',(-38.,8.2,144.2));
#39897=CARTESIAN_POINT('',(30.8485281374239,9.,144.2));
#39898=CARTESIAN_POINT('',(-38.,9.,144.2));
#39899=CARTESIAN_POINT('',(30.62442393624,8.99442305443429,144.29429745799));
#39900=CARTESIAN_POINT('Ctrl Pts',(30.62442393624,8.99442305443429,144.29429745799));
#39901=CARTESIAN_POINT('Ctrl Pts',(30.7010733797628,8.99756721057679,144.267809043778));
#39902=CARTESIAN_POINT('Ctrl Pts',(30.7759616147067,9.,144.236220433153));
#39903=CARTESIAN_POINT('Ctrl Pts',(30.8485281374239,9.,144.2));
#39904=CARTESIAN_POINT('',(29.37557606376,8.99442305443429,144.29429745799));
#39905=CARTESIAN_POINT('Ctrl Pts',(29.37557606376,8.99442305443429,144.29429745799));
#39906=CARTESIAN_POINT('Ctrl Pts',(29.3968663992163,8.99354972599348,144.301654944207));
#39907=CARTESIAN_POINT('Ctrl Pts',(29.418327449872,8.99263089654327,144.308617544038));
#39908=CARTESIAN_POINT('Ctrl Pts',(29.587662650504,8.98494611755363,144.360567193318));
#39909=CARTESIAN_POINT('Ctrl Pts',(29.8198775424307,8.97481395248941,144.39935020957));
#39910=CARTESIAN_POINT('Ctrl Pts',(30.180223294947,8.97487213269987,144.399225510548));
#39911=CARTESIAN_POINT('Ctrl Pts',(30.4123094590021,8.98495141076798,144.360555832908));
#39912=CARTESIAN_POINT('Ctrl Pts',(30.5816752399674,8.99263100404222,144.308617314527));
#39913=CARTESIAN_POINT('Ctrl Pts',(30.6031336007836,8.99354972599347,144.301654944207));
#39914=CARTESIAN_POINT('Ctrl Pts',(30.62442393624,8.99442305443429,144.29429745799));
#39915=CARTESIAN_POINT('',(29.1514718625761,9.,144.2));
#39916=CARTESIAN_POINT('Ctrl Pts',(29.1514718625749,9.,144.199999999999));
#39917=CARTESIAN_POINT('Ctrl Pts',(29.2240383852925,9.00000000000003,144.236220433153));
#39918=CARTESIAN_POINT('Ctrl Pts',(29.2989266202368,8.99756721057681,144.267809043778));
#39919=CARTESIAN_POINT('Ctrl Pts',(29.37557606376,8.99442305443429,144.29429745799));
#39920=CARTESIAN_POINT('',(-29.1514718625761,9.,144.2));
#39921=CARTESIAN_POINT('',(-38.,9.,144.2));
#39922=CARTESIAN_POINT('',(-29.37557606376,8.99442305443429,144.29429745799));
#39923=CARTESIAN_POINT('Ctrl Pts',(-29.37557606376,8.99442305443429,144.29429745799));
#39924=CARTESIAN_POINT('Ctrl Pts',(-29.2989266202372,8.99756721057679,144.267809043778));
#39925=CARTESIAN_POINT('Ctrl Pts',(-29.2240383852933,9.,144.236220433153));
#39926=CARTESIAN_POINT('Ctrl Pts',(-29.1514718625761,9.,144.2));
#39927=CARTESIAN_POINT('',(-30.62442393624,8.99442305443429,144.29429745799));
#39928=CARTESIAN_POINT('Ctrl Pts',(-30.62442393624,8.99442305443429,144.29429745799));
#39929=CARTESIAN_POINT('Ctrl Pts',(-30.6031336007837,8.99354972599348,144.301654944207));
#39930=CARTESIAN_POINT('Ctrl Pts',(-30.5816983343123,8.99261835182926,144.308632644433));
#39931=CARTESIAN_POINT('Ctrl Pts',(-30.4860772057434,8.98837707594693,144.337802199667));
#39932=CARTESIAN_POINT('Ctrl Pts',(-30.3737546351539,8.98306099714656,144.364880756376));
#39933=CARTESIAN_POINT('Ctrl Pts',(-30.1448589551985,8.97549033242365,144.39734513884));
#39934=CARTESIAN_POINT('Ctrl Pts',(-29.8570704543082,8.97294630891696,144.405692333025));
#39935=CARTESIAN_POINT('Ctrl Pts',(-29.5879618888624,8.98495073555583,144.36060019061));
#39936=CARTESIAN_POINT('Ctrl Pts',(-29.4183017778428,8.99262938553082,144.308615224025));
#39937=CARTESIAN_POINT('Ctrl Pts',(-29.3968663992163,8.99354972599348,144.301654944207));
#39938=CARTESIAN_POINT('Ctrl Pts',(-29.37557606376,8.99442305443429,144.29429745799));
#39939=CARTESIAN_POINT('',(-30.8485281374239,9.,144.2));
#39940=CARTESIAN_POINT('Ctrl Pts',(-30.8485281374251,9.,144.199999999999));
#39941=CARTESIAN_POINT('Ctrl Pts',(-30.7759616147075,9.00000000000003,144.236220433153));
#39942=CARTESIAN_POINT('Ctrl Pts',(-30.7010733797632,8.99756721057681,144.267809043778));
#39943=CARTESIAN_POINT('Ctrl Pts',(-30.62442393624,8.99442305443429,144.29429745799));
#39944=CARTESIAN_POINT('',(-38.,9.,144.2));
#39945=CARTESIAN_POINT('Origin',(-38.,9.,135.));
#39946=CARTESIAN_POINT('Origin',(-30.,9.,142.5));
#39947=CARTESIAN_POINT('Origin',(30.,9.,142.5));
#39948=CARTESIAN_POINT('Origin',(30.,9.,137.5));
#39949=CARTESIAN_POINT('Origin',(-30.,9.,137.5));
#39950=CARTESIAN_POINT('Origin',(38.,6.5,140.));
#39951=CARTESIAN_POINT('',(38.,8.5,136.));
#39952=CARTESIAN_POINT('',(38.,8.5,144.));
#39953=CARTESIAN_POINT('',(38.,8.5,142.2));
#39954=CARTESIAN_POINT('',(38.,8.,135.5));
#39955=CARTESIAN_POINT('Origin',(38.,8.,136.));
#39956=CARTESIAN_POINT('',(38.,5.,135.5));
#39957=CARTESIAN_POINT('',(38.,7.45,135.5));
#39958=CARTESIAN_POINT('',(38.,4.50000000000002,136.));
#39959=CARTESIAN_POINT('Origin',(38.,5.,136.));
#39960=CARTESIAN_POINT('',(38.,4.5,144.));
#39961=CARTESIAN_POINT('',(38.,4.5,137.8));
#39962=CARTESIAN_POINT('',(38.,5.,144.5));
#39963=CARTESIAN_POINT('Origin',(38.,5.,144.));
#39964=CARTESIAN_POINT('',(38.,8.,144.5));
#39965=CARTESIAN_POINT('',(38.,5.55,144.5));
#39966=CARTESIAN_POINT('Origin',(38.,8.,144.));
#39967=CARTESIAN_POINT('Ctrl Pts',(30.62442393624,8.99442305443429,144.29429745799));
#39968=CARTESIAN_POINT('Ctrl Pts',(30.6031336007836,8.99354972599347,144.301654944207));
#39969=CARTESIAN_POINT('Ctrl Pts',(30.5816752399674,8.99263100404222,144.308617314527));
#39970=CARTESIAN_POINT('Ctrl Pts',(30.4123094590021,8.98495141076798,144.360555832908));
#39971=CARTESIAN_POINT('Ctrl Pts',(30.180223294947,8.97487213269987,144.399225510548));
#39972=CARTESIAN_POINT('Ctrl Pts',(29.8198775424307,8.97481395248941,144.39935020957));
#39973=CARTESIAN_POINT('Ctrl Pts',(29.587662650504,8.98494611755363,144.360567193318));
#39974=CARTESIAN_POINT('Ctrl Pts',(29.418327449872,8.99263089654327,144.308617544038));
#39975=CARTESIAN_POINT('Ctrl Pts',(29.3968663992163,8.99354972599348,144.301654944207));
#39976=CARTESIAN_POINT('Ctrl Pts',(29.37557606376,8.99442305443429,144.29429745799));
#39977=CARTESIAN_POINT('Ctrl Pts',(30.6134852835967,8.96294870295619,144.262864971993));
#39978=CARTESIAN_POINT('Ctrl Pts',(30.592658514685,8.96237089086999,144.270081701427));
#39979=CARTESIAN_POINT('Ctrl Pts',(30.5716540376503,8.96172231088449,144.276909831782));
#39980=CARTESIAN_POINT('Ctrl Pts',(30.4057626992984,8.95618706951869,144.328010039787));
#39981=CARTESIAN_POINT('Ctrl Pts',(30.177480927785,8.94781793441349,144.366475382318));
#39982=CARTESIAN_POINT('Ctrl Pts',(29.8226192450814,8.94775833832967,144.366598850003));
#39983=CARTESIAN_POINT('Ctrl Pts',(29.5942100303878,8.95618270846843,144.328022210868));
#39984=CARTESIAN_POINT('Ctrl Pts',(29.4283485312412,8.96172203294744,144.276909913069));
#39985=CARTESIAN_POINT('Ctrl Pts',(29.4073415857357,8.96237102991341,144.270081822348));
#39986=CARTESIAN_POINT('Ctrl Pts',(29.3865147164033,8.96294870295619,144.262864971993));
#39987=CARTESIAN_POINT('Ctrl Pts',(30.6025466309533,8.9314743514781,144.231432485997));
#39988=CARTESIAN_POINT('Ctrl Pts',(30.5821847854831,8.93117883512348,144.238497937231));
#39989=CARTESIAN_POINT('Ctrl Pts',(30.5616314871845,8.93082738132286,144.245213391643));
#39990=CARTESIAN_POINT('Ctrl Pts',(30.3992200209108,8.92734726636692,144.295401442766));
#39991=CARTESIAN_POINT('Ctrl Pts',(30.1747360622273,8.92072288323236,144.333695864957));
#39992=CARTESIAN_POINT('Ctrl Pts',(29.8253608556981,8.92068647619822,144.333827818585));
#39993=CARTESIAN_POINT('Ctrl Pts',(29.6007527390699,8.92734289454247,144.295412539047));
#39994=CARTESIAN_POINT('Ctrl Pts',(29.4383712011633,8.93082748179126,144.245213780592));
#39995=CARTESIAN_POINT('Ctrl Pts',(29.4178151140962,8.93117869608006,144.238497816309));
#39996=CARTESIAN_POINT('Ctrl Pts',(29.3974533690467,8.9314743514781,144.231432485996));
#39997=CARTESIAN_POINT('Ctrl Pts',(30.59160797831,8.9,144.2));
#39998=CARTESIAN_POINT('Ctrl Pts',(30.5717096993845,8.9,144.206924694451));
#39999=CARTESIAN_POINT('Ctrl Pts',(30.5516102848674,8.89991868816513,144.213505908897));
#40000=CARTESIAN_POINT('Ctrl Pts',(30.3926732612071,8.89858292511763,144.262855649644));
#40001=CARTESIAN_POINT('Ctrl Pts',(30.1719936950654,8.89366868494597,144.300945736727));
#40002=CARTESIAN_POINT('Ctrl Pts',(29.8281025583487,8.89363086203848,144.301076459018));
#40003=CARTESIAN_POINT('Ctrl Pts',(29.6073001189537,8.89857948545727,144.262867556597));
#40004=CARTESIAN_POINT('Ctrl Pts',(29.4483922825326,8.89991861819543,144.213506149622));
#40005=CARTESIAN_POINT('Ctrl Pts',(29.4282903006156,8.9,144.206924694451));
#40006=CARTESIAN_POINT('Ctrl Pts',(29.40839202169,8.9,144.2));
#40007=CARTESIAN_POINT('',(29.40839202169,8.9,144.2));
#40008=CARTESIAN_POINT('',(29.40839202169,8.9,144.2));
#40009=CARTESIAN_POINT('',(30.59160797831,8.9,144.2));
#40010=CARTESIAN_POINT('',(30.62442393624,8.99442305443429,144.29429745799));
#40011=CARTESIAN_POINT('Ctrl Pts',(30.59160797831,8.9,144.2));
#40012=CARTESIAN_POINT('Ctrl Pts',(30.5717096993845,8.9,144.206924694451));
#40013=CARTESIAN_POINT('Ctrl Pts',(30.5516102848674,8.89991868816513,144.213505908897));
#40014=CARTESIAN_POINT('Ctrl Pts',(30.3926732612071,8.89858292511763,144.262855649644));
#40015=CARTESIAN_POINT('Ctrl Pts',(30.1719936950654,8.89366868494597,144.300945736727));
#40016=CARTESIAN_POINT('Ctrl Pts',(29.8281025583487,8.89363086203848,144.301076459018));
#40017=CARTESIAN_POINT('Ctrl Pts',(29.6073001189537,8.89857948545727,144.262867556597));
#40018=CARTESIAN_POINT('Ctrl Pts',(29.4483922825326,8.89991861819543,144.213506149622));
#40019=CARTESIAN_POINT('Ctrl Pts',(29.4282903006156,8.9,144.206924694451));
#40020=CARTESIAN_POINT('Ctrl Pts',(29.40839202169,8.9,144.2));
#40021=CARTESIAN_POINT('Origin',(30.,8.95,142.5));
#40022=CARTESIAN_POINT('',(29.19613123823,8.9,144.110526315789));
#40023=CARTESIAN_POINT('',(29.1514718625761,9.,144.2));
#40024=CARTESIAN_POINT('',(28.2,8.9,142.5));
#40025=CARTESIAN_POINT('Origin',(30.,8.9,142.5));
#40026=CARTESIAN_POINT('',(30.80386876177,8.9,144.110526315789));
#40027=CARTESIAN_POINT('Origin',(30.,8.9,142.5));
#40028=CARTESIAN_POINT('',(30.80386876177,8.9,144.110526315789));
#40029=CARTESIAN_POINT('Ctrl Pts',(29.37557606376,8.99442305443429,144.29429745799));
#40030=CARTESIAN_POINT('Ctrl Pts',(29.2989266202368,8.99756721057681,144.267809043778));
#40031=CARTESIAN_POINT('Ctrl Pts',(29.2240383852925,9.00000000000003,144.236220433153));
#40032=CARTESIAN_POINT('Ctrl Pts',(29.1514718625749,9.,144.199999999999));
#40033=CARTESIAN_POINT('Ctrl Pts',(29.3865147164033,8.96294870295619,144.262864971993));
#40034=CARTESIAN_POINT('Ctrl Pts',(29.311226246482,8.96504480705121,144.236788199029));
#40035=CARTESIAN_POINT('Ctrl Pts',(29.237651746954,8.96666666666668,144.205760425554));
#40036=CARTESIAN_POINT('Ctrl Pts',(29.1663583211262,8.96666666666667,144.170175438596));
#40037=CARTESIAN_POINT('Ctrl Pts',(29.3974533690467,8.9314743514781,144.231432485997));
#40038=CARTESIAN_POINT('Ctrl Pts',(29.3235258727272,8.9325224035256,144.20576735428));
#40039=CARTESIAN_POINT('Ctrl Pts',(29.2512651086156,8.93333333333334,144.175300417955));
#40040=CARTESIAN_POINT('Ctrl Pts',(29.1812447796775,8.93333333333333,144.140350877192));
#40041=CARTESIAN_POINT('Ctrl Pts',(29.40839202169,8.9,144.2));
#40042=CARTESIAN_POINT('Ctrl Pts',(29.3358254989724,8.9,144.174746509531));
#40043=CARTESIAN_POINT('Ctrl Pts',(29.2648784702771,8.9,144.144840410355));
#40044=CARTESIAN_POINT('Ctrl Pts',(29.1961312382288,8.9,144.110526315789));
#40045=CARTESIAN_POINT('Ctrl Pts',(29.40839202169,8.9,144.2));
#40046=CARTESIAN_POINT('Ctrl Pts',(29.3358254989724,8.9,144.174746509531));
#40047=CARTESIAN_POINT('Ctrl Pts',(29.2648784702771,8.9,144.144840410355));
#40048=CARTESIAN_POINT('Ctrl Pts',(29.1961312382288,8.9,144.110526315789));
#40049=CARTESIAN_POINT('Ctrl Pts',(30.8485281374239,9.,144.2));
#40050=CARTESIAN_POINT('Ctrl Pts',(30.7759616147067,9.,144.236220433153));
#40051=CARTESIAN_POINT('Ctrl Pts',(30.7010733797628,8.99756721057679,144.267809043778));
#40052=CARTESIAN_POINT('Ctrl Pts',(30.62442393624,8.99442305443429,144.29429745799));
#40053=CARTESIAN_POINT('Ctrl Pts',(30.8336416788726,8.96666666666667,144.170175438596));
#40054=CARTESIAN_POINT('Ctrl Pts',(30.7623482530451,8.96666666666667,144.205760425554));
#40055=CARTESIAN_POINT('Ctrl Pts',(30.6887737535176,8.96504480705119,144.236788199029));
#40056=CARTESIAN_POINT('Ctrl Pts',(30.6134852835966,8.96294870295619,144.262864971993));
#40057=CARTESIAN_POINT('Ctrl Pts',(30.8187552203213,8.93333333333333,144.140350877193));
#40058=CARTESIAN_POINT('Ctrl Pts',(30.7487348913836,8.93333333333333,144.175300417955));
#40059=CARTESIAN_POINT('Ctrl Pts',(30.6764741272724,8.9325224035256,144.20576735428));
#40060=CARTESIAN_POINT('Ctrl Pts',(30.6025466309533,8.9314743514781,144.231432485997));
#40061=CARTESIAN_POINT('Ctrl Pts',(30.80386876177,8.9,144.110526315789));
#40062=CARTESIAN_POINT('Ctrl Pts',(30.7351215297221,8.9,144.144840410356));
#40063=CARTESIAN_POINT('Ctrl Pts',(30.6641745010272,8.9,144.174746509531));
#40064=CARTESIAN_POINT('Ctrl Pts',(30.59160797831,8.9,144.2));
#40065=CARTESIAN_POINT('Ctrl Pts',(30.80386876177,8.9,144.110526315789));
#40066=CARTESIAN_POINT('Ctrl Pts',(30.7351215297221,8.9,144.144840410356));
#40067=CARTESIAN_POINT('Ctrl Pts',(30.6641745010272,8.9,144.174746509531));
#40068=CARTESIAN_POINT('Ctrl Pts',(30.59160797831,8.9,144.2));
#40069=CARTESIAN_POINT('Origin',(30.,9.1,142.5));
#40070=CARTESIAN_POINT('',(28.2,8.5,142.5));
#40071=CARTESIAN_POINT('',(28.2,9.1,142.5));
#40072=CARTESIAN_POINT('',(31.1048119379707,8.5,143.921052631579));
#40073=CARTESIAN_POINT('Origin',(30.,8.5,142.5));
#40074=CARTESIAN_POINT('',(30.9949874371066,8.5,144.));
#40075=CARTESIAN_POINT('Ctrl Pts',(30.9949874371066,8.5,144.));
#40076=CARTESIAN_POINT('Ctrl Pts',(31.0325673132895,8.5,143.975072330207));
#40077=CARTESIAN_POINT('Ctrl Pts',(31.0692099500079,8.5,143.948731762135));
#40078=CARTESIAN_POINT('Ctrl Pts',(31.1048119379707,8.5,143.921052631579));
#40079=CARTESIAN_POINT('',(29.0050125628934,8.5,144.));
#40080=CARTESIAN_POINT('Ctrl Pts',(29.0050125628934,8.5,144.));
#40081=CARTESIAN_POINT('Ctrl Pts',(29.0135741934101,8.5,144.005679143204));
#40082=CARTESIAN_POINT('Ctrl Pts',(29.0221619009622,8.499887926188,144.011270571938));
#40083=CARTESIAN_POINT('Ctrl Pts',(29.0307751172111,8.49967126826958,144.016774482844));
#40084=CARTESIAN_POINT('Ctrl Pts',(29.0424873151203,8.49937665817902,144.024258666676));
#40085=CARTESIAN_POINT('Ctrl Pts',(29.0542337840516,8.49890119138507,144.031576228849));
#40086=CARTESIAN_POINT('Ctrl Pts',(29.0660423164974,8.49823339234552,144.038741725773));
#40087=CARTESIAN_POINT('Ctrl Pts',(29.2076955264615,8.4902225850757,144.12469784648));
#40088=CARTESIAN_POINT('Ctrl Pts',(29.3542371018997,8.45928538094257,144.187286288274));
#40089=CARTESIAN_POINT('Ctrl Pts',(29.5016183779968,8.4294021201831,144.229723268464));
#40090=CARTESIAN_POINT('Ctrl Pts',(29.5753090160454,8.41446048980336,144.250941758559));
#40091=CARTESIAN_POINT('Ctrl Pts',(29.6492095792586,8.39978234526704,144.267122383253));
#40092=CARTESIAN_POINT('Ctrl Pts',(29.7226256562424,8.38828793821598,144.278582306918));
#40093=CARTESIAN_POINT('Ctrl Pts',(29.7960417332263,8.37679353116492,144.290042230583));
#40094=CARTESIAN_POINT('Ctrl Pts',(29.8689733239806,8.36848286159913,144.296781453219));
#40095=CARTESIAN_POINT('Ctrl Pts',(29.94195145693,8.36568839991374,144.299136383465));
#40096=CARTESIAN_POINT('Ctrl Pts',(29.9529560660921,8.3652670139804,144.299491491028));
#40097=CARTESIAN_POINT('Ctrl Pts',(29.9639511678485,8.36496071281008,144.29974204166));
#40098=CARTESIAN_POINT('Ctrl Pts',(29.9749502142532,8.36477781319046,144.2998941289));
#40099=CARTESIAN_POINT('Ctrl Pts',(29.9964912242973,8.36441961463412,144.300191983155));
#40100=CARTESIAN_POINT('Ctrl Pts',(30.0180354039898,8.36453081890395,144.30009870167));
#40101=CARTESIAN_POINT('Ctrl Pts',(30.0395683094927,8.36510330880466,144.299626292527));
#40102=CARTESIAN_POINT('Ctrl Pts',(30.0639695071918,8.36575205726298,144.299090956091));
#40103=CARTESIAN_POINT('Ctrl Pts',(30.0884019395258,8.36701354869722,144.298029111375));
#40104=CARTESIAN_POINT('Ctrl Pts',(30.1127651425163,8.36879615201152,144.296524636117));
#40105=CARTESIAN_POINT('Ctrl Pts',(30.3353233320769,8.38508025745082,144.282781234235));
#40106=CARTESIAN_POINT('Ctrl Pts',(30.5671595347865,8.45070605233951,144.225400079081));
#40107=CARTESIAN_POINT('Ctrl Pts',(30.7847332434266,8.4825312867794,144.119970740243));
#40108=CARTESIAN_POINT('Ctrl Pts',(30.8209955281999,8.48783549251939,144.10239918377));
#40109=CARTESIAN_POINT('Ctrl Pts',(30.8568616325825,8.49220079380246,144.083492955528));
#40110=CARTESIAN_POINT('Ctrl Pts',(30.8918449793237,8.49524192067261,144.063541126495));
#40111=CARTESIAN_POINT('Ctrl Pts',(30.9268283260648,8.49828304754276,144.043589297463));
#40112=CARTESIAN_POINT('Ctrl Pts',(30.9609289151646,8.5,144.022591867639));
#40113=CARTESIAN_POINT('Ctrl Pts',(30.9949874371066,8.5,144.));
#40114=CARTESIAN_POINT('',(28.8951880620293,8.5,143.921052631579));
#40115=CARTESIAN_POINT('Ctrl Pts',(28.8951880620293,8.5,143.921052631579));
#40116=CARTESIAN_POINT('Ctrl Pts',(28.9307900499921,8.5,143.948731762135));
#40117=CARTESIAN_POINT('Ctrl Pts',(28.9674326867105,8.5,143.975072330207));
#40118=CARTESIAN_POINT('Ctrl Pts',(29.0050125628934,8.5,144.));
#40119=CARTESIAN_POINT('Origin',(30.,8.5,142.5));
#40120=CARTESIAN_POINT('Origin',(37.95,8.45,142.2));
#40121=CARTESIAN_POINT('',(37.9,8.4,136.));
#40122=CARTESIAN_POINT('',(37.9,8.4,136.));
#40123=CARTESIAN_POINT('',(37.9,8.4,144.));
#40124=CARTESIAN_POINT('',(38.,8.5,144.));
#40125=CARTESIAN_POINT('',(37.9,8.4,142.2));
#40126=CARTESIAN_POINT('Origin',(37.95,8.,136.));
#40127=CARTESIAN_POINT('',(37.9,8.,135.6));
#40128=CARTESIAN_POINT('Origin',(37.9,8.,136.));
#40129=CARTESIAN_POINT('',(37.9,8.,135.6));
#40130=CARTESIAN_POINT('Origin',(37.95,7.45,135.55));
#40131=CARTESIAN_POINT('',(37.9,5.,135.6));
#40132=CARTESIAN_POINT('',(37.9,5.,135.6));
#40133=CARTESIAN_POINT('',(37.9,7.45,135.6));
#40134=CARTESIAN_POINT('Origin',(37.95,5.,136.));
#40135=CARTESIAN_POINT('Origin',(37.9,5.,136.));
#40136=CARTESIAN_POINT('',(37.9,4.6,136.));
#40137=CARTESIAN_POINT('Origin',(37.95,4.55,137.8));
#40138=CARTESIAN_POINT('',(37.9,4.6,144.));
#40139=CARTESIAN_POINT('Origin',(37.95,5.,144.));
#40140=CARTESIAN_POINT('',(37.9,5.,144.4));
#40141=CARTESIAN_POINT('Origin',(37.9,5.,144.));
#40142=CARTESIAN_POINT('',(37.9,5.,144.4));
#40143=CARTESIAN_POINT('Origin',(37.95,5.55,144.45));
#40144=CARTESIAN_POINT('',(37.9,8.,144.4));
#40145=CARTESIAN_POINT('',(37.9,8.,144.4));
#40146=CARTESIAN_POINT('',(37.9,5.55,144.4));
#40147=CARTESIAN_POINT('Origin',(37.95,8.,144.));
#40148=CARTESIAN_POINT('Origin',(37.9,8.,144.));
#40149=CARTESIAN_POINT('Origin',(-38.,5.,136.));
#40150=CARTESIAN_POINT('',(-37.9,5.,135.6));
#40151=CARTESIAN_POINT('',(-38.,5.,135.6));
#40152=CARTESIAN_POINT('Origin',(-37.9,5.,136.));
#40153=CARTESIAN_POINT('Origin',(-38.,8.4,135.6));
#40154=CARTESIAN_POINT('',(-37.9,8.,135.6));
#40155=CARTESIAN_POINT('',(-38.,8.,135.6));
#40156=CARTESIAN_POINT('',(-37.9,7.45,135.6));
#40157=CARTESIAN_POINT('Origin',(-38.,8.,136.));
#40158=CARTESIAN_POINT('',(31.1661903789691,8.4,136.));
#40159=CARTESIAN_POINT('',(-38.,8.4,136.));
#40160=CARTESIAN_POINT('',(31.0500544632573,8.39129047171135,135.916983334517));
#40161=CARTESIAN_POINT('Ctrl Pts',(31.0500544632573,8.39129047171135,135.916983334517));
#40162=CARTESIAN_POINT('Ctrl Pts',(31.0899798045429,8.39678689624297,135.942890163407));
#40163=CARTESIAN_POINT('Ctrl Pts',(31.1286105027861,8.4,135.970783139968));
#40164=CARTESIAN_POINT('Ctrl Pts',(31.166190378969,8.4,136.));
#40165=CARTESIAN_POINT('',(30.6614250203353,8.29999999989174,135.735424868771));
#40166=CARTESIAN_POINT('Ctrl Pts',(30.6617871419909,8.29994622735324,135.735320177065));
#40167=CARTESIAN_POINT('Ctrl Pts',(30.775165618415,8.33151941969813,135.770967056611));
#40168=CARTESIAN_POINT('Ctrl Pts',(30.8844578418793,8.36220781029194,135.818396041882));
#40169=CARTESIAN_POINT('Ctrl Pts',(30.9900521410047,8.3815773300417,135.880004886115));
#40170=CARTESIAN_POINT('Ctrl Pts',(31.0017011490688,8.3837141470255,135.886801483368));
#40171=CARTESIAN_POINT('Ctrl Pts',(31.0132512017484,8.38570823783425,135.893775706518));
#40172=CARTESIAN_POINT('Ctrl Pts',(31.0247618982842,8.38753579942467,135.900924376673));
#40173=CARTESIAN_POINT('Ctrl Pts',(31.0332269292893,8.38887979850225,135.906181548932));
#40174=CARTESIAN_POINT('Ctrl Pts',(31.0416572725171,8.39013445090616,135.911534549944));
#40175=CARTESIAN_POINT('Ctrl Pts',(31.0500544632573,8.39129047171136,135.916983334517));
#40176=CARTESIAN_POINT('',(29.338574981678,8.29999999933449,135.735424868139));
#40177=CARTESIAN_POINT('Ctrl Pts',(29.3386278125038,8.30008257895501,135.735540389865));
#40178=CARTESIAN_POINT('Ctrl Pts',(29.5057955176886,8.2535712447323,135.683143176038));
#40179=CARTESIAN_POINT('Ctrl Pts',(29.6838689436387,8.20463519701964,135.655313450655));
#40180=CARTESIAN_POINT('Ctrl Pts',(29.8979263724968,8.18554671829636,135.64548462364));
#40181=CARTESIAN_POINT('Ctrl Pts',(29.9260016099788,8.18385989257095,135.644589352545));
#40182=CARTESIAN_POINT('Ctrl Pts',(29.9790456809631,8.18217256996548,135.643730808771));
#40183=CARTESIAN_POINT('Ctrl Pts',(30.0039642863029,8.18202261194883,135.643653901212));
#40184=CARTESIAN_POINT('Ctrl Pts',(30.0415622629051,8.18276540718812,135.644034960973));
#40185=CARTESIAN_POINT('Ctrl Pts',(30.0542548744622,8.18318172952025,135.644248321544));
#40186=CARTESIAN_POINT('Ctrl Pts',(30.0932530393102,8.1849725865134,135.645173639629));
#40187=CARTESIAN_POINT('Ctrl Pts',(30.1194351443769,8.1868501959716,135.646150752494));
#40188=CARTESIAN_POINT('Ctrl Pts',(30.3267044343054,8.20740656544723,135.657166656925));
#40189=CARTESIAN_POINT('Ctrl Pts',(30.4983000996812,8.25464044598778,135.68404798762));
#40190=CARTESIAN_POINT('Ctrl Pts',(30.6614428655482,8.3000552919959,135.735319109435));
#40191=CARTESIAN_POINT('',(28.9499455367427,8.39129047171135,135.916983334517));
#40192=CARTESIAN_POINT('Ctrl Pts',(28.9499455367427,8.39129047171135,135.916983334517));
#40193=CARTESIAN_POINT('Ctrl Pts',(28.9833499104208,8.38669177291416,135.895307843082));
#40194=CARTESIAN_POINT('Ctrl Pts',(29.0505321085055,8.3745011316311,135.855362112556));
#40195=CARTESIAN_POINT('Ctrl Pts',(29.1793447791299,8.34434708123645,135.791526380412));
#40196=CARTESIAN_POINT('Ctrl Pts',(29.2768237032497,8.31707963998262,135.754802014391));
#40197=CARTESIAN_POINT('Ctrl Pts',(29.3385595046862,8.29989676950243,135.735454721815));
#40198=CARTESIAN_POINT('',(28.8338096210309,8.4,136.));
#40199=CARTESIAN_POINT('Ctrl Pts',(28.8338096210309,8.4,136.));
#40200=CARTESIAN_POINT('Ctrl Pts',(28.8713894972124,8.39999999999963,135.970783139966));
#40201=CARTESIAN_POINT('Ctrl Pts',(28.9100201954571,8.39678689624297,135.942890163407));
#40202=CARTESIAN_POINT('Ctrl Pts',(28.9499455367427,8.39129047171135,135.916983334517));
#40203=CARTESIAN_POINT('',(-28.8338096210309,8.4,136.));
#40204=CARTESIAN_POINT('',(-38.,8.4,136.));
#40205=CARTESIAN_POINT('',(-28.9499455367427,8.39129047171135,135.916983334517));
#40206=CARTESIAN_POINT('Ctrl Pts',(-28.9499455367427,8.39129047171135,135.916983334517));
#40207=CARTESIAN_POINT('Ctrl Pts',(-28.9100201954571,8.39678689624297,135.942890163407));
#40208=CARTESIAN_POINT('Ctrl Pts',(-28.8713894972139,8.4,135.970783139968));
#40209=CARTESIAN_POINT('Ctrl Pts',(-28.833809621031,8.4,136.));
#40210=CARTESIAN_POINT('',(-29.3385749796646,8.29999999989175,135.735424868771));
#40211=CARTESIAN_POINT('Ctrl Pts',(-29.3381669864801,8.30010233118074,135.735322327554));
#40212=CARTESIAN_POINT('Ctrl Pts',(-29.2247952376504,8.33157740613302,135.770950841463));
#40213=CARTESIAN_POINT('Ctrl Pts',(-29.1155062056164,8.36211580901458,135.818341931665));
#40214=CARTESIAN_POINT('Ctrl Pts',(-29.0099454651912,8.3815739822389,135.880001956662));
#40215=CARTESIAN_POINT('Ctrl Pts',(-28.9983001592736,8.38372057934386,135.886804200101));
#40216=CARTESIAN_POINT('Ctrl Pts',(-28.9867478988158,8.3857073377265,135.893774692507));
#40217=CARTESIAN_POINT('Ctrl Pts',(-28.9752376631878,8.38753570208383,135.900923965067));
#40218=CARTESIAN_POINT('Ctrl Pts',(-28.9667729711371,8.38888029152071,135.906181580337));
#40219=CARTESIAN_POINT('Ctrl Pts',(-28.9583427274828,8.39013445090617,135.911534549944));
#40220=CARTESIAN_POINT('Ctrl Pts',(-28.9499455367427,8.39129047171136,135.916983334517));
#40221=CARTESIAN_POINT('',(-30.661425018322,8.29999999933447,135.735424868139));
#40222=CARTESIAN_POINT('Ctrl Pts',(-30.6614403324357,8.29990288566549,135.735450246584));
#40223=CARTESIAN_POINT('Ctrl Pts',(-30.5288224131844,8.26307573905403,135.693849975409));
#40224=CARTESIAN_POINT('Ctrl Pts',(-30.3889944469613,8.22475878909875,135.667443669542));
#40225=CARTESIAN_POINT('Ctrl Pts',(-30.2068474352435,8.19595429131145,135.651012005824));
#40226=CARTESIAN_POINT('Ctrl Pts',(-30.1685015966763,8.19115568892363,135.648342005986));
#40227=CARTESIAN_POINT('Ctrl Pts',(-30.0772899664358,8.18310206076612,135.644103777041));
#40228=CARTESIAN_POINT('Ctrl Pts',(-30.0241258793722,8.18117464424746,135.643151906577));
#40229=CARTESIAN_POINT('Ctrl Pts',(-29.9583002059055,8.18248038026162,135.643821210287));
#40230=CARTESIAN_POINT('Ctrl Pts',(-29.945607880728,8.18289720095053,135.6440346745));
#40231=CARTESIAN_POINT('Ctrl Pts',(-29.9066026001864,8.18468277370489,135.644958149235));
#40232=CARTESIAN_POINT('Ctrl Pts',(-29.8804218187696,8.1865934232616,135.645948287097));
#40233=CARTESIAN_POINT('Ctrl Pts',(-29.7775051143642,8.19662294325174,135.651344091606));
#40234=CARTESIAN_POINT('Ctrl Pts',(-29.6004619510134,8.2275301924826,135.668504490137));
#40235=CARTESIAN_POINT('Ctrl Pts',(-29.4324777206386,8.27391945427491,135.705706123537));
#40236=CARTESIAN_POINT('Ctrl Pts',(-29.3385146936142,8.30000579886974,135.735213097063));
#40237=CARTESIAN_POINT('',(-31.0500544632573,8.39129047171135,135.916983334517));
#40238=CARTESIAN_POINT('Ctrl Pts',(-31.0500544632574,8.39129047171136,135.916983334517));
#40239=CARTESIAN_POINT('Ctrl Pts',(-30.9908315655339,8.38313739956722,135.87855467171));
#40240=CARTESIAN_POINT('Ctrl Pts',(-30.8660346152952,8.35700091284835,135.809286827101));
#40241=CARTESIAN_POINT('Ctrl Pts',(-30.7318879198758,8.31946572940279,135.757548608235));
#40242=CARTESIAN_POINT('Ctrl Pts',(-30.6614403324357,8.29990288566549,135.735450246584));
#40243=CARTESIAN_POINT('',(-31.0754160204889,8.39448466110766,135.933804440098));
#40244=CARTESIAN_POINT('Ctrl Pts',(-31.0754096448176,8.39448483093512,135.933813086818));
#40245=CARTESIAN_POINT('Ctrl Pts',(-31.0670151585375,8.39352977637734,135.92811721501));
#40246=CARTESIAN_POINT('Ctrl Pts',(-31.0585642183151,8.39246198897211,135.922505160031));
#40247=CARTESIAN_POINT('Ctrl Pts',(-31.0500544632573,8.39129047171135,135.916983334517));
#40248=CARTESIAN_POINT('',(-31.1661903789691,8.4,136.));
#40249=CARTESIAN_POINT('Ctrl Pts',(-31.1661903789691,8.4,136.));
#40250=CARTESIAN_POINT('Ctrl Pts',(-31.1366203414292,8.3999999999997,135.97701047114));
#40251=CARTESIAN_POINT('Ctrl Pts',(-31.1063996916262,8.39801061970443,135.954840619422));
#40252=CARTESIAN_POINT('Ctrl Pts',(-31.0754096448176,8.39448483093512,135.933813086818));
#40253=CARTESIAN_POINT('',(-37.9,8.4,136.));
#40254=CARTESIAN_POINT('',(-38.,8.4,136.));
#40255=CARTESIAN_POINT('Origin',(-37.9,8.,136.));
#40256=CARTESIAN_POINT('Origin',(-38.,8.4,144.4));
#40257=CARTESIAN_POINT('',(31.1661903789691,8.4,144.));
#40258=CARTESIAN_POINT('',(-38.,8.4,144.));
#40259=CARTESIAN_POINT('',(28.8338096210309,8.4,144.));
#40260=CARTESIAN_POINT('Origin',(30.,8.4,142.5));
#40261=CARTESIAN_POINT('',(-28.8338096210309,8.4,144.));
#40262=CARTESIAN_POINT('',(-38.,8.4,144.));
#40263=CARTESIAN_POINT('',(-31.1661903789691,8.4,144.));
#40264=CARTESIAN_POINT('Origin',(-30.,8.4,142.5));
#40265=CARTESIAN_POINT('',(-37.9,8.4,144.));
#40266=CARTESIAN_POINT('',(-38.,8.4,144.));
#40267=CARTESIAN_POINT('',(-37.9,8.4,142.2));
#40268=CARTESIAN_POINT('Origin',(-30.,8.4,137.5));
#40269=CARTESIAN_POINT('Origin',(30.,8.4,137.5));
#40270=CARTESIAN_POINT('Origin',(-37.95,8.45,142.2));
#40271=CARTESIAN_POINT('',(-38.,8.5,136.));
#40272=CARTESIAN_POINT('',(-37.9,8.4,144.));
#40273=CARTESIAN_POINT('Origin',(-37.95,8.,136.));
#40274=CARTESIAN_POINT('',(-38.,8.,135.5));
#40275=CARTESIAN_POINT('Origin',(-37.95,7.45,135.55));
#40276=CARTESIAN_POINT('',(-38.,5.,135.5));
#40277=CARTESIAN_POINT('Origin',(-37.95,5.,136.));
#40278=CARTESIAN_POINT('',(-38.,4.50000000000002,136.));
#40279=CARTESIAN_POINT('Origin',(-37.95,4.55,137.8));
#40280=CARTESIAN_POINT('',(-38.,4.5,144.));
#40281=CARTESIAN_POINT('Origin',(-37.95,5.,144.));
#40282=CARTESIAN_POINT('',(-37.9,5.,144.4));
#40283=CARTESIAN_POINT('',(-38.,5.,144.5));
#40284=CARTESIAN_POINT('Origin',(-37.9,5.,144.));
#40285=CARTESIAN_POINT('Origin',(-37.95,5.55,144.45));
#40286=CARTESIAN_POINT('',(-37.9,8.,144.4));
#40287=CARTESIAN_POINT('',(-38.,8.,144.5));
#40288=CARTESIAN_POINT('',(-37.9,5.55,144.4));
#40289=CARTESIAN_POINT('Origin',(-37.95,8.,144.));
#40290=CARTESIAN_POINT('Origin',(-37.9,8.,144.));
#40291=CARTESIAN_POINT('Origin',(-38.,5.,144.));
#40292=CARTESIAN_POINT('',(-38.,5.,144.4));
#40293=CARTESIAN_POINT('Origin',(-38.,4.6,144.4));
#40294=CARTESIAN_POINT('',(-38.,8.,144.4));
#40295=CARTESIAN_POINT('Origin',(-38.,8.,144.));
#40296=CARTESIAN_POINT('',(-31.0500544632573,8.39129047171135,144.083016665483));
#40297=CARTESIAN_POINT('Ctrl Pts',(-31.0500544632573,8.39129047171135,144.083016665483));
#40298=CARTESIAN_POINT('Ctrl Pts',(-31.0899798045429,8.39678689624297,144.057109836593));
#40299=CARTESIAN_POINT('Ctrl Pts',(-31.1286105027861,8.4,144.029216860032));
#40300=CARTESIAN_POINT('Ctrl Pts',(-31.166190378969,8.4,144.));
#40301=CARTESIAN_POINT('',(-30.6614250203354,8.29999999989176,144.264575131229));
#40302=CARTESIAN_POINT('Ctrl Pts',(-30.6618396899871,8.29991781521182,144.264739808957));
#40303=CARTESIAN_POINT('Ctrl Pts',(-30.7751945183757,8.33150592132261,144.229066212155));
#40304=CARTESIAN_POINT('Ctrl Pts',(-30.8844650149679,8.36221060079717,144.181611705071));
#40305=CARTESIAN_POINT('Ctrl Pts',(-30.9900531081148,8.38157715543247,144.119996210819));
#40306=CARTESIAN_POINT('Ctrl Pts',(-31.0017014315445,8.38371364530919,144.113198879946));
#40307=CARTESIAN_POINT('Ctrl Pts',(-31.0132516281393,8.38570812580638,144.106224780502));
#40308=CARTESIAN_POINT('Ctrl Pts',(-31.0247621663533,8.38753570049785,144.099075932216));
#40309=CARTESIAN_POINT('Ctrl Pts',(-31.0332270809276,8.38887970921002,144.093818628959));
#40310=CARTESIAN_POINT('Ctrl Pts',(-31.0416572725171,8.39013445090614,144.088465450056));
#40311=CARTESIAN_POINT('Ctrl Pts',(-31.0500544632573,8.39129047171135,144.083016665483));
#40312=CARTESIAN_POINT('',(-29.338574981678,8.29999999933447,144.264575131861));
#40313=CARTESIAN_POINT('Ctrl Pts',(-29.338652459278,8.30015458067006,144.264432850785));
#40314=CARTESIAN_POINT('Ctrl Pts',(-29.471254955589,8.26335414343341,144.306032812001));
#40315=CARTESIAN_POINT('Ctrl Pts',(-29.6110602576202,8.22506281541357,144.332438307369));
#40316=CARTESIAN_POINT('Ctrl Pts',(-29.7931828978245,8.19627966997637,144.348871433016));
#40317=CARTESIAN_POINT('Ctrl Pts',(-29.8315050694548,8.19147962387844,144.351541055828));
#40318=CARTESIAN_POINT('Ctrl Pts',(-29.8980881273779,8.18561185509721,144.354637251728));
#40319=CARTESIAN_POINT('Ctrl Pts',(-29.9261331455688,8.18390663041651,144.355518923594));
#40320=CARTESIAN_POINT('Ctrl Pts',(-29.9791768427067,8.18222339100664,144.356378794531));
#40321=CARTESIAN_POINT('Ctrl Pts',(-30.0040925088588,8.18207177302637,144.356454836261));
#40322=CARTESIAN_POINT('Ctrl Pts',(-30.0416869686119,8.18281540243689,144.356073075862));
#40323=CARTESIAN_POINT('Ctrl Pts',(-30.0543793900807,8.18323091163571,144.355860174902));
#40324=CARTESIAN_POINT('Ctrl Pts',(-30.0933740369497,8.18502349243028,144.354933142189));
#40325=CARTESIAN_POINT('Ctrl Pts',(-30.1195554386871,8.18690252431569,144.353956583673));
#40326=CARTESIAN_POINT('Ctrl Pts',(-30.326804087216,8.2074032973194,144.342951164697));
#40327=CARTESIAN_POINT('Ctrl Pts',(-30.4983498772685,8.25464807568585,144.316029140081));
#40328=CARTESIAN_POINT('Ctrl Pts',(-30.661449901242,8.30007700746228,144.264722411094));
#40329=CARTESIAN_POINT('',(-28.9499455367427,8.39129047171135,144.083016665483));
#40330=CARTESIAN_POINT('Ctrl Pts',(-28.9499455367427,8.39129047171135,144.083016665483));
#40331=CARTESIAN_POINT('Ctrl Pts',(-29.009168434466,8.38313739956723,144.121445328289));
#40332=CARTESIAN_POINT('Ctrl Pts',(-29.1339710420765,8.35700176313992,144.190714621136));
#40333=CARTESIAN_POINT('Ctrl Pts',(-29.2681148397227,8.3194718198051,144.242448628163));
#40334=CARTESIAN_POINT('Ctrl Pts',(-29.3385631777598,8.29991175184865,144.264544801319));
#40335=CARTESIAN_POINT('Ctrl Pts',(-28.8338096210309,8.4,144.));
#40336=CARTESIAN_POINT('Ctrl Pts',(-28.8713894972124,8.39999999999963,144.029216860034));
#40337=CARTESIAN_POINT('Ctrl Pts',(-28.9100201954571,8.39678689624297,144.057109836593));
#40338=CARTESIAN_POINT('Ctrl Pts',(-28.9499455367427,8.39129047171135,144.083016665483));
#40339=CARTESIAN_POINT('',(28.9499455367427,8.39129047171135,144.083016665483));
#40340=CARTESIAN_POINT('Ctrl Pts',(28.9499455367427,8.39129047171135,144.083016665483));
#40341=CARTESIAN_POINT('Ctrl Pts',(28.9100201954571,8.39678689624297,144.057109836593));
#40342=CARTESIAN_POINT('Ctrl Pts',(28.8713894972139,8.4,144.029216860032));
#40343=CARTESIAN_POINT('Ctrl Pts',(28.833809621031,8.4,144.));
#40344=CARTESIAN_POINT('',(29.3385749796647,8.29999999989175,144.264575131229));
#40345=CARTESIAN_POINT('Ctrl Pts',(29.3382753761609,8.30022001211062,144.264570458976));
#40346=CARTESIAN_POINT('Ctrl Pts',(29.2248705789997,8.33165596203575,144.228985346631));
#40347=CARTESIAN_POINT('Ctrl Pts',(29.115491058347,8.36206433955672,144.181672395662));
#40348=CARTESIAN_POINT('Ctrl Pts',(29.0099464509446,8.38157135670728,144.119998131135));
#40349=CARTESIAN_POINT('Ctrl Pts',(28.9983029247983,8.38372334220249,144.113194316812));
#40350=CARTESIAN_POINT('Ctrl Pts',(28.9867485261411,8.38570645439427,144.106225228903));
#40351=CARTESIAN_POINT('Ctrl Pts',(28.9752382142316,8.38753536993229,144.099075890131));
#40352=CARTESIAN_POINT('Ctrl Pts',(28.9667734660829,8.38888036471055,144.093818226167));
#40353=CARTESIAN_POINT('Ctrl Pts',(28.9583427274828,8.39013445090616,144.088465450056));
#40354=CARTESIAN_POINT('Ctrl Pts',(28.9499455367427,8.39129047171136,144.083016665483));
#40355=CARTESIAN_POINT('',(30.661425018322,8.29999999933449,144.264575131861));
#40356=CARTESIAN_POINT('Ctrl Pts',(30.6614433761257,8.29987533145044,144.264537899321));
#40357=CARTESIAN_POINT('Ctrl Pts',(30.4943037331861,8.25333014297023,144.316908600203));
#40358=CARTESIAN_POINT('Ctrl Pts',(30.3162632139204,8.20435742950814,144.344707484172));
#40359=CARTESIAN_POINT('Ctrl Pts',(30.1021065839386,8.18529590996961,144.354567989873));
#40360=CARTESIAN_POINT('Ctrl Pts',(30.074028637424,8.18360776495036,144.355462743862));
#40361=CARTESIAN_POINT('Ctrl Pts',(30.0209792504149,8.18191724490555,144.356319890362));
#40362=CARTESIAN_POINT('Ctrl Pts',(29.9960550388621,8.18176901342238,144.356398301945));
#40363=CARTESIAN_POINT('Ctrl Pts',(29.9584499596871,8.18250975841238,144.356016804967));
#40364=CARTESIAN_POINT('Ctrl Pts',(29.9457591107073,8.18293041085672,144.355804314577));
#40365=CARTESIAN_POINT('Ctrl Pts',(29.8489171025918,8.18733644430337,144.353503744874));
#40366=CARTESIAN_POINT('Ctrl Pts',(29.6834564814262,8.20996035010193,144.34210623907));
#40367=CARTESIAN_POINT('Ctrl Pts',(29.4880447175627,8.25873483980795,144.307413737166));
#40368=CARTESIAN_POINT('Ctrl Pts',(29.3751540243146,8.28999725964461,144.276134934077));
#40369=CARTESIAN_POINT('Ctrl Pts',(29.3385834550246,8.30013461249329,144.264667098602));
#40370=CARTESIAN_POINT('',(31.0500544632573,8.39129047171135,144.083016665483));
#40371=CARTESIAN_POINT('Ctrl Pts',(31.0500544632573,8.39129047171135,144.083016665483));
#40372=CARTESIAN_POINT('Ctrl Pts',(31.0166500895791,8.38669177291414,144.104692156918));
#40373=CARTESIAN_POINT('Ctrl Pts',(30.9494752442691,8.37449659083024,144.144633707188));
#40374=CARTESIAN_POINT('Ctrl Pts',(30.8206483458436,8.34434509414795,144.208476224786));
#40375=CARTESIAN_POINT('Ctrl Pts',(30.7231761413096,8.31706672387149,144.245194863023));
#40376=CARTESIAN_POINT('Ctrl Pts',(30.6614433761257,8.29987533145044,144.264537899321));
#40377=CARTESIAN_POINT('',(31.0754160204992,8.39448466110884,144.066195559895));
#40378=CARTESIAN_POINT('Ctrl Pts',(31.0754096448279,8.3944848309363,144.066186913175));
#40379=CARTESIAN_POINT('Ctrl Pts',(31.0670151585444,8.39352977637821,144.071882784985));
#40380=CARTESIAN_POINT('Ctrl Pts',(31.0585642183186,8.39246198897259,144.077494839966));
#40381=CARTESIAN_POINT('Ctrl Pts',(31.0500544632573,8.39129047171135,144.083016665483));
#40382=CARTESIAN_POINT('Ctrl Pts',(31.1661903789691,8.4,144.));
#40383=CARTESIAN_POINT('Ctrl Pts',(31.1366203414324,8.39999999999971,144.022989528857));
#40384=CARTESIAN_POINT('Ctrl Pts',(31.1063996916329,8.39801061970488,144.045159380573));
#40385=CARTESIAN_POINT('Ctrl Pts',(31.0754096448279,8.3944848309363,144.066186913175));
#40386=CARTESIAN_POINT('Ctrl Pts',(28.9499455367427,8.39129047171135,144.083016665483));
#40387=CARTESIAN_POINT('Ctrl Pts',(28.9583427274828,8.39013445090615,144.088465450056));
#40388=CARTESIAN_POINT('Ctrl Pts',(28.9667734660829,8.38888036471054,144.093818226167));
#40389=CARTESIAN_POINT('Ctrl Pts',(28.9867485261411,8.38570645439426,144.106225228903));
#40390=CARTESIAN_POINT('Ctrl Pts',(28.9983029247983,8.38372334220247,144.113194316812));
#40391=CARTESIAN_POINT('Ctrl Pts',(29.1496202725203,8.35575649321004,144.201615566941));
#40392=CARTESIAN_POINT('Ctrl Pts',(29.3692050696252,8.28839704166518,144.286315495019));
#40393=CARTESIAN_POINT('Ctrl Pts',(29.6834564814262,8.20996035010193,144.34210623907));
#40394=CARTESIAN_POINT('Ctrl Pts',(29.8489171025918,8.18733644430337,144.353503744874));
#40395=CARTESIAN_POINT('Ctrl Pts',(29.9457591107073,8.18293041085672,144.355804314577));
#40396=CARTESIAN_POINT('Ctrl Pts',(29.9584499596871,8.18250975841238,144.356016804967));
#40397=CARTESIAN_POINT('Ctrl Pts',(29.9960550388621,8.18176901342238,144.356398301945));
#40398=CARTESIAN_POINT('Ctrl Pts',(30.0209792504149,8.18191724490555,144.356319890362));
#40399=CARTESIAN_POINT('Ctrl Pts',(30.074028637424,8.18360776495036,144.355462743862));
#40400=CARTESIAN_POINT('Ctrl Pts',(30.1021065839386,8.18529590996961,144.354567989873));
#40401=CARTESIAN_POINT('Ctrl Pts',(30.3850503615939,8.21047999297718,144.341540287986));
#40402=CARTESIAN_POINT('Ctrl Pts',(30.6646454100207,8.30783313849756,144.285786323045));
#40403=CARTESIAN_POINT('Ctrl Pts',(30.9494752442691,8.37449659083024,144.144633707188));
#40404=CARTESIAN_POINT('Ctrl Pts',(31.0166500895791,8.38669177291414,144.104692156918));
#40405=CARTESIAN_POINT('Ctrl Pts',(31.0500544632573,8.39129047171135,144.083016665483));
#40406=CARTESIAN_POINT('Ctrl Pts',(28.9683012121262,8.4275269811409,144.055344443655));
#40407=CARTESIAN_POINT('Ctrl Pts',(28.9767513031944,8.42675710035562,144.060870100283));
#40408=CARTESIAN_POINT('Ctrl Pts',(28.9852390011866,8.42588181711275,144.06630220525));
#40409=CARTESIAN_POINT('Ctrl Pts',(29.0053237629384,8.4235986014281,144.078903194632));
#40410=CARTESIAN_POINT('Ctrl Pts',(29.0169525178044,8.42211351066722,144.085988008261));
#40411=CARTESIAN_POINT('Ctrl Pts',(29.1689435287771,8.40060024527846,144.175976886636));
#40412=CARTESIAN_POINT('Ctrl Pts',(29.3886619077997,8.34023129010989,144.263730862112));
#40413=CARTESIAN_POINT('Ctrl Pts',(29.696681571984,8.2683613847734,144.32250041751));
#40414=CARTESIAN_POINT('Ctrl Pts',(29.8556533021349,8.24775166628686,144.334588797671));
#40415=CARTESIAN_POINT('Ctrl Pts',(29.9481782437644,8.24373599383981,144.337025491425));
#40416=CARTESIAN_POINT('Ctrl Pts',(29.96031140905,8.24335735060291,144.337249855718));
#40417=CARTESIAN_POINT('Ctrl Pts',(29.9962175677341,8.24267481277293,144.337656505504));
#40418=CARTESIAN_POINT('Ctrl Pts',(30.0200334024999,8.24282657196158,144.337568458374));
#40419=CARTESIAN_POINT('Ctrl Pts',(30.0706836000534,8.24433573825835,144.336668567379));
#40420=CARTESIAN_POINT('Ctrl Pts',(30.0975914106849,8.24592098169161,144.335706222849));
#40421=CARTESIAN_POINT('Ctrl Pts',(30.3682304958345,8.26852298441906,144.322002439928));
#40422=CARTESIAN_POINT('Ctrl Pts',(30.6450768082368,8.35906946466354,144.262471796798));
#40423=CARTESIAN_POINT('Ctrl Pts',(30.9305532331129,8.41520829163761,144.117944392387));
#40424=CARTESIAN_POINT('Ctrl Pts',(30.9980737545343,8.42441643284468,144.07732956379));
#40425=CARTESIAN_POINT('Ctrl Pts',(31.0316987878737,8.4275269811409,144.055344443655));
#40426=CARTESIAN_POINT('Ctrl Pts',(28.9866568875098,8.46376349057045,144.027672221828));
#40427=CARTESIAN_POINT('Ctrl Pts',(28.9951656176985,8.46337735055053,144.033274492976));
#40428=CARTESIAN_POINT('Ctrl Pts',(29.0036963658584,8.46288647378579,144.038786592855));
#40429=CARTESIAN_POINT('Ctrl Pts',(29.0239120783231,8.46148451114518,144.051580700947));
#40430=CARTESIAN_POINT('Ctrl Pts',(29.0355841910455,8.46051102292033,144.0587825374));
#40431=CARTESIAN_POINT('Ctrl Pts',(29.1883722702047,8.44537883300728,144.150336526785));
#40432=CARTESIAN_POINT('Ctrl Pts',(29.4080510514443,8.39198253043129,144.241165142077));
#40433=CARTESIAN_POINT('Ctrl Pts',(29.7098850519141,8.32670316605924,144.302908829508));
#40434=CARTESIAN_POINT('Ctrl Pts',(29.8622371244374,8.30806763961565,144.315696400422));
#40435=CARTESIAN_POINT('Ctrl Pts',(29.9505369330349,8.30446143099731,144.31827031418));
#40436=CARTESIAN_POINT('Ctrl Pts',(29.9620897184856,8.30411312061956,144.318508990909));
#40437=CARTESIAN_POINT('Ctrl Pts',(29.9963286954253,8.30351381528359,144.318933779595));
#40438=CARTESIAN_POINT('Ctrl Pts',(30.0189812519047,8.30362149184793,144.318850133658));
#40439=CARTESIAN_POINT('Ctrl Pts',(30.0673145445624,8.30502408395499,144.317885132574));
#40440=CARTESIAN_POINT('Ctrl Pts',(30.0929171127796,8.30638847697522,144.316890878399));
#40441=CARTESIAN_POINT('Ctrl Pts',(30.3521431978363,8.32703726600895,144.302319082293));
#40442=CARTESIAN_POINT('Ctrl Pts',(30.6253675036887,8.41040735865498,144.239151079469));
#40443=CARTESIAN_POINT('Ctrl Pts',(30.9116497481213,8.45585439427816,144.091276042087));
#40444=CARTESIAN_POINT('Ctrl Pts',(30.9795052502094,8.46227534006946,144.049954460767));
#40445=CARTESIAN_POINT('Ctrl Pts',(31.0133431124902,8.46376349057045,144.027672221828));
#40446=CARTESIAN_POINT('Ctrl Pts',(29.0050125628934,8.5,144.));
#40447=CARTESIAN_POINT('Ctrl Pts',(29.01357419341,8.5,144.005679143204));
#40448=CARTESIAN_POINT('Ctrl Pts',(29.0221619009622,8.49988792618801,144.011270571938));
#40449=CARTESIAN_POINT('Ctrl Pts',(29.0424873151203,8.49937665817902,144.024258666676));
#40450=CARTESIAN_POINT('Ctrl Pts',(29.0542337840516,8.49890119138508,144.031576228849));
#40451=CARTESIAN_POINT('Ctrl Pts',(29.2076955264615,8.4902225850757,144.12469784648));
#40452=CARTESIAN_POINT('Ctrl Pts',(29.4275078896188,8.44381677887601,144.218580509171));
#40453=CARTESIAN_POINT('Ctrl Pts',(29.7231101424719,8.38510420073072,144.283303007947));
#40454=CARTESIAN_POINT('Ctrl Pts',(29.8689733239806,8.36848286159914,144.296781453219));
#40455=CARTESIAN_POINT('Ctrl Pts',(29.9529560660921,8.36526701398041,144.299491491028));
#40456=CARTESIAN_POINT('Ctrl Pts',(29.9639511678485,8.36496071281008,144.29974204166));
#40457=CARTESIAN_POINT('Ctrl Pts',(29.9964912242973,8.36441961463413,144.300191983155));
#40458=CARTESIAN_POINT('Ctrl Pts',(30.0180354039898,8.36453081890395,144.30009870167));
#40459=CARTESIAN_POINT('Ctrl Pts',(30.0639695071918,8.36575205726298,144.299090956091));
#40460=CARTESIAN_POINT('Ctrl Pts',(30.0884019395258,8.36701354869723,144.298029111375));
#40461=CARTESIAN_POINT('Ctrl Pts',(30.3353233320769,8.38508025745083,144.282781234235));
#40462=CARTESIAN_POINT('Ctrl Pts',(30.6057989019047,8.46164368482096,144.215836553222));
#40463=CARTESIAN_POINT('Ctrl Pts',(30.892727736965,8.49656609508553,144.064586727286));
#40464=CARTESIAN_POINT('Ctrl Pts',(30.9609289151646,8.5,144.022591867639));
#40465=CARTESIAN_POINT('Ctrl Pts',(30.9949874371066,8.5,144.));
#40466=CARTESIAN_POINT('',(28.9499455367427,8.39129047171135,144.083016665483));
#40467=CARTESIAN_POINT('',(30.9949874371066,8.5,144.));
#40468=CARTESIAN_POINT('Origin',(30.,8.45,142.5));
#40469=CARTESIAN_POINT('',(31.1661903789691,8.4,144.));
#40470=CARTESIAN_POINT('',(28.8951880620293,8.5,143.921052631579));
#40471=CARTESIAN_POINT('Ctrl Pts',(31.0500544632573,8.39129047171135,144.083016665483));
#40472=CARTESIAN_POINT('Ctrl Pts',(31.0899798051577,8.39678689632762,144.057109836194));
#40473=CARTESIAN_POINT('Ctrl Pts',(31.1286105039774,8.40000000009859,144.029216859175));
#40474=CARTESIAN_POINT('Ctrl Pts',(31.1661903807052,8.4,143.99999999865));
#40475=CARTESIAN_POINT('Ctrl Pts',(31.0316987878737,8.4275269811409,144.055344443655));
#40476=CARTESIAN_POINT('Ctrl Pts',(31.0708423080612,8.43119126421841,144.029764000737));
#40477=CARTESIAN_POINT('Ctrl Pts',(31.1088103196971,8.43333333339906,144.002388493225));
#40478=CARTESIAN_POINT('Ctrl Pts',(31.145730900342,8.43333333333333,143.9736842092));
#40479=CARTESIAN_POINT('Ctrl Pts',(31.0133431124902,8.46376349057045,144.027672221828));
#40480=CARTESIAN_POINT('Ctrl Pts',(31.0517048109648,8.46559563210921,144.00241816528));
#40481=CARTESIAN_POINT('Ctrl Pts',(31.0890101354168,8.46666666669953,143.975560127274));
#40482=CARTESIAN_POINT('Ctrl Pts',(31.1252714199787,8.46666666666667,143.94736841975));
#40483=CARTESIAN_POINT('Ctrl Pts',(30.9949874371066,8.5,144.));
#40484=CARTESIAN_POINT('Ctrl Pts',(31.0325673138683,8.5,143.975072329823));
#40485=CARTESIAN_POINT('Ctrl Pts',(31.0692099511365,8.5,143.948731761324));
#40486=CARTESIAN_POINT('Ctrl Pts',(31.1048119396155,8.5,143.9210526303));
#40487=CARTESIAN_POINT('Ctrl Pts',(28.833809621031,8.4,144.));
#40488=CARTESIAN_POINT('Ctrl Pts',(28.8713894972139,8.4,144.029216860032));
#40489=CARTESIAN_POINT('Ctrl Pts',(28.9100201954571,8.39678689624297,144.057109836593));
#40490=CARTESIAN_POINT('Ctrl Pts',(28.9499455367427,8.39129047171135,144.083016665483));
#40491=CARTESIAN_POINT('Ctrl Pts',(28.8542691013637,8.43333333333333,143.973684210526));
#40492=CARTESIAN_POINT('Ctrl Pts',(28.8911896814733,8.43333333333333,144.002388494066));
#40493=CARTESIAN_POINT('Ctrl Pts',(28.9291576925416,8.43119126416198,144.029764001131));
#40494=CARTESIAN_POINT('Ctrl Pts',(28.9683012121263,8.4275269811409,144.055344443655));
#40495=CARTESIAN_POINT('Ctrl Pts',(28.8747285816965,8.46666666666667,143.947368421053));
#40496=CARTESIAN_POINT('Ctrl Pts',(28.9109898657327,8.46666666666667,143.975560128101));
#40497=CARTESIAN_POINT('Ctrl Pts',(28.948295189626,8.46559563208099,144.002418165669));
#40498=CARTESIAN_POINT('Ctrl Pts',(28.9866568875098,8.46376349057045,144.027672221828));
#40499=CARTESIAN_POINT('Ctrl Pts',(28.8951880620293,8.5,143.921052631579));
#40500=CARTESIAN_POINT('Ctrl Pts',(28.9307900499921,8.5,143.948731762135));
#40501=CARTESIAN_POINT('Ctrl Pts',(28.9674326867105,8.5,143.975072330207));
#40502=CARTESIAN_POINT('Ctrl Pts',(29.0050125628934,8.5,144.));
#40503=CARTESIAN_POINT('Origin',(-30.,8.95,137.5));
#40504=CARTESIAN_POINT('',(-29.19613123823,8.9,135.889473684211));
#40505=CARTESIAN_POINT('',(-29.1514718625761,9.,135.8));
#40506=CARTESIAN_POINT('',(-31.8,8.9,137.5));
#40507=CARTESIAN_POINT('Origin',(-30.,8.9,137.5));
#40508=CARTESIAN_POINT('',(-30.80386876177,8.9,135.889473684211));
#40509=CARTESIAN_POINT('Origin',(-30.,8.9,137.5));
#40510=CARTESIAN_POINT('',(-30.80386876177,8.9,135.889473684211));
#40511=CARTESIAN_POINT('Ctrl Pts',(-30.62442393624,8.99442305443429,135.70570254201));
#40512=CARTESIAN_POINT('Ctrl Pts',(-30.6031336007837,8.99354972599348,135.698345055793));
#40513=CARTESIAN_POINT('Ctrl Pts',(-30.5816752394099,8.99263100796461,135.691382689721));
#40514=CARTESIAN_POINT('Ctrl Pts',(-30.4123094665995,8.98495128128084,135.639444028187));
#40515=CARTESIAN_POINT('Ctrl Pts',(-30.1802232821902,8.97487183787893,135.600774173325));
#40516=CARTESIAN_POINT('Ctrl Pts',(-29.8198774693527,8.97481364719588,135.600649477793));
#40517=CARTESIAN_POINT('Ctrl Pts',(-29.5876626138109,8.9849459908676,135.639432675438));
#40518=CARTESIAN_POINT('Ctrl Pts',(-29.418327451187,8.9926309002887,135.691382459919));
#40519=CARTESIAN_POINT('Ctrl Pts',(-29.3968663992163,8.99354972599348,135.698345055793));
#40520=CARTESIAN_POINT('Ctrl Pts',(-29.37557606376,8.99442305443429,135.70570254201));
#40521=CARTESIAN_POINT('Ctrl Pts',(-30.6134852835967,8.96294870295619,135.737135028007));
#40522=CARTESIAN_POINT('Ctrl Pts',(-30.5926585146851,8.96237089086999,135.729918298573));
#40523=CARTESIAN_POINT('Ctrl Pts',(-30.5716540370928,8.96172231480688,135.723090172466));
#40524=CARTESIAN_POINT('Ctrl Pts',(-30.4057627068958,8.95618694003155,135.671989821309));
#40525=CARTESIAN_POINT('Ctrl Pts',(-30.1774809150283,8.94781763959255,135.633524301555));
#40526=CARTESIAN_POINT('Ctrl Pts',(-29.8226191720034,8.94775803303614,135.63340083736));
#40527=CARTESIAN_POINT('Ctrl Pts',(-29.5942099936947,8.9561825817824,135.671977657888));
#40528=CARTESIAN_POINT('Ctrl Pts',(-29.4283485325563,8.96172203669287,135.723090090889));
#40529=CARTESIAN_POINT('Ctrl Pts',(-29.4073415857357,8.96237102991341,135.729918177652));
#40530=CARTESIAN_POINT('Ctrl Pts',(-29.3865147164033,8.96294870295619,135.737135028007));
#40531=CARTESIAN_POINT('Ctrl Pts',(-30.6025466309533,8.9314743514781,135.768567514003));
#40532=CARTESIAN_POINT('Ctrl Pts',(-30.582184785483,8.93117883512348,135.761502062769));
#40533=CARTESIAN_POINT('Ctrl Pts',(-30.5616314866267,8.93082738428349,135.754786613406));
#40534=CARTESIAN_POINT('Ctrl Pts',(-30.3992200288979,8.92734716856885,135.704598391766));
#40535=CARTESIAN_POINT('Ctrl Pts',(-30.1747360509692,8.92072266060556,135.666303758425));
#40536=CARTESIAN_POINT('Ctrl Pts',(-29.8253607851682,8.92068624425422,135.666171804744));
#40537=CARTESIAN_POINT('Ctrl Pts',(-29.6007527034052,8.92734279840361,135.704587303278));
#40538=CARTESIAN_POINT('Ctrl Pts',(-29.4383712024403,8.93082748462832,135.75478622414));
#40539=CARTESIAN_POINT('Ctrl Pts',(-29.4178151140962,8.93117869608006,135.761502183691));
#40540=CARTESIAN_POINT('Ctrl Pts',(-29.3974533690467,8.9314743514781,135.768567514003));
#40541=CARTESIAN_POINT('Ctrl Pts',(-30.59160797831,8.9,135.8));
#40542=CARTESIAN_POINT('Ctrl Pts',(-30.5717096993844,8.9,135.793075305549));
#40543=CARTESIAN_POINT('Ctrl Pts',(-30.5516102843096,8.89991869112576,135.786494096152));
#40544=CARTESIAN_POINT('Ctrl Pts',(-30.3926732691942,8.89858282731956,135.737144184887));
#40545=CARTESIAN_POINT('Ctrl Pts',(-30.1719936838072,8.89366846231917,135.699053886655));
#40546=CARTESIAN_POINT('Ctrl Pts',(-29.8281024878188,8.89363063009448,135.698923164311));
#40547=CARTESIAN_POINT('Ctrl Pts',(-29.607300083289,8.89857938931841,135.737132285728));
#40548=CARTESIAN_POINT('Ctrl Pts',(-29.4483922838095,8.89991862103249,135.78649385511));
#40549=CARTESIAN_POINT('Ctrl Pts',(-29.4282903006156,8.9,135.793075305549));
#40550=CARTESIAN_POINT('Ctrl Pts',(-29.40839202169,8.9,135.8));
#40551=CARTESIAN_POINT('',(-29.40839202169,8.9,135.8));
#40552=CARTESIAN_POINT('',(-29.40839202169,8.9,135.8));
#40553=CARTESIAN_POINT('',(-30.59160797831,8.9,135.8));
#40554=CARTESIAN_POINT('',(-30.62442393624,8.99442305443429,135.70570254201));
#40555=CARTESIAN_POINT('Ctrl Pts',(-30.59160797831,8.9,135.8));
#40556=CARTESIAN_POINT('Ctrl Pts',(-30.5717096993844,8.9,135.793075305549));
#40557=CARTESIAN_POINT('Ctrl Pts',(-30.5516102843096,8.89991869112576,135.786494096152));
#40558=CARTESIAN_POINT('Ctrl Pts',(-30.3926732691942,8.89858282731956,135.737144184887));
#40559=CARTESIAN_POINT('Ctrl Pts',(-30.1719936838072,8.89366846231917,135.699053886655));
#40560=CARTESIAN_POINT('Ctrl Pts',(-29.8281024878188,8.89363063009448,135.698923164311));
#40561=CARTESIAN_POINT('Ctrl Pts',(-29.607300083289,8.89857938931841,135.737132285728));
#40562=CARTESIAN_POINT('Ctrl Pts',(-29.4483922838095,8.89991862103249,135.78649385511));
#40563=CARTESIAN_POINT('Ctrl Pts',(-29.4282903006156,8.9,135.793075305549));
#40564=CARTESIAN_POINT('Ctrl Pts',(-29.40839202169,8.9,135.8));
#40565=CARTESIAN_POINT('Ctrl Pts',(-30.8485281374239,9.,135.8));
#40566=CARTESIAN_POINT('Ctrl Pts',(-30.7759616147067,9.,135.763779566847));
#40567=CARTESIAN_POINT('Ctrl Pts',(-30.7010733797628,8.99756721057679,135.732190956222));
#40568=CARTESIAN_POINT('Ctrl Pts',(-30.62442393624,8.99442305443429,135.70570254201));
#40569=CARTESIAN_POINT('Ctrl Pts',(-30.8336416788726,8.96666666666667,135.829824561404));
#40570=CARTESIAN_POINT('Ctrl Pts',(-30.7623482530451,8.96666666666667,135.794239574446));
#40571=CARTESIAN_POINT('Ctrl Pts',(-30.6887737535176,8.96504480705119,135.763211800971));
#40572=CARTESIAN_POINT('Ctrl Pts',(-30.6134852835966,8.96294870295619,135.737135028007));
#40573=CARTESIAN_POINT('Ctrl Pts',(-30.8187552203213,8.93333333333333,135.859649122807));
#40574=CARTESIAN_POINT('Ctrl Pts',(-30.7487348913836,8.93333333333333,135.824699582045));
#40575=CARTESIAN_POINT('Ctrl Pts',(-30.6764741272724,8.9325224035256,135.79423264572));
#40576=CARTESIAN_POINT('Ctrl Pts',(-30.6025466309533,8.9314743514781,135.768567514003));
#40577=CARTESIAN_POINT('Ctrl Pts',(-30.80386876177,8.9,135.889473684211));
#40578=CARTESIAN_POINT('Ctrl Pts',(-30.7351215297221,8.9,135.855159589644));
#40579=CARTESIAN_POINT('Ctrl Pts',(-30.6641745010272,8.9,135.825253490469));
#40580=CARTESIAN_POINT('Ctrl Pts',(-30.59160797831,8.9,135.8));
#40581=CARTESIAN_POINT('Ctrl Pts',(-30.80386876177,8.9,135.889473684211));
#40582=CARTESIAN_POINT('Ctrl Pts',(-30.7351215297221,8.9,135.855159589644));
#40583=CARTESIAN_POINT('Ctrl Pts',(-30.6641745010272,8.9,135.825253490469));
#40584=CARTESIAN_POINT('Ctrl Pts',(-30.59160797831,8.9,135.8));
#40585=CARTESIAN_POINT('Ctrl Pts',(-29.37557606376,8.99442305443429,135.70570254201));
#40586=CARTESIAN_POINT('Ctrl Pts',(-29.2989266202368,8.99756721057681,135.732190956222));
#40587=CARTESIAN_POINT('Ctrl Pts',(-29.2240383852925,9.00000000000003,135.763779566847));
#40588=CARTESIAN_POINT('Ctrl Pts',(-29.1514718625749,9.,135.800000000001));
#40589=CARTESIAN_POINT('Ctrl Pts',(-29.3865147164033,8.96294870295619,135.737135028007));
#40590=CARTESIAN_POINT('Ctrl Pts',(-29.311226246482,8.96504480705121,135.763211800971));
#40591=CARTESIAN_POINT('Ctrl Pts',(-29.237651746954,8.96666666666669,135.794239574446));
#40592=CARTESIAN_POINT('Ctrl Pts',(-29.1663583211262,8.96666666666667,135.829824561404));
#40593=CARTESIAN_POINT('Ctrl Pts',(-29.3974533690467,8.9314743514781,135.768567514003));
#40594=CARTESIAN_POINT('Ctrl Pts',(-29.3235258727272,8.9325224035256,135.79423264572));
#40595=CARTESIAN_POINT('Ctrl Pts',(-29.2512651086155,8.93333333333334,135.824699582045));
#40596=CARTESIAN_POINT('Ctrl Pts',(-29.1812447796775,8.93333333333333,135.859649122808));
#40597=CARTESIAN_POINT('Ctrl Pts',(-29.40839202169,8.9,135.8));
#40598=CARTESIAN_POINT('Ctrl Pts',(-29.3358254989724,8.9,135.825253490469));
#40599=CARTESIAN_POINT('Ctrl Pts',(-29.2648784702771,8.9,135.855159589645));
#40600=CARTESIAN_POINT('Ctrl Pts',(-29.1961312382288,8.9,135.889473684211));
#40601=CARTESIAN_POINT('Ctrl Pts',(-29.40839202169,8.9,135.8));
#40602=CARTESIAN_POINT('Ctrl Pts',(-29.3358254989724,8.9,135.825253490469));
#40603=CARTESIAN_POINT('Ctrl Pts',(-29.2648784702771,8.9,135.855159589645));
#40604=CARTESIAN_POINT('Ctrl Pts',(-29.1961312382288,8.9,135.889473684211));
#40605=CARTESIAN_POINT('Origin',(-30.,9.1,137.5));
#40606=CARTESIAN_POINT('',(-31.8,8.5,137.5));
#40607=CARTESIAN_POINT('',(-31.8,9.1,137.5));
#40608=CARTESIAN_POINT('',(-31.1048119379707,8.5,136.078947368421));
#40609=CARTESIAN_POINT('Origin',(-30.,8.5,137.5));
#40610=CARTESIAN_POINT('',(-30.9949874371066,8.5,136.));
#40611=CARTESIAN_POINT('Ctrl Pts',(-30.9949874371066,8.5,136.));
#40612=CARTESIAN_POINT('Ctrl Pts',(-31.0325673132895,8.5,136.024927669793));
#40613=CARTESIAN_POINT('Ctrl Pts',(-31.0692099500079,8.5,136.051268237865));
#40614=CARTESIAN_POINT('Ctrl Pts',(-31.1048119379707,8.5,136.078947368421));
#40615=CARTESIAN_POINT('',(-29.0050125628934,8.5,136.));
#40616=CARTESIAN_POINT('Ctrl Pts',(-29.0050125628934,8.5,136.));
#40617=CARTESIAN_POINT('Ctrl Pts',(-29.0135741934101,8.5,135.994320856796));
#40618=CARTESIAN_POINT('Ctrl Pts',(-29.0221618769299,8.4998881340947,135.988729270797));
#40619=CARTESIAN_POINT('Ctrl Pts',(-29.0307744240967,8.49967145659893,135.98322540583));
#40620=CARTESIAN_POINT('Ctrl Pts',(-29.0424857121922,8.49937681988721,135.975741284465));
#40621=CARTESIAN_POINT('Ctrl Pts',(-29.0542374418331,8.49890259856716,135.968422529549));
#40622=CARTESIAN_POINT('Ctrl Pts',(-29.0660378041393,8.49823351737356,135.961258388211));
#40623=CARTESIAN_POINT('Ctrl Pts',(-29.2617610405741,8.48713599907278,135.842432466379));
#40624=CARTESIAN_POINT('Ctrl Pts',(-29.4674506362191,8.43232113429692,135.768015720858));
#40625=CARTESIAN_POINT('Ctrl Pts',(-29.6708139777886,8.3968702701052,135.730147139424));
#40626=CARTESIAN_POINT('Ctrl Pts',(-29.7386017583118,8.38505331537463,135.717524278947));
#40627=CARTESIAN_POINT('Ctrl Pts',(-29.8061310661599,8.37538791626452,135.70896232559));
#40628=CARTESIAN_POINT('Ctrl Pts',(-29.8734626000106,8.36988598131075,135.704221903287));
#40629=CARTESIAN_POINT('Ctrl Pts',(-29.8963182945236,8.36801834905373,135.702612766559));
#40630=CARTESIAN_POINT('Ctrl Pts',(-29.9191264886051,8.36662503132851,135.701446014514));
#40631=CARTESIAN_POINT('Ctrl Pts',(-29.9419585439552,8.36574539366428,135.70071174992));
#40632=CARTESIAN_POINT('Ctrl Pts',(-29.9529619128661,8.36532147310264,135.70035788847));
#40633=CARTESIAN_POINT('Ctrl Pts',(-29.963955947468,8.365017872708,135.700106267193));
#40634=CARTESIAN_POINT('Ctrl Pts',(-29.9749570822295,8.36483405979636,135.699953932128));
#40635=CARTESIAN_POINT('Ctrl Pts',(-30.0209171987356,8.36406613330358,135.699317512567));
#40636=CARTESIAN_POINT('Ctrl Pts',(-30.0667990439102,8.36546505443102,135.700441545656));
#40637=CARTESIAN_POINT('Ctrl Pts',(-30.1127851886818,8.36886140284237,135.703319027213));
#40638=CARTESIAN_POINT('Ctrl Pts',(-30.1465700186564,8.37135661208814,135.705433038415));
#40639=CARTESIAN_POINT('Ctrl Pts',(-30.180449969916,8.37490071039504,135.70857305589));
#40640=CARTESIAN_POINT('Ctrl Pts',(-30.2142551605804,8.37930108895793,135.712568730666));
#40641=CARTESIAN_POINT('Ctrl Pts',(-30.4121935701959,8.40506647934105,135.735964472415));
#40642=CARTESIAN_POINT('Ctrl Pts',(-30.618223774017,8.46017177748985,135.795991006846));
#40643=CARTESIAN_POINT('Ctrl Pts',(-30.8090649857056,8.48601923378611,135.891967734795));
#40644=CARTESIAN_POINT('Ctrl Pts',(-30.8726787229352,8.49463505255153,135.923959977444));
#40645=CARTESIAN_POINT('Ctrl Pts',(-30.9346047943722,8.5,135.95994668604));
#40646=CARTESIAN_POINT('Ctrl Pts',(-30.9949874371066,8.5,136.));
#40647=CARTESIAN_POINT('',(-28.8951880620293,8.5,136.078947368421));
#40648=CARTESIAN_POINT('Ctrl Pts',(-28.8951880620293,8.5,136.078947368421));
#40649=CARTESIAN_POINT('Ctrl Pts',(-28.9307900499921,8.5,136.051268237865));
#40650=CARTESIAN_POINT('Ctrl Pts',(-28.9674326867105,8.5,136.024927669793));
#40651=CARTESIAN_POINT('Ctrl Pts',(-29.0050125628934,8.5,136.));
#40652=CARTESIAN_POINT('Origin',(-30.,8.5,137.5));
#40653=CARTESIAN_POINT('Ctrl Pts',(-28.9499455367427,8.39129047171135,135.916983334517));
#40654=CARTESIAN_POINT('Ctrl Pts',(-28.9583427274828,8.39013445090615,135.911534549944));
#40655=CARTESIAN_POINT('Ctrl Pts',(-28.966772971137,8.38888029152069,135.906181580337));
#40656=CARTESIAN_POINT('Ctrl Pts',(-28.9867478988158,8.38570733772648,135.893774692507));
#40657=CARTESIAN_POINT('Ctrl Pts',(-28.9983001592736,8.38372057934384,135.886804200101));
#40658=CARTESIAN_POINT('Ctrl Pts',(-29.2030969044704,8.34597008112109,135.767178547826));
#40659=CARTESIAN_POINT('Ctrl Pts',(-29.4772754648992,8.24903543084451,135.680444681192));
#40660=CARTESIAN_POINT('Ctrl Pts',(-29.7775051143642,8.19662294325174,135.651344091606));
#40661=CARTESIAN_POINT('Ctrl Pts',(-29.8804218187696,8.1865934232616,135.645948287097));
#40662=CARTESIAN_POINT('Ctrl Pts',(-29.9066026001864,8.18468277370489,135.644958149235));
#40663=CARTESIAN_POINT('Ctrl Pts',(-29.945607880728,8.18289720095053,135.6440346745));
#40664=CARTESIAN_POINT('Ctrl Pts',(-29.9583002059055,8.18248038026162,135.643821210287));
#40665=CARTESIAN_POINT('Ctrl Pts',(-30.0241258793722,8.18117464424746,135.643151906577));
#40666=CARTESIAN_POINT('Ctrl Pts',(-30.0772899664358,8.18310206076612,135.644103777041));
#40667=CARTESIAN_POINT('Ctrl Pts',(-30.1685015966763,8.19115568892363,135.648342005986));
#40668=CARTESIAN_POINT('Ctrl Pts',(-30.2068474352435,8.19595429131145,135.651012005824));
#40669=CARTESIAN_POINT('Ctrl Pts',(-30.465694468065,8.23688803331381,135.674362854996));
#40670=CARTESIAN_POINT('Ctrl Pts',(-30.7462229722334,8.33190850945499,135.742786049171));
#40671=CARTESIAN_POINT('Ctrl Pts',(-30.9908315655339,8.38313739956722,135.87855467171));
#40672=CARTESIAN_POINT('Ctrl Pts',(-31.0500544632574,8.39129047171136,135.916983334517));
#40673=CARTESIAN_POINT('Ctrl Pts',(-28.9683012121262,8.4275269811409,135.944655556345));
#40674=CARTESIAN_POINT('Ctrl Pts',(-28.9767482458833,8.42675447068797,135.939129772415));
#40675=CARTESIAN_POINT('Ctrl Pts',(-28.9852428165901,8.4258854532691,135.933697780808));
#40676=CARTESIAN_POINT('Ctrl Pts',(-29.0053155369763,8.42359293603061,135.921096409854));
#40677=CARTESIAN_POINT('Ctrl Pts',(-29.0169595159405,8.42211931541817,135.914010922128));
#40678=CARTESIAN_POINT('Ctrl Pts',(-29.2225856050001,8.39302212150272,135.792260131076));
#40679=CARTESIAN_POINT('Ctrl Pts',(-29.4968121969792,8.30401382953196,135.701370817213));
#40680=CARTESIAN_POINT('Ctrl Pts',(-29.7870605852856,8.25623003142132,135.670553593888));
#40681=CARTESIAN_POINT('Ctrl Pts',(-29.88567998585,8.24706050714524,135.664841173047));
#40682=CARTESIAN_POINT('Ctrl Pts',(-29.9107585634698,8.24533390764406,135.663791948766));
#40683=CARTESIAN_POINT('Ctrl Pts',(-29.9480281814684,8.24370245708609,135.662813622199));
#40684=CARTESIAN_POINT('Ctrl Pts',(-29.9601594059379,8.24332623806954,135.662587713756));
#40685=CARTESIAN_POINT('Ctrl Pts',(-30.0230260928526,8.242135170428,135.661877452567));
#40686=CARTESIAN_POINT('Ctrl Pts',(-30.0737662618809,8.243894603273,135.662889336933));
#40687=CARTESIAN_POINT('Ctrl Pts',(-30.1611638741047,8.25121736432493,135.66737577025));
#40688=CARTESIAN_POINT('Ctrl Pts',(-30.1980240267559,8.25561494071651,135.670207472671));
#40689=CARTESIAN_POINT('Ctrl Pts',(-30.4478023473742,8.29287747645514,135.694882333825));
#40690=CARTESIAN_POINT('Ctrl Pts',(-30.7264868782781,8.38080329713428,135.767194847034));
#40691=CARTESIAN_POINT('Ctrl Pts',(-30.9720741462826,8.42207265865225,135.90569558041));
#40692=CARTESIAN_POINT('Ctrl Pts',(-31.0316987878738,8.4275269811409,135.944655556345));
#40693=CARTESIAN_POINT('Ctrl Pts',(-28.9866568875098,8.46376349057045,135.972327778172));
#40694=CARTESIAN_POINT('Ctrl Pts',(-28.9951686750096,8.46337998021818,135.966725634326));
#40695=CARTESIAN_POINT('Ctrl Pts',(-29.0036920314769,8.46288297234629,135.961213070326));
#40696=CARTESIAN_POINT('Ctrl Pts',(-29.0239180740316,8.46149122158308,135.948419567118));
#40697=CARTESIAN_POINT('Ctrl Pts',(-29.0355780851662,8.46050386249283,135.941215807522));
#40698=CARTESIAN_POINT('Ctrl Pts',(-29.2422723400444,8.44008395869115,135.817350883128));
#40699=CARTESIAN_POINT('Ctrl Pts',(-29.5164771026875,8.35907111401752,135.722284002996));
#40700=CARTESIAN_POINT('Ctrl Pts',(-29.7965755952385,8.31578082809494,135.689752823308));
#40701=CARTESIAN_POINT('Ctrl Pts',(-29.8910601274432,8.3075512651701,135.683719880609));
#40702=CARTESIAN_POINT('Ctrl Pts',(-29.9149705253217,8.30597389738934,135.682612214983));
#40703=CARTESIAN_POINT('Ctrl Pts',(-29.9505416121257,8.30451621696708,135.681578940771));
#40704=CARTESIAN_POINT('Ctrl Pts',(-29.9620967474356,8.30417201490008,135.681339763724));
#40705=CARTESIAN_POINT('Ctrl Pts',(-30.0220169852552,8.30310560712303,135.680591966577));
#40706=CARTESIAN_POINT('Ctrl Pts',(-30.0703227484652,8.30467251192415,135.681655985765));
#40707=CARTESIAN_POINT('Ctrl Pts',(-30.153907741228,8.31129493668684,135.686399274151));
#40708=CARTESIAN_POINT('Ctrl Pts',(-30.1892733784037,8.31524006098998,135.689377589043));
#40709=CARTESIAN_POINT('Ctrl Pts',(-30.4300856908867,8.34907703619973,135.715444993586));
#40710=CARTESIAN_POINT('Ctrl Pts',(-30.7066366025794,8.42964542252683,135.791591053794));
#40711=CARTESIAN_POINT('Ctrl Pts',(-30.9533622136235,8.46106474091497,135.93280577734));
#40712=CARTESIAN_POINT('Ctrl Pts',(-31.0133431124902,8.46376349057045,135.972327778172));
#40713=CARTESIAN_POINT('Ctrl Pts',(-29.0050125628934,8.5,136.));
#40714=CARTESIAN_POINT('Ctrl Pts',(-29.01357419341,8.5,135.994320856796));
#40715=CARTESIAN_POINT('Ctrl Pts',(-29.0221618769299,8.4998881340947,135.988729270797));
#40716=CARTESIAN_POINT('Ctrl Pts',(-29.0424857121922,8.49937681988721,135.975741284465));
#40717=CARTESIAN_POINT('Ctrl Pts',(-29.0542374418331,8.49890259856716,135.968422529549));
#40718=CARTESIAN_POINT('Ctrl Pts',(-29.2617610405741,8.48713599907278,135.842432466379));
#40719=CARTESIAN_POINT('Ctrl Pts',(-29.5360138347675,8.41404951270497,135.743210139017));
#40720=CARTESIAN_POINT('Ctrl Pts',(-29.8061310661599,8.37538791626452,135.70896232559));
#40721=CARTESIAN_POINT('Ctrl Pts',(-29.8963182945236,8.36801834905373,135.702612766559));
#40722=CARTESIAN_POINT('Ctrl Pts',(-29.9191264886051,8.36662503132851,135.701446014514));
#40723=CARTESIAN_POINT('Ctrl Pts',(-29.9529619128661,8.36532147310264,135.70035788847));
#40724=CARTESIAN_POINT('Ctrl Pts',(-29.963955947468,8.365017872708,135.700106267193));
#40725=CARTESIAN_POINT('Ctrl Pts',(-30.0209171987356,8.36406613330358,135.699317512567));
#40726=CARTESIAN_POINT('Ctrl Pts',(-30.0667990439102,8.36546505443102,135.700441545656));
#40727=CARTESIAN_POINT('Ctrl Pts',(-30.1465700186564,8.37135661208814,135.705433038415));
#40728=CARTESIAN_POINT('Ctrl Pts',(-30.180449969916,8.37490071039504,135.70857305589));
#40729=CARTESIAN_POINT('Ctrl Pts',(-30.4121935701959,8.40506647934105,135.735964472415));
#40730=CARTESIAN_POINT('Ctrl Pts',(-30.6869005086241,8.47854021020612,135.815999851657));
#40731=CARTESIAN_POINT('Ctrl Pts',(-30.9346047943722,8.5,135.95994668604));
#40732=CARTESIAN_POINT('Ctrl Pts',(-30.9949874371067,8.5,136.));
#40733=CARTESIAN_POINT('',(-28.9499455367427,8.39129047171135,135.916983334517));
#40734=CARTESIAN_POINT('',(-30.9949874371066,8.5,136.));
#40735=CARTESIAN_POINT('Origin',(-30.,8.45,137.5));
#40736=CARTESIAN_POINT('',(-31.1661903789691,8.4,136.));
#40737=CARTESIAN_POINT('',(-28.8951880620293,8.5,136.078947368421));
#40738=CARTESIAN_POINT('Ctrl Pts',(-31.0500544632573,8.39129047171135,135.916983334517));
#40739=CARTESIAN_POINT('Ctrl Pts',(-31.0899798051577,8.39678689632762,135.942890163806));
#40740=CARTESIAN_POINT('Ctrl Pts',(-31.1286105039774,8.40000000009859,135.970783140825));
#40741=CARTESIAN_POINT('Ctrl Pts',(-31.1661903807052,8.4,136.00000000135));
#40742=CARTESIAN_POINT('Ctrl Pts',(-31.0316987878738,8.4275269811409,135.944655556345));
#40743=CARTESIAN_POINT('Ctrl Pts',(-31.0708423080613,8.43119126421841,135.970235999263));
#40744=CARTESIAN_POINT('Ctrl Pts',(-31.1088103196971,8.43333333339906,135.997611506775));
#40745=CARTESIAN_POINT('Ctrl Pts',(-31.145730900342,8.43333333333333,136.0263157908));
#40746=CARTESIAN_POINT('Ctrl Pts',(-31.0133431124902,8.46376349057045,135.972327778172));
#40747=CARTESIAN_POINT('Ctrl Pts',(-31.0517048109648,8.46559563210921,135.99758183472));
#40748=CARTESIAN_POINT('Ctrl Pts',(-31.0890101354168,8.46666666669953,136.024439872726));
#40749=CARTESIAN_POINT('Ctrl Pts',(-31.1252714199787,8.46666666666667,136.05263158025));
#40750=CARTESIAN_POINT('Ctrl Pts',(-30.9949874371066,8.5,136.));
#40751=CARTESIAN_POINT('Ctrl Pts',(-31.0325673138683,8.5,136.024927670177));
#40752=CARTESIAN_POINT('Ctrl Pts',(-31.0692099511365,8.5,136.051268238676));
#40753=CARTESIAN_POINT('Ctrl Pts',(-31.1048119396155,8.5,136.0789473697));
#40754=CARTESIAN_POINT('Ctrl Pts',(-28.833809621031,8.4,136.));
#40755=CARTESIAN_POINT('Ctrl Pts',(-28.8713894972139,8.4,135.970783139968));
#40756=CARTESIAN_POINT('Ctrl Pts',(-28.9100201954571,8.39678689624297,135.942890163407));
#40757=CARTESIAN_POINT('Ctrl Pts',(-28.9499455367427,8.39129047171135,135.916983334517));
#40758=CARTESIAN_POINT('Ctrl Pts',(-28.8542691013637,8.43333333333333,136.026315789474));
#40759=CARTESIAN_POINT('Ctrl Pts',(-28.8911896814733,8.43333333333333,135.997611505934));
#40760=CARTESIAN_POINT('Ctrl Pts',(-28.9291576925416,8.43119126416198,135.970235998869));
#40761=CARTESIAN_POINT('Ctrl Pts',(-28.9683012121263,8.4275269811409,135.944655556345));
#40762=CARTESIAN_POINT('Ctrl Pts',(-28.8747285816965,8.46666666666667,136.052631578947));
#40763=CARTESIAN_POINT('Ctrl Pts',(-28.9109898657327,8.46666666666667,136.024439871899));
#40764=CARTESIAN_POINT('Ctrl Pts',(-28.948295189626,8.46559563208099,135.997581834331));
#40765=CARTESIAN_POINT('Ctrl Pts',(-28.9866568875098,8.46376349057045,135.972327778172));
#40766=CARTESIAN_POINT('Ctrl Pts',(-28.8951880620293,8.5,136.078947368421));
#40767=CARTESIAN_POINT('Ctrl Pts',(-28.9307900499921,8.5,136.051268237865));
#40768=CARTESIAN_POINT('Ctrl Pts',(-28.9674326867105,8.5,136.024927669793));
#40769=CARTESIAN_POINT('Ctrl Pts',(-29.0050125628934,8.5,136.));
#40770=CARTESIAN_POINT('Ctrl Pts',(-29.37557606376,8.99442305443429,144.29429745799));
#40771=CARTESIAN_POINT('Ctrl Pts',(-29.3968663992163,8.99354972599348,144.301654944207));
#40772=CARTESIAN_POINT('Ctrl Pts',(-29.4183017778428,8.99262938553082,144.308615224025));
#40773=CARTESIAN_POINT('Ctrl Pts',(-29.5879618888624,8.98495073555583,144.36060019061));
#40774=CARTESIAN_POINT('Ctrl Pts',(-29.8570704543082,8.97294630891696,144.405692333025));
#40775=CARTESIAN_POINT('Ctrl Pts',(-30.1448589551985,8.97549033242365,144.39734513884));
#40776=CARTESIAN_POINT('Ctrl Pts',(-30.3737546351539,8.98306099714656,144.364880756376));
#40777=CARTESIAN_POINT('Ctrl Pts',(-30.4860772057434,8.98837707594693,144.337802199667));
#40778=CARTESIAN_POINT('Ctrl Pts',(-30.5816983343123,8.99261835182926,144.308632644433));
#40779=CARTESIAN_POINT('Ctrl Pts',(-30.6031336007837,8.99354972599348,144.301654944207));
#40780=CARTESIAN_POINT('Ctrl Pts',(-30.62442393624,8.99442305443429,144.29429745799));
#40781=CARTESIAN_POINT('Ctrl Pts',(-29.3865147164033,8.96294870295619,144.262864971993));
#40782=CARTESIAN_POINT('Ctrl Pts',(-29.4073401763186,8.96237080371183,144.270080554424));
#40783=CARTESIAN_POINT('Ctrl Pts',(-29.4283245709687,8.96172080327479,144.276909137492));
#40784=CARTESIAN_POINT('Ctrl Pts',(-29.594500212573,8.95618570956421,144.328046949343));
#40785=CARTESIAN_POINT('Ctrl Pts',(-29.8591950711281,8.94617889889013,144.372922700884));
#40786=CARTESIAN_POINT('Ctrl Pts',(-30.1426748215025,8.9483374189058,144.364588161718));
#40787=CARTESIAN_POINT('Ctrl Pts',(-30.3677623300152,8.95450008198494,144.332371964081));
#40788=CARTESIAN_POINT('Ctrl Pts',(-30.4780285068212,8.95865448574558,144.305612529178));
#40789=CARTESIAN_POINT('Ctrl Pts',(-30.5716737135296,8.96171637278058,144.276928607877));
#40790=CARTESIAN_POINT('Ctrl Pts',(-30.5926609072949,8.96236576597913,144.270078935029));
#40791=CARTESIAN_POINT('Ctrl Pts',(-30.6134852835967,8.96294870295619,144.262864971993));
#40792=CARTESIAN_POINT('Ctrl Pts',(-29.3974533690467,8.9314743514781,144.231432485996));
#40793=CARTESIAN_POINT('Ctrl Pts',(-29.4178165235133,8.93117892228165,144.238499084234));
#40794=CARTESIAN_POINT('Ctrl Pts',(-29.4383449914353,8.93082558456286,144.245210604997));
#40795=CARTESIAN_POINT('Ctrl Pts',(-29.6010478149954,8.92735264779638,144.295449195762));
#40796=CARTESIAN_POINT('Ctrl Pts',(-29.861341108549,8.91940129063077,144.340159362869));
#40797=CARTESIAN_POINT('Ctrl Pts',(-30.1404741111915,8.92117778746871,144.331810860123));
#40798=CARTESIAN_POINT('Ctrl Pts',(-30.3617899054628,8.9259156506157,144.299860032397));
#40799=CARTESIAN_POINT('Ctrl Pts',(-30.4699427746209,8.92894383621034,144.273406936258));
#40800=CARTESIAN_POINT('Ctrl Pts',(-30.5616573345954,8.93081126954196,144.245227705831));
#40801=CARTESIAN_POINT('Ctrl Pts',(-30.5821823928732,8.93118396001435,144.238500703629));
#40802=CARTESIAN_POINT('Ctrl Pts',(-30.6025466309533,8.9314743514781,144.231432485997));
#40803=CARTESIAN_POINT('Ctrl Pts',(-29.40839202169,8.9,144.2));
#40804=CARTESIAN_POINT('Ctrl Pts',(-29.4282903006156,8.9,144.206924694451));
#40805=CARTESIAN_POINT('Ctrl Pts',(-29.4483677845611,8.89991700230683,144.213504518463));
#40806=CARTESIAN_POINT('Ctrl Pts',(-29.607586138706,8.89858762180476,144.262895954495));
#40807=CARTESIAN_POINT('Ctrl Pts',(-29.8634657253689,8.89263388060395,144.307389730728));
#40808=CARTESIAN_POINT('Ctrl Pts',(-30.1382899774955,8.89402487395086,144.299053883001));
#40809=CARTESIAN_POINT('Ctrl Pts',(-30.3557976003241,8.89735473545407,144.267351240102));
#40810=CARTESIAN_POINT('Ctrl Pts',(-30.4618940756987,8.899221246009,144.241217265769));
#40811=CARTESIAN_POINT('Ctrl Pts',(-30.5516327138128,8.89990929049328,144.213523669276));
#40812=CARTESIAN_POINT('Ctrl Pts',(-30.5717096993844,8.9,144.206924694451));
#40813=CARTESIAN_POINT('Ctrl Pts',(-30.59160797831,8.9,144.2));
#40814=CARTESIAN_POINT('',(-30.59160797831,8.9,144.2));
#40815=CARTESIAN_POINT('',(-30.59160797831,8.9,144.2));
#40816=CARTESIAN_POINT('',(-29.40839202169,8.9,144.2));
#40817=CARTESIAN_POINT('',(-29.37557606376,8.99442305443429,144.29429745799));
#40818=CARTESIAN_POINT('Ctrl Pts',(-29.40839202169,8.9,144.2));
#40819=CARTESIAN_POINT('Ctrl Pts',(-29.4282903006156,8.9,144.206924694451));
#40820=CARTESIAN_POINT('Ctrl Pts',(-29.4483677845611,8.89991700230683,144.213504518463));
#40821=CARTESIAN_POINT('Ctrl Pts',(-29.607586138706,8.89858762180476,144.262895954495));
#40822=CARTESIAN_POINT('Ctrl Pts',(-29.8634657253689,8.89263388060395,144.307389730728));
#40823=CARTESIAN_POINT('Ctrl Pts',(-30.1382899774955,8.89402487395086,144.299053883001));
#40824=CARTESIAN_POINT('Ctrl Pts',(-30.3557976003241,8.89735473545407,144.267351240102));
#40825=CARTESIAN_POINT('Ctrl Pts',(-30.4618940756987,8.899221246009,144.241217265769));
#40826=CARTESIAN_POINT('Ctrl Pts',(-30.5516327138128,8.89990929049328,144.213523669276));
#40827=CARTESIAN_POINT('Ctrl Pts',(-30.5717096993844,8.9,144.206924694451));
#40828=CARTESIAN_POINT('Ctrl Pts',(-30.59160797831,8.9,144.2));
#40829=CARTESIAN_POINT('Origin',(-30.,8.95,142.5));
#40830=CARTESIAN_POINT('',(-30.80386876177,8.9,144.110526315789));
#40831=CARTESIAN_POINT('',(-30.8485281374239,9.,144.2));
#40832=CARTESIAN_POINT('',(-31.8,8.9,142.5));
#40833=CARTESIAN_POINT('Origin',(-30.,8.9,142.5));
#40834=CARTESIAN_POINT('',(-29.19613123823,8.9,144.110526315789));
#40835=CARTESIAN_POINT('Origin',(-30.,8.9,142.5));
#40836=CARTESIAN_POINT('',(-29.19613123823,8.9,144.110526315789));
#40837=CARTESIAN_POINT('Ctrl Pts',(-30.62442393624,8.99442305443429,144.29429745799));
#40838=CARTESIAN_POINT('Ctrl Pts',(-30.7010733797632,8.99756721057681,144.267809043778));
#40839=CARTESIAN_POINT('Ctrl Pts',(-30.7759616147075,9.00000000000003,144.236220433153));
#40840=CARTESIAN_POINT('Ctrl Pts',(-30.8485281374251,9.,144.199999999999));
#40841=CARTESIAN_POINT('Ctrl Pts',(-30.6134852835967,8.96294870295619,144.262864971993));
#40842=CARTESIAN_POINT('Ctrl Pts',(-30.688773753518,8.96504480705121,144.236788199029));
#40843=CARTESIAN_POINT('Ctrl Pts',(-30.762348253046,8.96666666666669,144.205760425554));
#40844=CARTESIAN_POINT('Ctrl Pts',(-30.8336416788738,8.96666666666667,144.170175438596));
#40845=CARTESIAN_POINT('Ctrl Pts',(-30.6025466309533,8.9314743514781,144.231432485997));
#40846=CARTESIAN_POINT('Ctrl Pts',(-30.6764741272728,8.9325224035256,144.20576735428));
#40847=CARTESIAN_POINT('Ctrl Pts',(-30.7487348913845,8.93333333333334,144.175300417955));
#40848=CARTESIAN_POINT('Ctrl Pts',(-30.8187552203225,8.93333333333333,144.140350877192));
#40849=CARTESIAN_POINT('Ctrl Pts',(-30.59160797831,8.9,144.2));
#40850=CARTESIAN_POINT('Ctrl Pts',(-30.6641745010276,8.9,144.174746509531));
#40851=CARTESIAN_POINT('Ctrl Pts',(-30.7351215297229,8.9,144.144840410355));
#40852=CARTESIAN_POINT('Ctrl Pts',(-30.8038687617712,8.9,144.110526315789));
#40853=CARTESIAN_POINT('Ctrl Pts',(-30.59160797831,8.9,144.2));
#40854=CARTESIAN_POINT('Ctrl Pts',(-30.6641745010276,8.9,144.174746509531));
#40855=CARTESIAN_POINT('Ctrl Pts',(-30.7351215297229,8.9,144.144840410355));
#40856=CARTESIAN_POINT('Ctrl Pts',(-30.8038687617712,8.9,144.110526315789));
#40857=CARTESIAN_POINT('Ctrl Pts',(-29.1514718625761,9.,144.2));
#40858=CARTESIAN_POINT('Ctrl Pts',(-29.2240383852933,9.,144.236220433153));
#40859=CARTESIAN_POINT('Ctrl Pts',(-29.2989266202372,8.99756721057679,144.267809043778));
#40860=CARTESIAN_POINT('Ctrl Pts',(-29.37557606376,8.99442305443429,144.29429745799));
#40861=CARTESIAN_POINT('Ctrl Pts',(-29.1663583211274,8.96666666666667,144.170175438596));
#40862=CARTESIAN_POINT('Ctrl Pts',(-29.2376517469549,8.96666666666667,144.205760425554));
#40863=CARTESIAN_POINT('Ctrl Pts',(-29.3112262464824,8.96504480705119,144.236788199029));
#40864=CARTESIAN_POINT('Ctrl Pts',(-29.3865147164034,8.96294870295619,144.262864971993));
#40865=CARTESIAN_POINT('Ctrl Pts',(-29.1812447796787,8.93333333333333,144.140350877193));
#40866=CARTESIAN_POINT('Ctrl Pts',(-29.2512651086164,8.93333333333333,144.175300417955));
#40867=CARTESIAN_POINT('Ctrl Pts',(-29.3235258727276,8.9325224035256,144.20576735428));
#40868=CARTESIAN_POINT('Ctrl Pts',(-29.3974533690467,8.9314743514781,144.231432485997));
#40869=CARTESIAN_POINT('Ctrl Pts',(-29.19613123823,8.9,144.110526315789));
#40870=CARTESIAN_POINT('Ctrl Pts',(-29.2648784702779,8.9,144.144840410356));
#40871=CARTESIAN_POINT('Ctrl Pts',(-29.3358254989728,8.9,144.174746509531));
#40872=CARTESIAN_POINT('Ctrl Pts',(-29.40839202169,8.9,144.2));
#40873=CARTESIAN_POINT('Ctrl Pts',(-29.19613123823,8.9,144.110526315789));
#40874=CARTESIAN_POINT('Ctrl Pts',(-29.2648784702779,8.9,144.144840410356));
#40875=CARTESIAN_POINT('Ctrl Pts',(-29.3358254989728,8.9,144.174746509531));
#40876=CARTESIAN_POINT('Ctrl Pts',(-29.40839202169,8.9,144.2));
#40877=CARTESIAN_POINT('Origin',(-30.,9.1,142.5));
#40878=CARTESIAN_POINT('',(-31.8,8.5,142.5));
#40879=CARTESIAN_POINT('',(-31.8,9.1,142.5));
#40880=CARTESIAN_POINT('',(-28.8951880620293,8.5,143.921052631579));
#40881=CARTESIAN_POINT('Origin',(-30.,8.5,142.5));
#40882=CARTESIAN_POINT('',(-29.0050125628934,8.5,144.));
#40883=CARTESIAN_POINT('Ctrl Pts',(-29.0050125628934,8.5,144.));
#40884=CARTESIAN_POINT('Ctrl Pts',(-28.9674326867105,8.5,143.975072330207));
#40885=CARTESIAN_POINT('Ctrl Pts',(-28.9307900499921,8.5,143.948731762135));
#40886=CARTESIAN_POINT('Ctrl Pts',(-28.8951880620293,8.5,143.921052631579));
#40887=CARTESIAN_POINT('',(-30.9949874371066,8.5,144.));
#40888=CARTESIAN_POINT('Ctrl Pts',(-30.9949874371066,8.49999999999999,144.));
#40889=CARTESIAN_POINT('Ctrl Pts',(-30.9864258065899,8.49999999999999,144.005679143204));
#40890=CARTESIAN_POINT('Ctrl Pts',(-30.9778386719318,8.49988852054169,144.011270754062));
#40891=CARTESIAN_POINT('Ctrl Pts',(-30.9692250597263,8.49967146108473,144.016774507783));
#40892=CARTESIAN_POINT('Ctrl Pts',(-30.9575123233977,8.49937630498455,144.024258477877));
#40893=CARTESIAN_POINT('Ctrl Pts',(-30.9457720398319,8.49890718075588,144.031578258464));
#40894=CARTESIAN_POINT('Ctrl Pts',(-30.9339557366539,8.49823143451159,144.038740897101));
#40895=CARTESIAN_POINT('Ctrl Pts',(-30.6726388899699,8.48328734624167,144.197142227399));
#40896=CARTESIAN_POINT('Ctrl Pts',(-30.3955689407068,8.39161125939828,144.276735792559));
#40897=CARTESIAN_POINT('Ctrl Pts',(-30.1265319331592,8.36984745763126,144.295772364356));
#40898=CARTESIAN_POINT('Ctrl Pts',(-30.1037007747645,8.36800052657168,144.297387855808));
#40899=CARTESIAN_POINT('Ctrl Pts',(-30.0808712194313,8.36659012091945,144.298549094101));
#40900=CARTESIAN_POINT('Ctrl Pts',(-30.0580431077713,8.36571381605628,144.299284047477));
#40901=CARTESIAN_POINT('Ctrl Pts',(-30.0470416394284,8.36529150165926,144.299638240868));
#40902=CARTESIAN_POINT('Ctrl Pts',(-30.036044636314,8.36498601410341,144.299889873607));
#40903=CARTESIAN_POINT('Ctrl Pts',(-30.0250454942028,8.36480330495199,144.300041744189));
#40904=CARTESIAN_POINT('Ctrl Pts',(-30.0035042967233,8.36444547941686,144.300339174131));
#40905=CARTESIAN_POINT('Ctrl Pts',(-29.9819683006895,8.36455538212952,144.30024955842));
#40906=CARTESIAN_POINT('Ctrl Pts',(-29.9604261249166,8.36513079602048,144.299774357394));
#40907=CARTESIAN_POINT('Ctrl Pts',(-29.9360144221004,8.36578285795937,144.299235857181));
#40908=CARTESIAN_POINT('Ctrl Pts',(-29.9116476872554,8.36702849219147,144.298196931516));
#40909=CARTESIAN_POINT('Ctrl Pts',(-29.8872073846878,8.36883152973277,144.29666716382));
#40910=CARTESIAN_POINT('Ctrl Pts',(-29.8534067066909,8.37132511143786,144.294551511398));
#40911=CARTESIAN_POINT('Ctrl Pts',(-29.8195400563255,8.37487055555119,144.291412849903));
#40912=CARTESIAN_POINT('Ctrl Pts',(-29.7857330314176,8.3792716381878,144.287417383752));
#40913=CARTESIAN_POINT('Ctrl Pts',(-29.5877838818172,8.40504115111046,144.264022863562));
#40914=CARTESIAN_POINT('Ctrl Pts',(-29.3817727081634,8.46016437071621,144.204005312567));
#40915=CARTESIAN_POINT('Ctrl Pts',(-29.1909346646337,8.48601711341369,144.108031216413));
#40916=CARTESIAN_POINT('Ctrl Pts',(-29.1273219834571,8.49463469431285,144.076039851029));
#40917=CARTESIAN_POINT('Ctrl Pts',(-29.0653952056277,8.49999999999999,144.04005331396));
#40918=CARTESIAN_POINT('Ctrl Pts',(-29.0050125628934,8.49999999999999,144.));
#40919=CARTESIAN_POINT('',(-31.1048119379707,8.5,143.921052631579));
#40920=CARTESIAN_POINT('Ctrl Pts',(-31.1048119379707,8.5,143.921052631579));
#40921=CARTESIAN_POINT('Ctrl Pts',(-31.0692099500079,8.5,143.948731762135));
#40922=CARTESIAN_POINT('Ctrl Pts',(-31.0325673132895,8.5,143.975072330207));
#40923=CARTESIAN_POINT('Ctrl Pts',(-30.9949874371066,8.5,144.));
#40924=CARTESIAN_POINT('Origin',(-30.,8.5,142.5));
#40925=CARTESIAN_POINT('Ctrl Pts',(-31.0500544632573,8.39129047171135,144.083016665483));
#40926=CARTESIAN_POINT('Ctrl Pts',(-31.0416572725172,8.39013445090615,144.088465450056));
#40927=CARTESIAN_POINT('Ctrl Pts',(-31.0332270809276,8.38887970921002,144.093818628959));
#40928=CARTESIAN_POINT('Ctrl Pts',(-31.0132516281393,8.38570812580638,144.106224780502));
#40929=CARTESIAN_POINT('Ctrl Pts',(-31.0017014315445,8.38371364530919,144.113198879946));
#40930=CARTESIAN_POINT('Ctrl Pts',(-30.7324511236407,8.33432880803088,144.270318781487));
#40931=CARTESIAN_POINT('Ctrl Pts',(-30.4529311916243,8.21959507258029,144.336354071163));
#40932=CARTESIAN_POINT('Ctrl Pts',(-30.1195807496158,8.18661062269483,144.354047747419));
#40933=CARTESIAN_POINT('Ctrl Pts',(-30.0933941115233,8.18473112770877,144.355023956059));
#40934=CARTESIAN_POINT('Ctrl Pts',(-30.0543910542229,8.18293757017519,144.355950759946));
#40935=CARTESIAN_POINT('Ctrl Pts',(-30.0416959390612,8.18252195324135,144.35616358648));
#40936=CARTESIAN_POINT('Ctrl Pts',(-30.0040933217041,8.18177796546578,144.356545242999));
#40937=CARTESIAN_POINT('Ctrl Pts',(-29.9791722273264,8.18192966483189,144.356469222117));
#40938=CARTESIAN_POINT('Ctrl Pts',(-29.9261171052882,8.18361364393076,144.355609595774));
#40939=CARTESIAN_POINT('Ctrl Pts',(-29.8980661716417,8.18531958471388,144.354728185553));
#40940=CARTESIAN_POINT('Ctrl Pts',(-29.8314696713767,8.19118993782772,144.351632857542));
#40941=CARTESIAN_POINT('Ctrl Pts',(-29.7931403426605,8.19599191204271,144.348964017633));
#40942=CARTESIAN_POINT('Ctrl Pts',(-29.5342776523695,8.23691405320499,144.32561688535));
#40943=CARTESIAN_POINT('Ctrl Pts',(-29.2537806211792,8.33191174571249,144.257212629307));
#40944=CARTESIAN_POINT('Ctrl Pts',(-29.009168434466,8.38313739956723,144.121445328289));
#40945=CARTESIAN_POINT('Ctrl Pts',(-28.9499455367427,8.39129047171135,144.083016665483));
#40946=CARTESIAN_POINT('Ctrl Pts',(-31.0316987878738,8.4275269811409,144.055344443655));
#40947=CARTESIAN_POINT('Ctrl Pts',(-31.0232494782234,8.42674758136909,144.060871364535));
#40948=CARTESIAN_POINT('Ctrl Pts',(-31.0147604421638,8.4258945773603,144.066300826652));
#40949=CARTESIAN_POINT('Ctrl Pts',(-30.9946783468982,8.42357664552238,144.078905881521));
#40950=CARTESIAN_POINT('Ctrl Pts',(-30.9830491673224,8.42213380515014,144.085988624004));
#40951=CARTESIAN_POINT('Ctrl Pts',(-30.7126406025825,8.38391948813827,144.245935181324));
#40952=CARTESIAN_POINT('Ctrl Pts',(-30.4335871468451,8.27667769995428,144.316530411117));
#40953=CARTESIAN_POINT('Ctrl Pts',(-30.1143332642689,8.24713075999365,144.335146729607));
#40954=CARTESIAN_POINT('Ctrl Pts',(-30.0892321163076,8.24534698733409,144.336195530571));
#40955=CARTESIAN_POINT('Ctrl Pts',(-30.0519728840255,8.24375611845358,144.337169744628));
#40956=CARTESIAN_POINT('Ctrl Pts',(-30.03983621471,8.24336276859699,144.337398013963));
#40957=CARTESIAN_POINT('Ctrl Pts',(-30.0039249294193,8.24269311190836,144.337801203055));
#40958=CARTESIAN_POINT('Ctrl Pts',(-29.9801292530066,8.24282792333394,144.33772086074));
#40959=CARTESIAN_POINT('Ctrl Pts',(-29.9294428595935,8.24435853719646,144.33681052603));
#40960=CARTESIAN_POINT('Ctrl Pts',(-29.902618367519,8.24591603275185,144.335874860442));
#40961=CARTESIAN_POINT('Ctrl Pts',(-29.8388088722218,8.25125052269469,144.332599609949));
#40962=CARTESIAN_POINT('Ctrl Pts',(-29.8019634018542,8.25565283346855,144.329768423253));
#40963=CARTESIAN_POINT('Ctrl Pts',(-29.5521701639099,8.29290319017188,144.305097549906));
#40964=CARTESIAN_POINT('Ctrl Pts',(-29.2735164712547,8.3808067246845,144.232803741881));
#40965=CARTESIAN_POINT('Ctrl Pts',(-29.0279259249285,8.42207260275014,144.094304445759));
#40966=CARTESIAN_POINT('Ctrl Pts',(-28.9683012121263,8.4275269811409,144.055344443655));
#40967=CARTESIAN_POINT('Ctrl Pts',(-31.0133431124902,8.46376349057045,144.027672221828));
#40968=CARTESIAN_POINT('Ctrl Pts',(-31.0048336008837,8.46338686953705,144.033273228725));
#40969=CARTESIAN_POINT('Ctrl Pts',(-30.9963053106956,8.46287365239142,144.038788556369));
#40970=CARTESIAN_POINT('Ctrl Pts',(-30.9760856046388,8.46150778526856,144.051577376858));
#40971=CARTESIAN_POINT('Ctrl Pts',(-30.964424304054,8.46048702091494,144.058788514405));
#40972=CARTESIAN_POINT('Ctrl Pts',(-30.6924494110281,8.43369666613429,144.221525827561));
#40973=CARTESIAN_POINT('Ctrl Pts',(-30.4149129854861,8.33452863202431,144.296559452605));
#40974=CARTESIAN_POINT('Ctrl Pts',(-30.1089482601113,8.30748038927288,144.316288873621));
#40975=CARTESIAN_POINT('Ctrl Pts',(-30.085033214647,8.30597426129415,144.317377519589));
#40976=CARTESIAN_POINT('Ctrl Pts',(-30.0494598096259,8.30447295338088,144.318419256187));
#40977=CARTESIAN_POINT('Ctrl Pts',(-30.0379043606653,8.30414519874779,144.318655446124));
#40978=CARTESIAN_POINT('Ctrl Pts',(-30.0036726890082,8.3035303329743,144.319083214075));
#40979=CARTESIAN_POINT('Ctrl Pts',(-29.9810112750093,8.3036571236275,144.318997919797));
#40980=CARTESIAN_POINT('Ctrl Pts',(-29.9326886677951,8.30503796469369,144.318034926925));
#40981=CARTESIAN_POINT('Ctrl Pts',(-29.9070954913782,8.30643204415352,144.317050256628));
#40982=CARTESIAN_POINT('Ctrl Pts',(-29.8460675058458,8.31126452657091,144.31358475899));
#40983=CARTESIAN_POINT('Ctrl Pts',(-29.8107169971318,8.31520963412536,144.310608444283));
#40984=CARTESIAN_POINT('Ctrl Pts',(-29.5698913702768,8.34905201414359,144.284542199006));
#40985=CARTESIAN_POINT('Ctrl Pts',(-29.29336646687,8.42964379827947,144.208408349661));
#40986=CARTESIAN_POINT('Ctrl Pts',(-29.0466377151652,8.46106479681709,144.067194196491));
#40987=CARTESIAN_POINT('Ctrl Pts',(-28.9866568875098,8.46376349057045,144.027672221828));
#40988=CARTESIAN_POINT('Ctrl Pts',(-30.9949874371066,8.5,144.));
#40989=CARTESIAN_POINT('Ctrl Pts',(-30.9864258065899,8.5,144.005679143204));
#40990=CARTESIAN_POINT('Ctrl Pts',(-30.9778386719318,8.49988852054171,144.011270754062));
#40991=CARTESIAN_POINT('Ctrl Pts',(-30.9575123233977,8.49937630498457,144.024258477877));
#40992=CARTESIAN_POINT('Ctrl Pts',(-30.9457720398319,8.49890718075589,144.031578258464));
#40993=CARTESIAN_POINT('Ctrl Pts',(-30.6726388899699,8.48328734624168,144.197142227399));
#40994=CARTESIAN_POINT('Ctrl Pts',(-30.3955689407068,8.3916112593983,144.276735792559));
#40995=CARTESIAN_POINT('Ctrl Pts',(-30.1037007747645,8.3680005265717,144.297387855808));
#40996=CARTESIAN_POINT('Ctrl Pts',(-30.0808712194313,8.36659012091947,144.298549094101));
#40997=CARTESIAN_POINT('Ctrl Pts',(-30.0470416394284,8.36529150165928,144.299638240868));
#40998=CARTESIAN_POINT('Ctrl Pts',(-30.036044636314,8.36498601410343,144.299889873607));
#40999=CARTESIAN_POINT('Ctrl Pts',(-30.0035042967233,8.36444547941688,144.300339174131));
#41000=CARTESIAN_POINT('Ctrl Pts',(-29.9819683006895,8.36455538212954,144.30024955842));
#41001=CARTESIAN_POINT('Ctrl Pts',(-29.9360144221004,8.36578285795938,144.299235857181));
#41002=CARTESIAN_POINT('Ctrl Pts',(-29.9116476872554,8.36702849219149,144.298196931516));
#41003=CARTESIAN_POINT('Ctrl Pts',(-29.8534067066909,8.37132511143788,144.294551511398));
#41004=CARTESIAN_POINT('Ctrl Pts',(-29.8195400563255,8.3748705555512,144.291412849903));
#41005=CARTESIAN_POINT('Ctrl Pts',(-29.5877838818172,8.40504115111048,144.264022863562));
#41006=CARTESIAN_POINT('Ctrl Pts',(-29.3131023169455,8.47853877725148,144.183999462235));
#41007=CARTESIAN_POINT('Ctrl Pts',(-29.0653952056277,8.5,144.04005331396));
#41008=CARTESIAN_POINT('Ctrl Pts',(-29.0050125628934,8.5,144.));
#41009=CARTESIAN_POINT('',(-31.0500544632573,8.39129047171135,144.083016665483));
#41010=CARTESIAN_POINT('',(-29.0050125628934,8.5,144.));
#41011=CARTESIAN_POINT('Origin',(-30.,8.45,142.5));
#41012=CARTESIAN_POINT('',(-28.8338096210309,8.4,144.));
#41013=CARTESIAN_POINT('',(-31.1048119379707,8.5,143.921052631579));
#41014=CARTESIAN_POINT('Ctrl Pts',(-28.9499455367427,8.39129047171135,144.083016665483));
#41015=CARTESIAN_POINT('Ctrl Pts',(-28.9100201948423,8.39678689632762,144.057109836194));
#41016=CARTESIAN_POINT('Ctrl Pts',(-28.8713894960226,8.40000000009859,144.029216859175));
#41017=CARTESIAN_POINT('Ctrl Pts',(-28.8338096192947,8.4,143.99999999865));
#41018=CARTESIAN_POINT('Ctrl Pts',(-28.9683012121262,8.4275269811409,144.055344443655));
#41019=CARTESIAN_POINT('Ctrl Pts',(-28.9291576919387,8.43119126421841,144.029764000737));
#41020=CARTESIAN_POINT('Ctrl Pts',(-28.8911896803029,8.43333333339906,144.002388493225));
#41021=CARTESIAN_POINT('Ctrl Pts',(-28.854269099658,8.43333333333333,143.9736842092));
#41022=CARTESIAN_POINT('Ctrl Pts',(-28.9866568875098,8.46376349057045,144.027672221828));
#41023=CARTESIAN_POINT('Ctrl Pts',(-28.9482951890352,8.46559563210921,144.00241816528));
#41024=CARTESIAN_POINT('Ctrl Pts',(-28.9109898645832,8.46666666669953,143.975560127274));
#41025=CARTESIAN_POINT('Ctrl Pts',(-28.8747285800212,8.46666666666667,143.94736841975));
#41026=CARTESIAN_POINT('Ctrl Pts',(-29.0050125628934,8.5,144.));
#41027=CARTESIAN_POINT('Ctrl Pts',(-28.9674326861317,8.5,143.975072329823));
#41028=CARTESIAN_POINT('Ctrl Pts',(-28.9307900488635,8.5,143.948731761324));
#41029=CARTESIAN_POINT('Ctrl Pts',(-28.8951880603845,8.5,143.9210526303));
#41030=CARTESIAN_POINT('Ctrl Pts',(-31.166190378969,8.4,144.));
#41031=CARTESIAN_POINT('Ctrl Pts',(-31.1286105027861,8.4,144.029216860032));
#41032=CARTESIAN_POINT('Ctrl Pts',(-31.0899798045429,8.39678689624297,144.057109836593));
#41033=CARTESIAN_POINT('Ctrl Pts',(-31.0500544632573,8.39129047171135,144.083016665483));
#41034=CARTESIAN_POINT('Ctrl Pts',(-31.1457308986363,8.43333333333333,143.973684210526));
#41035=CARTESIAN_POINT('Ctrl Pts',(-31.1088103185267,8.43333333333333,144.002388494066));
#41036=CARTESIAN_POINT('Ctrl Pts',(-31.0708423074584,8.43119126416198,144.029764001131));
#41037=CARTESIAN_POINT('Ctrl Pts',(-31.0316987878737,8.4275269811409,144.055344443655));
#41038=CARTESIAN_POINT('Ctrl Pts',(-31.1252714183035,8.46666666666667,143.947368421053));
#41039=CARTESIAN_POINT('Ctrl Pts',(-31.0890101342673,8.46666666666667,143.975560128101));
#41040=CARTESIAN_POINT('Ctrl Pts',(-31.051704810374,8.46559563208099,144.002418165669));
#41041=CARTESIAN_POINT('Ctrl Pts',(-31.0133431124902,8.46376349057045,144.027672221828));
#41042=CARTESIAN_POINT('Ctrl Pts',(-31.1048119379707,8.5,143.921052631579));
#41043=CARTESIAN_POINT('Ctrl Pts',(-31.0692099500079,8.5,143.948731762135));
#41044=CARTESIAN_POINT('Ctrl Pts',(-31.0325673132895,8.5,143.975072330207));
#41045=CARTESIAN_POINT('Ctrl Pts',(-30.9949874371066,8.5,144.));
#41046=CARTESIAN_POINT('Origin',(30.,8.95,137.5));
#41047=CARTESIAN_POINT('',(30.80386876177,8.9,135.889473684211));
#41048=CARTESIAN_POINT('',(30.8485281374239,9.,135.8));
#41049=CARTESIAN_POINT('',(28.2,8.9,137.5));
#41050=CARTESIAN_POINT('Origin',(30.,8.9,137.5));
#41051=CARTESIAN_POINT('',(29.19613123823,8.9,135.889473684211));
#41052=CARTESIAN_POINT('Origin',(30.,8.9,137.5));
#41053=CARTESIAN_POINT('',(29.19613123823,8.9,135.889473684211));
#41054=CARTESIAN_POINT('Ctrl Pts',(29.37557606376,8.99442305443429,135.70570254201));
#41055=CARTESIAN_POINT('Ctrl Pts',(29.3968663992163,8.99354972599348,135.698345055793));
#41056=CARTESIAN_POINT('Ctrl Pts',(29.4183247605901,8.99263100796461,135.691382689721));
#41057=CARTESIAN_POINT('Ctrl Pts',(29.5876905334005,8.98495128128084,135.639444028187));
#41058=CARTESIAN_POINT('Ctrl Pts',(29.8197767178098,8.97487183787893,135.600774173325));
#41059=CARTESIAN_POINT('Ctrl Pts',(30.1801225306472,8.97481364719588,135.600649477793));
#41060=CARTESIAN_POINT('Ctrl Pts',(30.4123373861891,8.9849459908676,135.639432675438));
#41061=CARTESIAN_POINT('Ctrl Pts',(30.581672548813,8.99263090028869,135.69138245992));
#41062=CARTESIAN_POINT('Ctrl Pts',(30.6031336007837,8.99354972599348,135.698345055793));
#41063=CARTESIAN_POINT('Ctrl Pts',(30.62442393624,8.99442305443429,135.70570254201));
#41064=CARTESIAN_POINT('Ctrl Pts',(29.3865147164033,8.96294870295619,135.737135028007));
#41065=CARTESIAN_POINT('Ctrl Pts',(29.4073414853149,8.96237089086999,135.729918298573));
#41066=CARTESIAN_POINT('Ctrl Pts',(29.4283459629072,8.96172231480688,135.723090172466));
#41067=CARTESIAN_POINT('Ctrl Pts',(29.5942372931042,8.95618694003155,135.671989821309));
#41068=CARTESIAN_POINT('Ctrl Pts',(29.8225190849717,8.94781763959254,135.633524301555));
#41069=CARTESIAN_POINT('Ctrl Pts',(30.1773808279966,8.94775803303614,135.63340083736));
#41070=CARTESIAN_POINT('Ctrl Pts',(30.4057900063053,8.9561825817824,135.671977657887));
#41071=CARTESIAN_POINT('Ctrl Pts',(30.5716514674437,8.96172203669286,135.723090090889));
#41072=CARTESIAN_POINT('Ctrl Pts',(30.5926584142642,8.96237102991341,135.729918177652));
#41073=CARTESIAN_POINT('Ctrl Pts',(30.6134852835967,8.96294870295619,135.737135028007));
#41074=CARTESIAN_POINT('Ctrl Pts',(29.3974533690467,8.9314743514781,135.768567514004));
#41075=CARTESIAN_POINT('Ctrl Pts',(29.417815214517,8.93117883512348,135.761502062769));
#41076=CARTESIAN_POINT('Ctrl Pts',(29.4383685133733,8.93082738428349,135.754786613407));
#41077=CARTESIAN_POINT('Ctrl Pts',(29.6007799711022,8.92734716856884,135.704598391766));
#41078=CARTESIAN_POINT('Ctrl Pts',(29.8252639490309,8.92072266060556,135.666303758425));
#41079=CARTESIAN_POINT('Ctrl Pts',(30.1746392148318,8.92068624425422,135.666171804744));
#41080=CARTESIAN_POINT('Ctrl Pts',(30.3992472965949,8.9273427984036,135.704587303278));
#41081=CARTESIAN_POINT('Ctrl Pts',(30.5616287975597,8.93082748462833,135.75478622414));
#41082=CARTESIAN_POINT('Ctrl Pts',(30.5821848859038,8.93117869608006,135.761502183691));
#41083=CARTESIAN_POINT('Ctrl Pts',(30.6025466309533,8.9314743514781,135.768567514004));
#41084=CARTESIAN_POINT('Ctrl Pts',(29.40839202169,8.9,135.8));
#41085=CARTESIAN_POINT('Ctrl Pts',(29.4282903006156,8.9,135.793075305549));
#41086=CARTESIAN_POINT('Ctrl Pts',(29.4483897156904,8.89991869112576,135.786494096152));
#41087=CARTESIAN_POINT('Ctrl Pts',(29.6073267308058,8.89858282731955,135.737144184887));
#41088=CARTESIAN_POINT('Ctrl Pts',(29.8280063161928,8.89366846231917,135.699053886655));
#41089=CARTESIAN_POINT('Ctrl Pts',(30.1718975121812,8.89363063009448,135.698923164311));
#41090=CARTESIAN_POINT('Ctrl Pts',(30.3926999167111,8.8985793893184,135.737132285728));
#41091=CARTESIAN_POINT('Ctrl Pts',(30.5516077161905,8.8999186210325,135.78649385511));
#41092=CARTESIAN_POINT('Ctrl Pts',(30.5717096993844,8.9,135.793075305549));
#41093=CARTESIAN_POINT('Ctrl Pts',(30.59160797831,8.9,135.8));
#41094=CARTESIAN_POINT('',(30.59160797831,8.9,135.8));
#41095=CARTESIAN_POINT('',(30.59160797831,8.9,135.8));
#41096=CARTESIAN_POINT('',(29.40839202169,8.9,135.8));
#41097=CARTESIAN_POINT('',(29.37557606376,8.99442305443429,135.70570254201));
#41098=CARTESIAN_POINT('Ctrl Pts',(29.40839202169,8.9,135.8));
#41099=CARTESIAN_POINT('Ctrl Pts',(29.4282903006156,8.9,135.793075305549));
#41100=CARTESIAN_POINT('Ctrl Pts',(29.4483897156904,8.89991869112576,135.786494096152));
#41101=CARTESIAN_POINT('Ctrl Pts',(29.6073267308058,8.89858282731955,135.737144184887));
#41102=CARTESIAN_POINT('Ctrl Pts',(29.8280063161928,8.89366846231917,135.699053886655));
#41103=CARTESIAN_POINT('Ctrl Pts',(30.1718975121812,8.89363063009448,135.698923164311));
#41104=CARTESIAN_POINT('Ctrl Pts',(30.3926999167111,8.8985793893184,135.737132285728));
#41105=CARTESIAN_POINT('Ctrl Pts',(30.5516077161905,8.8999186210325,135.78649385511));
#41106=CARTESIAN_POINT('Ctrl Pts',(30.5717096993844,8.9,135.793075305549));
#41107=CARTESIAN_POINT('Ctrl Pts',(30.59160797831,8.9,135.8));
#41108=CARTESIAN_POINT('Ctrl Pts',(29.1514718625761,9.,135.8));
#41109=CARTESIAN_POINT('Ctrl Pts',(29.2240383852933,9.,135.763779566847));
#41110=CARTESIAN_POINT('Ctrl Pts',(29.2989266202372,8.99756721057679,135.732190956222));
#41111=CARTESIAN_POINT('Ctrl Pts',(29.37557606376,8.99442305443429,135.70570254201));
#41112=CARTESIAN_POINT('Ctrl Pts',(29.1663583211274,8.96666666666667,135.829824561404));
#41113=CARTESIAN_POINT('Ctrl Pts',(29.2376517469549,8.96666666666667,135.794239574446));
#41114=CARTESIAN_POINT('Ctrl Pts',(29.3112262464824,8.96504480705119,135.763211800971));
#41115=CARTESIAN_POINT('Ctrl Pts',(29.3865147164034,8.96294870295619,135.737135028007));
#41116=CARTESIAN_POINT('Ctrl Pts',(29.1812447796787,8.93333333333333,135.859649122807));
#41117=CARTESIAN_POINT('Ctrl Pts',(29.2512651086164,8.93333333333333,135.824699582045));
#41118=CARTESIAN_POINT('Ctrl Pts',(29.3235258727276,8.9325224035256,135.79423264572));
#41119=CARTESIAN_POINT('Ctrl Pts',(29.3974533690467,8.9314743514781,135.768567514003));
#41120=CARTESIAN_POINT('Ctrl Pts',(29.19613123823,8.9,135.889473684211));
#41121=CARTESIAN_POINT('Ctrl Pts',(29.2648784702779,8.9,135.855159589644));
#41122=CARTESIAN_POINT('Ctrl Pts',(29.3358254989728,8.9,135.825253490469));
#41123=CARTESIAN_POINT('Ctrl Pts',(29.40839202169,8.9,135.8));
#41124=CARTESIAN_POINT('Ctrl Pts',(29.19613123823,8.9,135.889473684211));
#41125=CARTESIAN_POINT('Ctrl Pts',(29.2648784702779,8.9,135.855159589644));
#41126=CARTESIAN_POINT('Ctrl Pts',(29.3358254989728,8.9,135.825253490469));
#41127=CARTESIAN_POINT('Ctrl Pts',(29.40839202169,8.9,135.8));
#41128=CARTESIAN_POINT('Ctrl Pts',(30.62442393624,8.99442305443429,135.70570254201));
#41129=CARTESIAN_POINT('Ctrl Pts',(30.7010733797633,8.99756721057681,135.732190956222));
#41130=CARTESIAN_POINT('Ctrl Pts',(30.7759616147075,9.00000000000003,135.763779566847));
#41131=CARTESIAN_POINT('Ctrl Pts',(30.8485281374252,9.,135.800000000001));
#41132=CARTESIAN_POINT('Ctrl Pts',(30.6134852835967,8.96294870295619,135.737135028007));
#41133=CARTESIAN_POINT('Ctrl Pts',(30.6887737535181,8.96504480705121,135.763211800971));
#41134=CARTESIAN_POINT('Ctrl Pts',(30.762348253046,8.96666666666669,135.794239574446));
#41135=CARTESIAN_POINT('Ctrl Pts',(30.8336416788738,8.96666666666667,135.829824561404));
#41136=CARTESIAN_POINT('Ctrl Pts',(30.6025466309533,8.9314743514781,135.768567514003));
#41137=CARTESIAN_POINT('Ctrl Pts',(30.6764741272728,8.9325224035256,135.79423264572));
#41138=CARTESIAN_POINT('Ctrl Pts',(30.7487348913845,8.93333333333334,135.824699582045));
#41139=CARTESIAN_POINT('Ctrl Pts',(30.8187552203225,8.93333333333333,135.859649122808));
#41140=CARTESIAN_POINT('Ctrl Pts',(30.59160797831,8.9,135.8));
#41141=CARTESIAN_POINT('Ctrl Pts',(30.6641745010276,8.9,135.825253490469));
#41142=CARTESIAN_POINT('Ctrl Pts',(30.7351215297229,8.9,135.855159589645));
#41143=CARTESIAN_POINT('Ctrl Pts',(30.8038687617712,8.9,135.889473684211));
#41144=CARTESIAN_POINT('Ctrl Pts',(30.59160797831,8.9,135.8));
#41145=CARTESIAN_POINT('Ctrl Pts',(30.6641745010276,8.9,135.825253490469));
#41146=CARTESIAN_POINT('Ctrl Pts',(30.7351215297229,8.9,135.855159589645));
#41147=CARTESIAN_POINT('Ctrl Pts',(30.8038687617712,8.9,135.889473684211));
#41148=CARTESIAN_POINT('Origin',(30.,9.1,137.5));
#41149=CARTESIAN_POINT('',(28.2,8.5,137.5));
#41150=CARTESIAN_POINT('',(28.2,9.1,137.5));
#41151=CARTESIAN_POINT('',(28.8951880620293,8.5,136.078947368421));
#41152=CARTESIAN_POINT('Origin',(30.,8.5,137.5));
#41153=CARTESIAN_POINT('',(29.0050125628934,8.5,136.));
#41154=CARTESIAN_POINT('Ctrl Pts',(29.0050125628934,8.5,136.));
#41155=CARTESIAN_POINT('Ctrl Pts',(28.9674326867105,8.5,136.024927669793));
#41156=CARTESIAN_POINT('Ctrl Pts',(28.9307900499921,8.5,136.051268237865));
#41157=CARTESIAN_POINT('Ctrl Pts',(28.8951880620293,8.5,136.078947368421));
#41158=CARTESIAN_POINT('',(30.9949874371066,8.5,136.));
#41159=CARTESIAN_POINT('Ctrl Pts',(30.9949874371066,8.5,136.));
#41160=CARTESIAN_POINT('Ctrl Pts',(30.9864258065899,8.5,135.994320856796));
#41161=CARTESIAN_POINT('Ctrl Pts',(30.9778385803597,8.49988842326335,135.98872938726));
#41162=CARTESIAN_POINT('Ctrl Pts',(30.969224994042,8.49967132634843,135.983225754498));
#41163=CARTESIAN_POINT('Ctrl Pts',(30.9575122929155,8.49937611931315,135.975741948882));
#41164=CARTESIAN_POINT('Ctrl Pts',(30.9457713217168,8.49890678768928,135.968421934072));
#41165=CARTESIAN_POINT('Ctrl Pts',(30.9339557970041,8.49823106356219,135.961260087485));
#41166=CARTESIAN_POINT('Ctrl Pts',(30.672656166037,8.48328746441287,135.802876273328));
#41167=CARTESIAN_POINT('Ctrl Pts',(30.3954457405881,8.39151314723882,135.72337153152));
#41168=CARTESIAN_POINT('Ctrl Pts',(30.12651806476,8.36979419621021,135.704342425858));
#41169=CARTESIAN_POINT('Ctrl Pts',(30.1036961845309,8.36795107129735,135.702727568001));
#41170=CARTESIAN_POINT('Ctrl Pts',(30.0808655520404,8.36653921144899,135.701565046591));
#41171=CARTESIAN_POINT('Ctrl Pts',(30.0580358116452,8.3656616809124,135.700830713729));
#41172=CARTESIAN_POINT('Ctrl Pts',(30.047033558372,8.36523877583107,135.700476819378));
#41173=CARTESIAN_POINT('Ctrl Pts',(30.0360377469811,8.36493371946735,135.700224932826));
#41174=CARTESIAN_POINT('Ctrl Pts',(30.0250383816017,8.36475069000845,135.70007315735));
#41175=CARTESIAN_POINT('Ctrl Pts',(30.0034967468638,8.36439223716922,135.699775913669));
#41176=CARTESIAN_POINT('Ctrl Pts',(29.9819578260176,8.36450298023026,135.69986705092));
#41177=CARTESIAN_POINT('Ctrl Pts',(29.9604219380954,8.36507608574144,135.700340519536));
#41178=CARTESIAN_POINT('Ctrl Pts',(29.9360173607035,8.36572553181268,135.700877056574));
#41179=CARTESIAN_POINT('Ctrl Pts',(29.911581134165,8.36698783297317,135.701939651609));
#41180=CARTESIAN_POINT('Ctrl Pts',(29.8872393421969,8.36876645171126,135.703437238886));
#41181=CARTESIAN_POINT('Ctrl Pts',(29.6648767426176,8.38501415799279,135.717117718958));
#41182=CARTESIAN_POINT('Ctrl Pts',(29.4328429101899,8.45069979287912,135.774591014166));
#41183=CARTESIAN_POINT('Ctrl Pts',(29.2152684605821,8.48252846513542,135.880025058399));
#41184=CARTESIAN_POINT('Ctrl Pts',(29.1790060523141,8.48783324384481,135.897597399105));
#41185=CARTESIAN_POINT('Ctrl Pts',(29.1431452935689,8.49219755137002,135.916501982839));
#41186=CARTESIAN_POINT('Ctrl Pts',(29.1081615516992,8.49523924040882,135.936454666153));
#41187=CARTESIAN_POINT('Ctrl Pts',(29.0731778098294,8.49828092944762,135.956407349467));
#41188=CARTESIAN_POINT('Ctrl Pts',(29.0390710848352,8.5,135.977408132361));
#41189=CARTESIAN_POINT('Ctrl Pts',(29.0050125628934,8.5,136.));
#41190=CARTESIAN_POINT('',(31.1048119379707,8.5,136.078947368421));
#41191=CARTESIAN_POINT('Ctrl Pts',(31.1048119379707,8.5,136.078947368421));
#41192=CARTESIAN_POINT('Ctrl Pts',(31.0692099500079,8.5,136.051268237865));
#41193=CARTESIAN_POINT('Ctrl Pts',(31.0325673132895,8.5,136.024927669793));
#41194=CARTESIAN_POINT('Ctrl Pts',(30.9949874371066,8.5,136.));
#41195=CARTESIAN_POINT('Origin',(30.,8.5,137.5));
#41196=CARTESIAN_POINT('Ctrl Pts',(31.0500544632573,8.39129047171135,135.916983334517));
#41197=CARTESIAN_POINT('Ctrl Pts',(31.0416572725171,8.39013445090614,135.911534549944));
#41198=CARTESIAN_POINT('Ctrl Pts',(31.0332269292893,8.38887979850224,135.906181548932));
#41199=CARTESIAN_POINT('Ctrl Pts',(31.0132512017485,8.38570823783423,135.893775706518));
#41200=CARTESIAN_POINT('Ctrl Pts',(31.0017011490689,8.38371414702549,135.886801483368));
#41201=CARTESIAN_POINT('Ctrl Pts',(30.73243501588,8.33432174868635,135.729698539418));
#41202=CARTESIAN_POINT('Ctrl Pts',(30.4528075616641,8.21969538053694,135.663791800073));
#41203=CARTESIAN_POINT('Ctrl Pts',(30.1194544951314,8.18662675501976,135.646080977264));
#41204=CARTESIAN_POINT('Ctrl Pts',(30.0932684231087,8.18474888991971,135.645104148142));
#41205=CARTESIAN_POINT('Ctrl Pts',(30.0542637892422,8.18295722410468,135.644178995873));
#41206=CARTESIAN_POINT('Ctrl Pts',(30.0415691426709,8.18254082843928,135.643965691679));
#41207=CARTESIAN_POINT('Ctrl Pts',(30.0039648708177,8.18179778951162,135.64358472223));
#41208=CARTESIAN_POINT('Ctrl Pts',(29.9790422078338,8.18194773384953,135.643661590033));
#41209=CARTESIAN_POINT('Ctrl Pts',(29.9259892365849,8.18363575834559,135.644519987645));
#41210=CARTESIAN_POINT('Ctrl Pts',(29.8979097346567,8.18532290965731,135.645414992116));
#41211=CARTESIAN_POINT('Ctrl Pts',(29.6150612328207,8.21055133692172,135.658397917784));
#41212=CARTESIAN_POINT('Ctrl Pts',(29.3353440644627,8.30782885450725,135.714217769816));
#41213=CARTESIAN_POINT('Ctrl Pts',(29.0505321085055,8.3745011316311,135.855362112556));
#41214=CARTESIAN_POINT('Ctrl Pts',(28.9833499104208,8.38669177291416,135.895307843082));
#41215=CARTESIAN_POINT('Ctrl Pts',(28.9499455367427,8.39129047171135,135.916983334517));
#41216=CARTESIAN_POINT('Ctrl Pts',(31.0316987878737,8.4275269811409,135.944655556345));
#41217=CARTESIAN_POINT('Ctrl Pts',(31.0232496115585,8.42674793297165,135.939128693744));
#41218=CARTESIAN_POINT('Ctrl Pts',(31.0147601027094,8.42589417137142,135.933699269146));
#41219=CARTESIAN_POINT('Ctrl Pts',(30.9946782507695,8.42357762853484,135.921094749865));
#41220=CARTESIAN_POINT('Ctrl Pts',(30.9830484738135,8.42213322181795,135.914011559485));
#41221=CARTESIAN_POINT('Ctrl Pts',(30.7126277643191,8.3839211305528,135.754083580217));
#41222=CARTESIAN_POINT('Ctrl Pts',(30.4334575445295,8.27676192071996,135.683612800791));
#41223=CARTESIAN_POINT('Ctrl Pts',(30.11421209809,8.24716089858398,135.664984304196));
#41224=CARTESIAN_POINT('Ctrl Pts',(30.0891005771669,8.24535197239345,135.663930548954));
#41225=CARTESIAN_POINT('Ctrl Pts',(30.0518486109606,8.24377963463304,135.662960509384));
#41226=CARTESIAN_POINT('Ctrl Pts',(30.0397052276191,8.2433830423102,135.66273192281));
#41227=CARTESIAN_POINT('Ctrl Pts',(30.0038065076672,8.24270601822244,135.662326479773));
#41228=CARTESIAN_POINT('Ctrl Pts',(29.9799830207133,8.24285973044089,135.662414140564));
#41229=CARTESIAN_POINT('Ctrl Pts',(29.9293414259812,8.24435747176978,135.66331209502));
#41230=CARTESIAN_POINT('Ctrl Pts',(29.9024170132781,8.24595661414936,135.664279393149));
#41231=CARTESIAN_POINT('Ctrl Pts',(29.6318884637786,8.26858643327872,135.677933353777));
#41232=CARTESIAN_POINT('Ctrl Pts',(29.3549087480204,8.35906934575154,135.737533569262));
#41233=CARTESIAN_POINT('Ctrl Pts',(29.0694554505283,8.41521142211316,135.882050996154));
#41234=CARTESIAN_POINT('Ctrl Pts',(29.0019254602039,8.42441726441167,135.922670690471));
#41235=CARTESIAN_POINT('Ctrl Pts',(28.9683012121262,8.4275269811409,135.944655556345));
#41236=CARTESIAN_POINT('Ctrl Pts',(31.0133431124902,8.46376349057045,135.972327778172));
#41237=CARTESIAN_POINT('Ctrl Pts',(31.0048334675486,8.46338651793449,135.966726712996));
#41238=CARTESIAN_POINT('Ctrl Pts',(30.9963054069395,8.46287405039417,135.961211667046));
#41239=CARTESIAN_POINT('Ctrl Pts',(30.9760852438945,8.46150672861254,135.948422905536));
#41240=CARTESIAN_POINT('Ctrl Pts',(30.9644239969721,8.46048771289681,135.941211857955));
#41241=CARTESIAN_POINT('Ctrl Pts',(30.6924634175979,8.43368808254642,135.778491232529));
#41242=CARTESIAN_POINT('Ctrl Pts',(30.4147957577227,8.3344466070558,135.703550530802));
#41243=CARTESIAN_POINT('Ctrl Pts',(30.1089385815722,8.30741692773313,135.683824241069));
#41244=CARTESIAN_POINT('Ctrl Pts',(30.0850333979822,8.30593612897524,135.68273864578));
#41245=CARTESIAN_POINT('Ctrl Pts',(30.0494487366536,8.30441636530272,135.681695305867));
#41246=CARTESIAN_POINT('Ctrl Pts',(30.0379016620329,8.30409150559643,135.681458701694));
#41247=CARTESIAN_POINT('Ctrl Pts',(30.0036551100143,8.3034840084584,135.681034156126));
#41248=CARTESIAN_POINT('Ctrl Pts',(29.981017013138,8.3035909836389,135.681114500388));
#41249=CARTESIAN_POINT('Ctrl Pts',(29.9326651713072,8.30500381838849,135.682084949199));
#41250=CARTESIAN_POINT('Ctrl Pts',(29.9070738555437,8.30635412848112,135.683075250576));
#41251=CARTESIAN_POINT('Ctrl Pts',(29.6480495116597,8.32697906163579,135.697582282965));
#41252=CARTESIAN_POINT('Ctrl Pts',(29.3746059212276,8.41040690744922,135.760854097255));
#41253=CARTESIAN_POINT('Ctrl Pts',(29.0883611928009,8.45585156841319,135.908717682976));
#41254=CARTESIAN_POINT('Ctrl Pts',(29.020495535052,8.46227450850248,135.950045284972));
#41255=CARTESIAN_POINT('Ctrl Pts',(28.9866568875098,8.46376349057045,135.972327778172));
#41256=CARTESIAN_POINT('Ctrl Pts',(30.9949874371066,8.5,136.));
#41257=CARTESIAN_POINT('Ctrl Pts',(30.9864258065899,8.5,135.994320856796));
#41258=CARTESIAN_POINT('Ctrl Pts',(30.9778385803597,8.49988842326335,135.98872938726));
#41259=CARTESIAN_POINT('Ctrl Pts',(30.9575122929155,8.49937611931315,135.975741948882));
#41260=CARTESIAN_POINT('Ctrl Pts',(30.9457713217168,8.49890678768928,135.968421934072));
#41261=CARTESIAN_POINT('Ctrl Pts',(30.672656166037,8.48328746441287,135.802876273328));
#41262=CARTESIAN_POINT('Ctrl Pts',(30.3954457405881,8.39151314723882,135.72337153152));
#41263=CARTESIAN_POINT('Ctrl Pts',(30.1036961845309,8.36795107129735,135.702727568001));
#41264=CARTESIAN_POINT('Ctrl Pts',(30.0808655520404,8.36653921144899,135.701565046591));
#41265=CARTESIAN_POINT('Ctrl Pts',(30.047033558372,8.36523877583107,135.700476819378));
#41266=CARTESIAN_POINT('Ctrl Pts',(30.0360377469811,8.36493371946735,135.700224932826));
#41267=CARTESIAN_POINT('Ctrl Pts',(30.0034967468638,8.36439223716922,135.699775913669));
#41268=CARTESIAN_POINT('Ctrl Pts',(29.9819578260176,8.36450298023026,135.69986705092));
#41269=CARTESIAN_POINT('Ctrl Pts',(29.9360173607035,8.36572553181268,135.700877056574));
#41270=CARTESIAN_POINT('Ctrl Pts',(29.911581134165,8.36698783297317,135.701939651609));
#41271=CARTESIAN_POINT('Ctrl Pts',(29.6648767426176,8.38501415799279,135.717117718958));
#41272=CARTESIAN_POINT('Ctrl Pts',(29.3941706047853,8.46164739869351,135.784169896701));
#41273=CARTESIAN_POINT('Ctrl Pts',(29.1072845348237,8.49656185889524,135.935406566573));
#41274=CARTESIAN_POINT('Ctrl Pts',(29.0390710848352,8.5,135.977408132361));
#41275=CARTESIAN_POINT('Ctrl Pts',(29.0050125628934,8.5,136.));
#41276=CARTESIAN_POINT('',(31.0500544632573,8.39129047171135,135.916983334517));
#41277=CARTESIAN_POINT('',(29.0050125628934,8.5,136.));
#41278=CARTESIAN_POINT('Origin',(30.,8.45,137.5));
#41279=CARTESIAN_POINT('',(28.8338096210309,8.4,136.));
#41280=CARTESIAN_POINT('',(31.1048119379707,8.5,136.078947368421));
#41281=CARTESIAN_POINT('Ctrl Pts',(28.9499455367427,8.39129047171135,135.916983334517));
#41282=CARTESIAN_POINT('Ctrl Pts',(28.9100201948422,8.39678689632762,135.942890163806));
#41283=CARTESIAN_POINT('Ctrl Pts',(28.8713894960226,8.40000000009859,135.970783140825));
#41284=CARTESIAN_POINT('Ctrl Pts',(28.8338096192947,8.4,136.00000000135));
#41285=CARTESIAN_POINT('Ctrl Pts',(28.9683012121262,8.4275269811409,135.944655556345));
#41286=CARTESIAN_POINT('Ctrl Pts',(28.9291576919387,8.43119126421841,135.970235999263));
#41287=CARTESIAN_POINT('Ctrl Pts',(28.8911896803029,8.43333333339906,135.997611506775));
#41288=CARTESIAN_POINT('Ctrl Pts',(28.854269099658,8.43333333333333,136.0263157908));
#41289=CARTESIAN_POINT('Ctrl Pts',(28.9866568875098,8.46376349057045,135.972327778172));
#41290=CARTESIAN_POINT('Ctrl Pts',(28.9482951890352,8.46559563210921,135.99758183472));
#41291=CARTESIAN_POINT('Ctrl Pts',(28.9109898645832,8.46666666669953,136.024439872726));
#41292=CARTESIAN_POINT('Ctrl Pts',(28.8747285800212,8.46666666666667,136.05263158025));
#41293=CARTESIAN_POINT('Ctrl Pts',(29.0050125628934,8.5,136.));
#41294=CARTESIAN_POINT('Ctrl Pts',(28.9674326861317,8.5,136.024927670177));
#41295=CARTESIAN_POINT('Ctrl Pts',(28.9307900488635,8.5,136.051268238676));
#41296=CARTESIAN_POINT('Ctrl Pts',(28.8951880603845,8.5,136.0789473697));
#41297=CARTESIAN_POINT('Ctrl Pts',(31.166190378969,8.4,136.));
#41298=CARTESIAN_POINT('Ctrl Pts',(31.1286105027861,8.4,135.970783139968));
#41299=CARTESIAN_POINT('Ctrl Pts',(31.0899798045429,8.39678689624297,135.942890163407));
#41300=CARTESIAN_POINT('Ctrl Pts',(31.0500544632573,8.39129047171135,135.916983334517));
#41301=CARTESIAN_POINT('Ctrl Pts',(31.1457308986363,8.43333333333333,136.026315789474));
#41302=CARTESIAN_POINT('Ctrl Pts',(31.1088103185267,8.43333333333333,135.997611505934));
#41303=CARTESIAN_POINT('Ctrl Pts',(31.0708423074584,8.43119126416198,135.970235998869));
#41304=CARTESIAN_POINT('Ctrl Pts',(31.0316987878737,8.4275269811409,135.944655556345));
#41305=CARTESIAN_POINT('Ctrl Pts',(31.1252714183035,8.46666666666667,136.052631578947));
#41306=CARTESIAN_POINT('Ctrl Pts',(31.0890101342673,8.46666666666667,136.024439871899));
#41307=CARTESIAN_POINT('Ctrl Pts',(31.051704810374,8.46559563208099,135.997581834331));
#41308=CARTESIAN_POINT('Ctrl Pts',(31.0133431124902,8.46376349057045,135.972327778172));
#41309=CARTESIAN_POINT('Ctrl Pts',(31.1048119379707,8.5,136.078947368421));
#41310=CARTESIAN_POINT('Ctrl Pts',(31.0692099500079,8.5,136.051268237865));
#41311=CARTESIAN_POINT('Ctrl Pts',(31.0325673132895,8.5,136.024927669793));
#41312=CARTESIAN_POINT('Ctrl Pts',(30.9949874371066,8.5,136.));
#41313=CARTESIAN_POINT('Origin',(18.5,0.,134.05));
#41314=CARTESIAN_POINT('',(17.895,7.40911313484149E-17,134.));
#41315=CARTESIAN_POINT('Origin',(18.5,0.,134.));
#41316=CARTESIAN_POINT('',(17.995,-6.18446633569412E-17,134.1));
#41317=CARTESIAN_POINT('',(17.945,6.79678973526781E-17,134.05));
#41318=CARTESIAN_POINT('Origin',(18.5,0.,134.1));
#41319=CARTESIAN_POINT('Origin',(18.5,0.,134.));
#41320=CARTESIAN_POINT('',(17.995,6.18446633569412E-17,134.9));
#41321=CARTESIAN_POINT('',(17.995,-6.18446633569412E-17,134.));
#41322=CARTESIAN_POINT('Origin',(18.5,0.,134.9));
#41323=CARTESIAN_POINT('Origin',(0.,0.,134.));
#41324=CARTESIAN_POINT('',(-19.105,7.40911313484149E-17,134.));
#41325=CARTESIAN_POINT('Origin',(-18.5,0.,134.));
#41326=CARTESIAN_POINT('Origin',(18.5,0.,134.95));
#41327=CARTESIAN_POINT('',(17.895,-7.40911313484149E-17,135.));
#41328=CARTESIAN_POINT('Origin',(18.5,0.,135.));
#41329=CARTESIAN_POINT('',(17.945,-6.79678973526781E-17,134.95));
#41330=CARTESIAN_POINT('Origin',(0.,0.,135.));
#41331=CARTESIAN_POINT('',(-25.8,9.,135.));
#41332=CARTESIAN_POINT('',(-19.105,-7.40911313484149E-17,135.));
#41333=CARTESIAN_POINT('Origin',(-18.5,0.,135.));
#41334=CARTESIAN_POINT('Origin',(-18.5,0.,134.05));
#41335=CARTESIAN_POINT('',(-19.005,-6.18446633569412E-17,134.1));
#41336=CARTESIAN_POINT('',(-19.055,6.79678973526781E-17,134.05));
#41337=CARTESIAN_POINT('Origin',(-18.5,0.,134.1));
#41338=CARTESIAN_POINT('Origin',(-18.5,0.,134.));
#41339=CARTESIAN_POINT('',(-19.005,6.18446633569412E-17,134.9));
#41340=CARTESIAN_POINT('',(-19.005,-6.18446633569412E-17,134.));
#41341=CARTESIAN_POINT('Origin',(-18.5,0.,134.9));
#41342=CARTESIAN_POINT('Origin',(-18.5,0.,134.95));
#41343=CARTESIAN_POINT('',(-19.055,-6.79678973526781E-17,134.95));
#41344=CARTESIAN_POINT('Ctrl Pts',(5.24283818900585,-9.,140.915348529816));
#41345=CARTESIAN_POINT('Ctrl Pts',(5.24283818900585,-8.9,140.915348529816));
#41346=CARTESIAN_POINT('Ctrl Pts',(5.00361661612988,-9.,141.188950061798));
#41347=CARTESIAN_POINT('Ctrl Pts',(5.00361661612988,-8.9,141.188950061798));
#41348=CARTESIAN_POINT('Ctrl Pts',(4.59392957389355,-9.,141.188950061798));
#41349=CARTESIAN_POINT('Ctrl Pts',(4.59392957389355,-8.9,141.188950061798));
#41350=CARTESIAN_POINT('',(5.24283818900585,-9.,140.915348529816));
#41351=CARTESIAN_POINT('',(4.59392957389355,-9.,141.188950061798));
#41352=CARTESIAN_POINT('Ctrl Pts',(5.24283818900585,-9.,140.915348529816));
#41353=CARTESIAN_POINT('Ctrl Pts',(5.00361661612988,-9.,141.188950061798));
#41354=CARTESIAN_POINT('Ctrl Pts',(4.59392957389355,-9.,141.188950061798));
#41355=CARTESIAN_POINT('',(5.24283818900585,-8.9,140.915348529816));
#41356=CARTESIAN_POINT('',(5.24283818900585,-9.,140.915348529816));
#41357=CARTESIAN_POINT('',(4.59392957389355,-8.9,141.188950061798));
#41358=CARTESIAN_POINT('Ctrl Pts',(5.24283818900585,-8.9,140.915348529816));
#41359=CARTESIAN_POINT('Ctrl Pts',(5.00361661612988,-8.9,141.188950061798));
#41360=CARTESIAN_POINT('Ctrl Pts',(4.59392957389355,-8.9,141.188950061798));
#41361=CARTESIAN_POINT('',(4.59392957389355,-9.,141.188950061798));
#41362=CARTESIAN_POINT('Ctrl Pts',(5.48205976188183,-9.,140.048704624176));
#41363=CARTESIAN_POINT('Ctrl Pts',(5.48205976188183,-8.9,140.048704624176));
#41364=CARTESIAN_POINT('Ctrl Pts',(5.48205976188183,-9.,140.641746997833));
#41365=CARTESIAN_POINT('Ctrl Pts',(5.48205976188183,-8.9,140.641746997833));
#41366=CARTESIAN_POINT('Ctrl Pts',(5.24283818900585,-9.,140.915348529816));
#41367=CARTESIAN_POINT('Ctrl Pts',(5.24283818900585,-8.9,140.915348529816));
#41368=CARTESIAN_POINT('',(5.48205976188183,-9.,140.048704624176));
#41369=CARTESIAN_POINT('Ctrl Pts',(5.48205976188183,-9.,140.048704624176));
#41370=CARTESIAN_POINT('Ctrl Pts',(5.48205976188183,-9.,140.641746997833));
#41371=CARTESIAN_POINT('Ctrl Pts',(5.24283818900585,-9.,140.915348529816));
#41372=CARTESIAN_POINT('',(5.48205976188183,-8.9,140.048704624176));
#41373=CARTESIAN_POINT('',(5.48205976188183,-9.,140.048704624176));
#41374=CARTESIAN_POINT('Ctrl Pts',(5.48205976188183,-8.9,140.048704624176));
#41375=CARTESIAN_POINT('Ctrl Pts',(5.48205976188183,-8.9,140.641746997833));
#41376=CARTESIAN_POINT('Ctrl Pts',(5.24283818900585,-8.9,140.915348529816));
#41377=CARTESIAN_POINT('Ctrl Pts',(5.25286512076855,-9.,139.071760654449));
#41378=CARTESIAN_POINT('Ctrl Pts',(5.25286512076855,-8.9,139.071760654449));
#41379=CARTESIAN_POINT('Ctrl Pts',(5.48205976188183,-9.,139.343929767609));
#41380=CARTESIAN_POINT('Ctrl Pts',(5.48205976188183,-8.9,139.343929767609));
#41381=CARTESIAN_POINT('Ctrl Pts',(5.48205976188183,-9.,140.048704624176));
#41382=CARTESIAN_POINT('Ctrl Pts',(5.48205976188183,-8.9,140.048704624176));
#41383=CARTESIAN_POINT('',(5.25286512076855,-9.,139.071760654449));
#41384=CARTESIAN_POINT('Ctrl Pts',(5.25286512076855,-9.,139.071760654449));
#41385=CARTESIAN_POINT('Ctrl Pts',(5.48205976188183,-9.,139.343929767609));
#41386=CARTESIAN_POINT('Ctrl Pts',(5.48205976188183,-9.,140.048704624176));
#41387=CARTESIAN_POINT('',(5.25286512076855,-8.9,139.071760654449));
#41388=CARTESIAN_POINT('',(5.25286512076855,-9.,139.071760654449));
#41389=CARTESIAN_POINT('Ctrl Pts',(5.25286512076855,-8.9,139.071760654449));
#41390=CARTESIAN_POINT('Ctrl Pts',(5.48205976188183,-8.9,139.343929767609));
#41391=CARTESIAN_POINT('Ctrl Pts',(5.48205976188183,-8.9,140.048704624176));
#41392=CARTESIAN_POINT('Ctrl Pts',(4.60538892447948,-9.,138.79959154129));
#41393=CARTESIAN_POINT('Ctrl Pts',(4.60538892447948,-8.9,138.79959154129));
#41394=CARTESIAN_POINT('Ctrl Pts',(5.02367047965527,-9.,138.79959154129));
#41395=CARTESIAN_POINT('Ctrl Pts',(5.02367047965527,-8.9,138.79959154129));
#41396=CARTESIAN_POINT('Ctrl Pts',(5.25286512076855,-9.,139.071760654449));
#41397=CARTESIAN_POINT('Ctrl Pts',(5.25286512076855,-8.9,139.071760654449));
#41398=CARTESIAN_POINT('',(4.60538892447948,-9.,138.79959154129));
#41399=CARTESIAN_POINT('Ctrl Pts',(4.60538892447948,-9.,138.79959154129));
#41400=CARTESIAN_POINT('Ctrl Pts',(5.02367047965527,-9.,138.79959154129));
#41401=CARTESIAN_POINT('Ctrl Pts',(5.25286512076855,-9.,139.071760654449));
#41402=CARTESIAN_POINT('',(4.60538892447948,-8.9,138.79959154129));
#41403=CARTESIAN_POINT('',(4.60538892447948,-9.,138.79959154129));
#41404=CARTESIAN_POINT('Ctrl Pts',(4.60538892447948,-8.9,138.79959154129));
#41405=CARTESIAN_POINT('Ctrl Pts',(5.02367047965527,-8.9,138.79959154129));
#41406=CARTESIAN_POINT('Ctrl Pts',(5.25286512076855,-8.9,139.071760654449));
#41407=CARTESIAN_POINT('Ctrl Pts',(3.96220998466015,-9.,139.077490329742));
#41408=CARTESIAN_POINT('Ctrl Pts',(3.96220998466015,-8.9,139.077490329742));
#41409=CARTESIAN_POINT('Ctrl Pts',(4.19856862723827,-9.,138.79959154129));
#41410=CARTESIAN_POINT('Ctrl Pts',(4.19856862723827,-8.9,138.79959154129));
#41411=CARTESIAN_POINT('Ctrl Pts',(4.60538892447948,-9.,138.79959154129));
#41412=CARTESIAN_POINT('Ctrl Pts',(4.60538892447948,-8.9,138.79959154129));
#41413=CARTESIAN_POINT('',(3.96220998466015,-9.,139.077490329742));
#41414=CARTESIAN_POINT('Ctrl Pts',(3.96220998466015,-9.,139.077490329742));
#41415=CARTESIAN_POINT('Ctrl Pts',(4.19856862723827,-9.,138.79959154129));
#41416=CARTESIAN_POINT('Ctrl Pts',(4.60538892447948,-9.,138.79959154129));
#41417=CARTESIAN_POINT('',(3.96220998466015,-8.9,139.077490329742));
#41418=CARTESIAN_POINT('',(3.96220998466015,-9.,139.077490329742));
#41419=CARTESIAN_POINT('Ctrl Pts',(3.96220998466015,-8.9,139.077490329742));
#41420=CARTESIAN_POINT('Ctrl Pts',(4.19856862723827,-8.9,138.79959154129));
#41421=CARTESIAN_POINT('Ctrl Pts',(4.60538892447948,-8.9,138.79959154129));
#41422=CARTESIAN_POINT('Ctrl Pts',(3.72585324943066,-9.,139.991405963898));
#41423=CARTESIAN_POINT('Ctrl Pts',(3.72585324943066,-8.9,139.991405963898));
#41424=CARTESIAN_POINT('Ctrl Pts',(3.72585324943066,-9.,139.355389595032));
#41425=CARTESIAN_POINT('Ctrl Pts',(3.72585324943066,-8.9,139.355389595032));
#41426=CARTESIAN_POINT('Ctrl Pts',(3.96220998466015,-9.,139.077490329742));
#41427=CARTESIAN_POINT('Ctrl Pts',(3.96220998466015,-8.9,139.077490329742));
#41428=CARTESIAN_POINT('',(3.72585324943066,-9.,139.991405963898));
#41429=CARTESIAN_POINT('Ctrl Pts',(3.72585324943066,-9.,139.991405963898));
#41430=CARTESIAN_POINT('Ctrl Pts',(3.72585324943066,-9.,139.355389595032));
#41431=CARTESIAN_POINT('Ctrl Pts',(3.96220998466015,-9.,139.077490329742));
#41432=CARTESIAN_POINT('',(3.72585324943066,-8.9,139.991405963898));
#41433=CARTESIAN_POINT('',(3.72585324943066,-9.,139.991405963898));
#41434=CARTESIAN_POINT('Ctrl Pts',(3.72585324943066,-8.9,139.991405963898));
#41435=CARTESIAN_POINT('Ctrl Pts',(3.72585324943066,-8.9,139.355389595032));
#41436=CARTESIAN_POINT('Ctrl Pts',(3.96220998466015,-8.9,139.077490329742));
#41437=CARTESIAN_POINT('Ctrl Pts',(3.96364431083202,-9.,140.911051273346));
#41438=CARTESIAN_POINT('Ctrl Pts',(3.96364431083202,-8.9,140.911051273346));
#41439=CARTESIAN_POINT('Ctrl Pts',(3.72585324943066,-9.,140.633152008057));
#41440=CARTESIAN_POINT('Ctrl Pts',(3.72585324943066,-8.9,140.633152008057));
#41441=CARTESIAN_POINT('Ctrl Pts',(3.72585324943066,-9.,139.991405963898));
#41442=CARTESIAN_POINT('Ctrl Pts',(3.72585324943066,-8.9,139.991405963898));
#41443=CARTESIAN_POINT('',(3.96364431083202,-9.,140.911051273346));
#41444=CARTESIAN_POINT('Ctrl Pts',(3.96364431083202,-9.,140.911051273346));
#41445=CARTESIAN_POINT('Ctrl Pts',(3.72585324943066,-9.,140.633152008057));
#41446=CARTESIAN_POINT('Ctrl Pts',(3.72585324943066,-9.,139.991405963898));
#41447=CARTESIAN_POINT('',(3.96364431083202,-8.9,140.911051273346));
#41448=CARTESIAN_POINT('',(3.96364431083202,-9.,140.911051273346));
#41449=CARTESIAN_POINT('Ctrl Pts',(3.96364431083202,-8.9,140.911051273346));
#41450=CARTESIAN_POINT('Ctrl Pts',(3.72585324943066,-8.9,140.633152008057));
#41451=CARTESIAN_POINT('Ctrl Pts',(3.72585324943066,-8.9,139.991405963898));
#41452=CARTESIAN_POINT('Ctrl Pts',(4.59392957389355,-9.,141.188950061798));
#41453=CARTESIAN_POINT('Ctrl Pts',(4.59392957389355,-8.9,141.188950061798));
#41454=CARTESIAN_POINT('Ctrl Pts',(4.20143346488476,-9.,141.188950061798));
#41455=CARTESIAN_POINT('Ctrl Pts',(4.20143346488476,-8.9,141.188950061798));
#41456=CARTESIAN_POINT('Ctrl Pts',(3.96364431083202,-9.,140.911051273346));
#41457=CARTESIAN_POINT('Ctrl Pts',(3.96364431083202,-8.9,140.911051273346));
#41458=CARTESIAN_POINT('Ctrl Pts',(4.59392957389355,-9.,141.188950061798));
#41459=CARTESIAN_POINT('Ctrl Pts',(4.20143346488476,-9.,141.188950061798));
#41460=CARTESIAN_POINT('Ctrl Pts',(3.96364431083202,-9.,140.911051273346));
#41461=CARTESIAN_POINT('Ctrl Pts',(4.59392957389355,-8.9,141.188950061798));
#41462=CARTESIAN_POINT('Ctrl Pts',(4.20143346488476,-8.9,141.188950061798));
#41463=CARTESIAN_POINT('Ctrl Pts',(3.96364431083202,-8.9,140.911051273346));
#41464=CARTESIAN_POINT('Ctrl Pts',(3.47230558097363,-9.,138.054707050323));
#41465=CARTESIAN_POINT('Ctrl Pts',(3.47230558097363,-8.9,138.054707050323));
#41466=CARTESIAN_POINT('Ctrl Pts',(3.00675420463085,-9.,138.281037330627));
#41467=CARTESIAN_POINT('Ctrl Pts',(3.00675420463085,-8.9,138.281037330627));
#41468=CARTESIAN_POINT('Ctrl Pts',(2.71739415824413,-9.,138.770942211151));
#41469=CARTESIAN_POINT('Ctrl Pts',(2.71739415824413,-8.9,138.770942211151));
#41470=CARTESIAN_POINT('',(3.47230558097363,-8.9,138.054707050323));
#41471=CARTESIAN_POINT('',(3.47230558097363,-9.,138.054707050323));
#41472=CARTESIAN_POINT('',(2.71739415824413,-8.9,138.770942211151));
#41473=CARTESIAN_POINT('Ctrl Pts',(3.47230558097363,-8.9,138.054707050323));
#41474=CARTESIAN_POINT('Ctrl Pts',(3.00675420463085,-8.9,138.281037330627));
#41475=CARTESIAN_POINT('Ctrl Pts',(2.71739415824413,-8.9,138.770942211151));
#41476=CARTESIAN_POINT('',(2.71739415824413,-9.,138.770942211151));
#41477=CARTESIAN_POINT('Ctrl Pts',(4.64836339652538,-9.,137.828377246857));
#41478=CARTESIAN_POINT('Ctrl Pts',(4.64836339652538,-8.9,137.828377246857));
#41479=CARTESIAN_POINT('Ctrl Pts',(3.93785886466503,-9.,137.828377246857));
#41480=CARTESIAN_POINT('Ctrl Pts',(3.93785886466503,-8.9,137.828377246857));
#41481=CARTESIAN_POINT('Ctrl Pts',(3.47230558097363,-9.,138.054707050323));
#41482=CARTESIAN_POINT('Ctrl Pts',(3.47230558097363,-8.9,138.054707050323));
#41483=CARTESIAN_POINT('',(4.64836339652538,-8.9,137.828377246857));
#41484=CARTESIAN_POINT('',(4.64836339652538,-9.,137.828377246857));
#41485=CARTESIAN_POINT('Ctrl Pts',(4.64836339652538,-8.9,137.828377246857));
#41486=CARTESIAN_POINT('Ctrl Pts',(3.93785886466503,-8.9,137.828377246857));
#41487=CARTESIAN_POINT('Ctrl Pts',(3.47230558097363,-8.9,138.054707050323));
#41488=CARTESIAN_POINT('Ctrl Pts',(5.81582669913769,-9.,138.090518951416));
#41489=CARTESIAN_POINT('Ctrl Pts',(5.81582669913769,-8.9,138.090518951416));
#41490=CARTESIAN_POINT('Ctrl Pts',(5.3474085777998,-9.,137.828377246857));
#41491=CARTESIAN_POINT('Ctrl Pts',(5.3474085777998,-8.9,137.828377246857));
#41492=CARTESIAN_POINT('Ctrl Pts',(4.64836339652538,-9.,137.828377246857));
#41493=CARTESIAN_POINT('Ctrl Pts',(4.64836339652538,-8.9,137.828377246857));
#41494=CARTESIAN_POINT('',(5.81582669913769,-8.9,138.090518951416));
#41495=CARTESIAN_POINT('',(5.81582669913769,-9.,138.090518951416));
#41496=CARTESIAN_POINT('Ctrl Pts',(5.81582669913769,-8.9,138.090518951416));
#41497=CARTESIAN_POINT('Ctrl Pts',(5.3474085777998,-8.9,137.828377246857));
#41498=CARTESIAN_POINT('Ctrl Pts',(4.64836339652538,-8.9,137.828377246857));
#41499=CARTESIAN_POINT('Ctrl Pts',(6.53206090629101,-9.,138.823943138123));
#41500=CARTESIAN_POINT('Ctrl Pts',(6.53206090629101,-8.9,138.823943138123));
#41501=CARTESIAN_POINT('Ctrl Pts',(6.28424291312695,-9.,138.352660655975));
#41502=CARTESIAN_POINT('Ctrl Pts',(6.28424291312695,-8.9,138.352660655975));
#41503=CARTESIAN_POINT('Ctrl Pts',(5.81582669913769,-9.,138.090518951416));
#41504=CARTESIAN_POINT('Ctrl Pts',(5.81582669913769,-8.9,138.090518951416));
#41505=CARTESIAN_POINT('',(6.53206090629101,-8.9,138.823943138123));
#41506=CARTESIAN_POINT('',(6.53206090629101,-9.,138.823943138123));
#41507=CARTESIAN_POINT('Ctrl Pts',(6.53206090629101,-8.9,138.823943138123));
#41508=CARTESIAN_POINT('Ctrl Pts',(6.28424291312695,-8.9,138.352660655975));
#41509=CARTESIAN_POINT('Ctrl Pts',(5.81582669913769,-8.9,138.090518951416));
#41510=CARTESIAN_POINT('Ctrl Pts',(6.77987699210644,-9.,140.031514644623));
#41511=CARTESIAN_POINT('Ctrl Pts',(6.77987699210644,-8.9,140.031514644623));
#41512=CARTESIAN_POINT('Ctrl Pts',(6.77987699210644,-9.,139.29522562027));
#41513=CARTESIAN_POINT('Ctrl Pts',(6.77987699210644,-8.9,139.29522562027));
#41514=CARTESIAN_POINT('Ctrl Pts',(6.53206090629101,-9.,138.823943138123));
#41515=CARTESIAN_POINT('Ctrl Pts',(6.53206090629101,-8.9,138.823943138123));
#41516=CARTESIAN_POINT('',(6.77987699210644,-8.9,140.031514644623));
#41517=CARTESIAN_POINT('',(6.77987699210644,-9.,140.031514644623));
#41518=CARTESIAN_POINT('Ctrl Pts',(6.77987699210644,-8.9,140.031514644623));
#41519=CARTESIAN_POINT('Ctrl Pts',(6.77987699210644,-8.9,139.29522562027));
#41520=CARTESIAN_POINT('Ctrl Pts',(6.53206090629101,-8.9,138.823943138123));
#41521=CARTESIAN_POINT('Ctrl Pts',(6.2126200646162,-9.,141.60866355896));
#41522=CARTESIAN_POINT('Ctrl Pts',(6.2126200646162,-8.9,141.60866355896));
#41523=CARTESIAN_POINT('Ctrl Pts',(6.77987699210644,-9.,141.045703411102));
#41524=CARTESIAN_POINT('Ctrl Pts',(6.77987699210644,-8.9,141.045703411102));
#41525=CARTESIAN_POINT('Ctrl Pts',(6.77987699210644,-9.,140.031514644623));
#41526=CARTESIAN_POINT('Ctrl Pts',(6.77987699210644,-8.9,140.031514644623));
#41527=CARTESIAN_POINT('',(6.2126200646162,-8.9,141.60866355896));
#41528=CARTESIAN_POINT('',(6.2126200646162,-9.,141.60866355896));
#41529=CARTESIAN_POINT('Ctrl Pts',(6.2126200646162,-8.9,141.60866355896));
#41530=CARTESIAN_POINT('Ctrl Pts',(6.77987699210644,-8.9,141.045703411102));
#41531=CARTESIAN_POINT('Ctrl Pts',(6.77987699210644,-8.9,140.031514644623));
#41532=CARTESIAN_POINT('Ctrl Pts',(4.59679441154003,-9.,142.171624183655));
#41533=CARTESIAN_POINT('Ctrl Pts',(4.59679441154003,-8.9,142.171624183655));
#41534=CARTESIAN_POINT('Ctrl Pts',(5.64536122977734,-9.,142.171624183655));
#41535=CARTESIAN_POINT('Ctrl Pts',(5.64536122977734,-8.9,142.171624183655));
#41536=CARTESIAN_POINT('Ctrl Pts',(6.2126200646162,-9.,141.60866355896));
#41537=CARTESIAN_POINT('Ctrl Pts',(6.2126200646162,-8.9,141.60866355896));
#41538=CARTESIAN_POINT('',(4.59679441154003,-8.9,142.171624183655));
#41539=CARTESIAN_POINT('',(4.59679441154003,-9.,142.171624183655));
#41540=CARTESIAN_POINT('Ctrl Pts',(4.59679441154003,-8.9,142.171624183655));
#41541=CARTESIAN_POINT('Ctrl Pts',(5.64536122977734,-8.9,142.171624183655));
#41542=CARTESIAN_POINT('Ctrl Pts',(6.2126200646162,-8.9,141.60866355896));
#41543=CARTESIAN_POINT('Ctrl Pts',(3.00102452933788,-9.,141.598636388779));
#41544=CARTESIAN_POINT('Ctrl Pts',(3.00102452933788,-8.9,141.598636388779));
#41545=CARTESIAN_POINT('Ctrl Pts',(3.57401113212109,-9.,142.171624183655));
#41546=CARTESIAN_POINT('Ctrl Pts',(3.57401113212109,-8.9,142.171624183655));
#41547=CARTESIAN_POINT('Ctrl Pts',(4.59679441154003,-9.,142.171624183655));
#41548=CARTESIAN_POINT('Ctrl Pts',(4.59679441154003,-8.9,142.171624183655));
#41549=CARTESIAN_POINT('',(3.00102452933788,-8.9,141.598636388779));
#41550=CARTESIAN_POINT('',(3.00102452933788,-9.,141.598636388779));
#41551=CARTESIAN_POINT('Ctrl Pts',(3.00102452933788,-8.9,141.598636388779));
#41552=CARTESIAN_POINT('Ctrl Pts',(3.57401113212109,-8.9,142.171624183655));
#41553=CARTESIAN_POINT('Ctrl Pts',(4.59679441154003,-8.9,142.171624183655));
#41554=CARTESIAN_POINT('Ctrl Pts',(2.42803601920605,-9.,139.997135639191));
#41555=CARTESIAN_POINT('Ctrl Pts',(2.42803601920605,-8.9,139.997135639191));
#41556=CARTESIAN_POINT('Ctrl Pts',(2.42803601920605,-9.,141.025648593903));
#41557=CARTESIAN_POINT('Ctrl Pts',(2.42803601920605,-8.9,141.025648593903));
#41558=CARTESIAN_POINT('Ctrl Pts',(3.00102452933788,-9.,141.598636388779));
#41559=CARTESIAN_POINT('Ctrl Pts',(3.00102452933788,-8.9,141.598636388779));
#41560=CARTESIAN_POINT('',(2.42803601920605,-8.9,139.997135639191));
#41561=CARTESIAN_POINT('',(2.42803601920605,-9.,139.997135639191));
#41562=CARTESIAN_POINT('Ctrl Pts',(2.42803601920605,-8.9,139.997135639191));
#41563=CARTESIAN_POINT('Ctrl Pts',(2.42803601920605,-8.9,141.025648593903));
#41564=CARTESIAN_POINT('Ctrl Pts',(3.00102452933788,-8.9,141.598636388779));
#41565=CARTESIAN_POINT('Ctrl Pts',(2.71739415824413,-9.,138.770942211151));
#41566=CARTESIAN_POINT('Ctrl Pts',(2.71739415824413,-8.9,138.770942211151));
#41567=CARTESIAN_POINT('Ctrl Pts',(2.42803601920605,-9.,139.260846614838));
#41568=CARTESIAN_POINT('Ctrl Pts',(2.42803601920605,-8.9,139.260846614838));
#41569=CARTESIAN_POINT('Ctrl Pts',(2.42803601920605,-9.,139.997135639191));
#41570=CARTESIAN_POINT('Ctrl Pts',(2.42803601920605,-8.9,139.997135639191));
#41571=CARTESIAN_POINT('Ctrl Pts',(2.71739415824413,-8.9,138.770942211151));
#41572=CARTESIAN_POINT('Ctrl Pts',(2.42803601920605,-8.9,139.260846614838));
#41573=CARTESIAN_POINT('Ctrl Pts',(2.42803601920605,-8.9,139.997135639191));
#41574=CARTESIAN_POINT('Origin',(4.60395650565624,-8.9,140.000000715256));
#41575=CARTESIAN_POINT('Origin',(-0.41684789955616,-9.,141.062892436981));
#41576=CARTESIAN_POINT('',(-0.41684789955616,-8.9,141.062892436981));
#41577=CARTESIAN_POINT('',(-0.41684789955616,-9.,141.062892436981));
#41578=CARTESIAN_POINT('',(-1.74044962227345,-8.9,141.062892436981));
#41579=CARTESIAN_POINT('',(-0.41684789955616,-8.9,141.062892436981));
#41580=CARTESIAN_POINT('',(-1.74044962227345,-9.,141.062892436981));
#41581=CARTESIAN_POINT('Origin',(-0.41684789955616,-9.,137.900000572205));
#41582=CARTESIAN_POINT('',(-0.41684789955616,-8.9,137.900000572205));
#41583=CARTESIAN_POINT('',(-0.41684789955616,-9.,137.900000572205));
#41584=CARTESIAN_POINT('',(-0.41684789955616,-8.9,137.900000572205));
#41585=CARTESIAN_POINT('Origin',(0.880968376994133,-9.,137.900000572205));
#41586=CARTESIAN_POINT('',(0.880968376994133,-8.9,137.900000572205));
#41587=CARTESIAN_POINT('',(0.880968376994133,-9.,137.900000572205));
#41588=CARTESIAN_POINT('',(0.880968376994133,-8.9,137.900000572205));
#41589=CARTESIAN_POINT('Origin',(0.880968376994133,-9.,141.062892436981));
#41590=CARTESIAN_POINT('',(0.880968376994133,-8.9,141.062892436981));
#41591=CARTESIAN_POINT('',(0.880968376994133,-9.,141.062892436981));
#41592=CARTESIAN_POINT('',(0.880968376994133,-8.9,141.062892436981));
#41593=CARTESIAN_POINT('Origin',(2.20457105338573,-9.,141.062892436981));
#41594=CARTESIAN_POINT('',(2.20457105338573,-8.9,141.062892436981));
#41595=CARTESIAN_POINT('',(2.20457105338573,-9.,141.062892436981));
#41596=CARTESIAN_POINT('',(2.20457105338573,-8.9,141.062892436981));
#41597=CARTESIAN_POINT('Origin',(2.20457105338573,-9.,142.10000038147));
#41598=CARTESIAN_POINT('',(2.20457105338573,-8.9,142.10000038147));
#41599=CARTESIAN_POINT('',(2.20457105338573,-9.,142.10000038147));
#41600=CARTESIAN_POINT('',(2.20457105338573,-8.9,142.10000038147));
#41601=CARTESIAN_POINT('Origin',(-1.74044962227345,-9.,142.10000038147));
#41602=CARTESIAN_POINT('',(-1.74044962227345,-8.9,142.10000038147));
#41603=CARTESIAN_POINT('',(-1.74044962227345,-9.,142.10000038147));
#41604=CARTESIAN_POINT('',(-1.74044962227345,-8.9,142.10000038147));
#41605=CARTESIAN_POINT('Origin',(-1.74044962227345,-9.,141.062892436981));
#41606=CARTESIAN_POINT('',(-1.74044962227345,-8.9,141.062892436981));
#41607=CARTESIAN_POINT('Origin',(0.232060715556145,-8.9,140.000000476837));
#41608=CARTESIAN_POINT('Ctrl Pts',(-5.37462396919727,-9.,141.10729932785));
#41609=CARTESIAN_POINT('Ctrl Pts',(-5.37462396919727,-8.9,141.10729932785));
#41610=CARTESIAN_POINT('Ctrl Pts',(-5.51643820106983,-9.,141.395225763321));
#41611=CARTESIAN_POINT('Ctrl Pts',(-5.51643820106983,-8.9,141.395225763321));
#41612=CARTESIAN_POINT('Ctrl Pts',(-5.80006761848927,-9.,141.395225763321));
#41613=CARTESIAN_POINT('Ctrl Pts',(-5.80006761848927,-8.9,141.395225763321));
#41614=CARTESIAN_POINT('',(-5.37462396919727,-9.,141.10729932785));
#41615=CARTESIAN_POINT('',(-5.80006761848927,-9.,141.395225763321));
#41616=CARTESIAN_POINT('Ctrl Pts',(-5.37462396919727,-9.,141.10729932785));
#41617=CARTESIAN_POINT('Ctrl Pts',(-5.51643820106983,-9.,141.395225763321));
#41618=CARTESIAN_POINT('Ctrl Pts',(-5.80006761848927,-9.,141.395225763321));
#41619=CARTESIAN_POINT('',(-5.37462396919727,-8.9,141.10729932785));
#41620=CARTESIAN_POINT('',(-5.37462396919727,-9.,141.10729932785));
#41621=CARTESIAN_POINT('',(-5.80006761848927,-8.9,141.395225763321));
#41622=CARTESIAN_POINT('Ctrl Pts',(-5.37462396919727,-8.9,141.10729932785));
#41623=CARTESIAN_POINT('Ctrl Pts',(-5.51643820106983,-8.9,141.395225763321));
#41624=CARTESIAN_POINT('Ctrl Pts',(-5.80006761848927,-8.9,141.395225763321));
#41625=CARTESIAN_POINT('',(-5.80006761848927,-9.,141.395225763321));
#41626=CARTESIAN_POINT('Ctrl Pts',(-5.23280973732471,-9.,139.982810974121));
#41627=CARTESIAN_POINT('Ctrl Pts',(-5.23280973732471,-8.9,139.982810974121));
#41628=CARTESIAN_POINT('Ctrl Pts',(-5.23280973732471,-9.,140.819372653961));
#41629=CARTESIAN_POINT('Ctrl Pts',(-5.23280973732471,-8.9,140.819372653961));
#41630=CARTESIAN_POINT('Ctrl Pts',(-5.37462396919727,-9.,141.10729932785));
#41631=CARTESIAN_POINT('Ctrl Pts',(-5.37462396919727,-8.9,141.10729932785));
#41632=CARTESIAN_POINT('',(-5.23280973732471,-9.,139.982810974121));
#41633=CARTESIAN_POINT('Ctrl Pts',(-5.23280973732471,-9.,139.982810974121));
#41634=CARTESIAN_POINT('Ctrl Pts',(-5.23280973732471,-9.,140.819372653961));
#41635=CARTESIAN_POINT('Ctrl Pts',(-5.37462396919727,-9.,141.10729932785));
#41636=CARTESIAN_POINT('',(-5.23280973732471,-8.9,139.982810974121));
#41637=CARTESIAN_POINT('',(-5.23280973732471,-9.,139.982810974121));
#41638=CARTESIAN_POINT('Ctrl Pts',(-5.23280973732471,-8.9,139.982810974121));
#41639=CARTESIAN_POINT('Ctrl Pts',(-5.23280973732471,-8.9,140.819372653961));
#41640=CARTESIAN_POINT('Ctrl Pts',(-5.37462396919727,-8.9,141.10729932785));
#41641=CARTESIAN_POINT('Ctrl Pts',(-5.29440565407276,-9.,139.143383979797));
#41642=CARTESIAN_POINT('Ctrl Pts',(-5.29440565407276,-8.9,139.143383979797));
#41643=CARTESIAN_POINT('Ctrl Pts',(-5.23280973732471,-9.,139.41268825531));
#41644=CARTESIAN_POINT('Ctrl Pts',(-5.23280973732471,-8.9,139.41268825531));
#41645=CARTESIAN_POINT('Ctrl Pts',(-5.23280973732471,-9.,139.982810974121));
#41646=CARTESIAN_POINT('Ctrl Pts',(-5.23280973732471,-8.9,139.982810974121));
#41647=CARTESIAN_POINT('',(-5.29440565407276,-9.,139.143383979797));
#41648=CARTESIAN_POINT('Ctrl Pts',(-5.29440565407276,-9.,139.143383979797));
#41649=CARTESIAN_POINT('Ctrl Pts',(-5.23280973732471,-9.,139.41268825531));
#41650=CARTESIAN_POINT('Ctrl Pts',(-5.23280973732471,-9.,139.982810974121));
#41651=CARTESIAN_POINT('',(-5.29440565407276,-8.9,139.143383979797));
#41652=CARTESIAN_POINT('',(-5.29440565407276,-9.,139.143383979797));
#41653=CARTESIAN_POINT('Ctrl Pts',(-5.29440565407276,-8.9,139.143383979797));
#41654=CARTESIAN_POINT('Ctrl Pts',(-5.23280973732471,-8.9,139.41268825531));
#41655=CARTESIAN_POINT('Ctrl Pts',(-5.23280973732471,-8.9,139.982810974121));
#41656=CARTESIAN_POINT('Ctrl Pts',(-5.48635645210743,-9.,138.749454975128));
#41657=CARTESIAN_POINT('Ctrl Pts',(-5.48635645210743,-8.9,138.749454975128));
#41658=CARTESIAN_POINT('Ctrl Pts',(-5.35600157082081,-9.,138.874079704285));
#41659=CARTESIAN_POINT('Ctrl Pts',(-5.35600157082081,-8.9,138.874079704285));
#41660=CARTESIAN_POINT('Ctrl Pts',(-5.29440565407276,-9.,139.143383979797));
#41661=CARTESIAN_POINT('Ctrl Pts',(-5.29440565407276,-8.9,139.143383979797));
#41662=CARTESIAN_POINT('',(-5.48635645210743,-9.,138.749454975128));
#41663=CARTESIAN_POINT('Ctrl Pts',(-5.48635645210743,-9.,138.749454975128));
#41664=CARTESIAN_POINT('Ctrl Pts',(-5.35600157082081,-9.,138.874079704285));
#41665=CARTESIAN_POINT('Ctrl Pts',(-5.29440565407276,-9.,139.143383979797));
#41666=CARTESIAN_POINT('',(-5.48635645210743,-8.9,138.749454975128));
#41667=CARTESIAN_POINT('',(-5.48635645210743,-9.,138.749454975128));
#41668=CARTESIAN_POINT('Ctrl Pts',(-5.48635645210743,-8.9,138.749454975128));
#41669=CARTESIAN_POINT('Ctrl Pts',(-5.35600157082081,-8.9,138.874079704285));
#41670=CARTESIAN_POINT('Ctrl Pts',(-5.29440565407276,-8.9,139.143383979797));
#41671=CARTESIAN_POINT('Ctrl Pts',(-5.7943379431963,-9.,138.624830245972));
#41672=CARTESIAN_POINT('Ctrl Pts',(-5.7943379431963,-8.9,138.624830245972));
#41673=CARTESIAN_POINT('Ctrl Pts',(-5.61671133339405,-9.,138.624830245972));
#41674=CARTESIAN_POINT('Ctrl Pts',(-5.61671133339405,-8.9,138.624830245972));
#41675=CARTESIAN_POINT('Ctrl Pts',(-5.48635645210743,-9.,138.749454975128));
#41676=CARTESIAN_POINT('Ctrl Pts',(-5.48635645210743,-8.9,138.749454975128));
#41677=CARTESIAN_POINT('',(-5.7943379431963,-9.,138.624830245972));
#41678=CARTESIAN_POINT('Ctrl Pts',(-5.7943379431963,-9.,138.624830245972));
#41679=CARTESIAN_POINT('Ctrl Pts',(-5.61671133339405,-9.,138.624830245972));
#41680=CARTESIAN_POINT('Ctrl Pts',(-5.48635645210743,-9.,138.749454975128));
#41681=CARTESIAN_POINT('',(-5.7943379431963,-8.9,138.624830245972));
#41682=CARTESIAN_POINT('',(-5.7943379431963,-9.,138.624830245972));
#41683=CARTESIAN_POINT('Ctrl Pts',(-5.7943379431963,-8.9,138.624830245972));
#41684=CARTESIAN_POINT('Ctrl Pts',(-5.61671133339405,-8.9,138.624830245972));
#41685=CARTESIAN_POINT('Ctrl Pts',(-5.48635645210743,-8.9,138.749454975128));
#41686=CARTESIAN_POINT('Ctrl Pts',(-6.20545549690723,-9.,138.918486118317));
#41687=CARTESIAN_POINT('Ctrl Pts',(-6.20545549690723,-8.9,138.918486118317));
#41688=CARTESIAN_POINT('Ctrl Pts',(-6.06364221870899,-9.,138.624830245972));
#41689=CARTESIAN_POINT('Ctrl Pts',(-6.06364221870899,-8.9,138.624830245972));
#41690=CARTESIAN_POINT('Ctrl Pts',(-5.7943379431963,-9.,138.624830245972));
#41691=CARTESIAN_POINT('Ctrl Pts',(-5.7943379431963,-8.9,138.624830245972));
#41692=CARTESIAN_POINT('',(-6.20545549690723,-9.,138.918486118317));
#41693=CARTESIAN_POINT('Ctrl Pts',(-6.20545549690723,-9.,138.918486118317));
#41694=CARTESIAN_POINT('Ctrl Pts',(-6.06364221870899,-9.,138.624830245972));
#41695=CARTESIAN_POINT('Ctrl Pts',(-5.7943379431963,-9.,138.624830245972));
#41696=CARTESIAN_POINT('',(-6.20545549690723,-8.9,138.918486118317));
#41697=CARTESIAN_POINT('',(-6.20545549690723,-9.,138.918486118317));
#41698=CARTESIAN_POINT('Ctrl Pts',(-6.20545549690723,-8.9,138.918486118317));
#41699=CARTESIAN_POINT('Ctrl Pts',(-6.06364221870899,-8.9,138.624830245972));
#41700=CARTESIAN_POINT('Ctrl Pts',(-5.7943379431963,-8.9,138.624830245972));
#41701=CARTESIAN_POINT('Ctrl Pts',(-6.34727068245411,-9.,140.014325141907));
#41702=CARTESIAN_POINT('Ctrl Pts',(-6.34727068245411,-8.9,140.014325141907));
#41703=CARTESIAN_POINT('Ctrl Pts',(-6.34727068245411,-9.,139.212142467499));
#41704=CARTESIAN_POINT('Ctrl Pts',(-6.34727068245411,-8.9,139.212142467499));
#41705=CARTESIAN_POINT('Ctrl Pts',(-6.20545549690723,-9.,138.918486118317));
#41706=CARTESIAN_POINT('Ctrl Pts',(-6.20545549690723,-8.9,138.918486118317));
#41707=CARTESIAN_POINT('',(-6.34727068245411,-9.,140.014325141907));
#41708=CARTESIAN_POINT('Ctrl Pts',(-6.34727068245411,-9.,140.014325141907));
#41709=CARTESIAN_POINT('Ctrl Pts',(-6.34727068245411,-9.,139.212142467499));
#41710=CARTESIAN_POINT('Ctrl Pts',(-6.20545549690723,-9.,138.918486118317));
#41711=CARTESIAN_POINT('',(-6.34727068245411,-8.9,140.014325141907));
#41712=CARTESIAN_POINT('',(-6.34727068245411,-9.,140.014325141907));
#41713=CARTESIAN_POINT('Ctrl Pts',(-6.34727068245411,-8.9,140.014325141907));
#41714=CARTESIAN_POINT('Ctrl Pts',(-6.34727068245411,-8.9,139.212142467499));
#41715=CARTESIAN_POINT('Ctrl Pts',(-6.20545549690723,-8.9,138.918486118317));
#41716=CARTESIAN_POINT('Ctrl Pts',(-6.21834821999073,-9.,141.101569652557));
#41717=CARTESIAN_POINT('Ctrl Pts',(-6.21834821999073,-8.9,141.101569652557));
#41718=CARTESIAN_POINT('Ctrl Pts',(-6.34727068245411,-9.,140.807913303375));
#41719=CARTESIAN_POINT('Ctrl Pts',(-6.34727068245411,-8.9,140.807913303375));
#41720=CARTESIAN_POINT('Ctrl Pts',(-6.34727068245411,-9.,140.014325141907));
#41721=CARTESIAN_POINT('Ctrl Pts',(-6.34727068245411,-8.9,140.014325141907));
#41722=CARTESIAN_POINT('',(-6.21834821999073,-9.,141.101569652557));
#41723=CARTESIAN_POINT('Ctrl Pts',(-6.21834821999073,-9.,141.101569652557));
#41724=CARTESIAN_POINT('Ctrl Pts',(-6.34727068245411,-9.,140.807913303375));
#41725=CARTESIAN_POINT('Ctrl Pts',(-6.34727068245411,-9.,140.014325141907));
#41726=CARTESIAN_POINT('',(-6.21834821999073,-8.9,141.101569652557));
#41727=CARTESIAN_POINT('',(-6.21834821999073,-9.,141.101569652557));
#41728=CARTESIAN_POINT('Ctrl Pts',(-6.21834821999073,-8.9,141.101569652557));
#41729=CARTESIAN_POINT('Ctrl Pts',(-6.34727068245411,-8.9,140.807913303375));
#41730=CARTESIAN_POINT('Ctrl Pts',(-6.34727068245411,-8.9,140.014325141907));
#41731=CARTESIAN_POINT('Ctrl Pts',(-5.80006761848927,-9.,141.395225763321));
#41732=CARTESIAN_POINT('Ctrl Pts',(-5.80006761848927,-8.9,141.395225763321));
#41733=CARTESIAN_POINT('Ctrl Pts',(-6.08942575752735,-9.,141.395225763321));
#41734=CARTESIAN_POINT('Ctrl Pts',(-6.08942575752735,-8.9,141.395225763321));
#41735=CARTESIAN_POINT('Ctrl Pts',(-6.21834821999073,-9.,141.101569652557));
#41736=CARTESIAN_POINT('Ctrl Pts',(-6.21834821999073,-8.9,141.101569652557));
#41737=CARTESIAN_POINT('Ctrl Pts',(-5.80006761848927,-9.,141.395225763321));
#41738=CARTESIAN_POINT('Ctrl Pts',(-6.08942575752735,-9.,141.395225763321));
#41739=CARTESIAN_POINT('Ctrl Pts',(-6.21834821999073,-9.,141.101569652557));
#41740=CARTESIAN_POINT('Ctrl Pts',(-5.80006761848927,-8.9,141.395225763321));
#41741=CARTESIAN_POINT('Ctrl Pts',(-6.08942575752735,-8.9,141.395225763321));
#41742=CARTESIAN_POINT('Ctrl Pts',(-6.21834821999073,-8.9,141.101569652557));
#41743=CARTESIAN_POINT('Ctrl Pts',(-7.1838323622942,-9.,138.493042945862));
#41744=CARTESIAN_POINT('Ctrl Pts',(-7.1838323622942,-8.9,138.493042945862));
#41745=CARTESIAN_POINT('Ctrl Pts',(-7.33567447960377,-9.,138.725102901459));
#41746=CARTESIAN_POINT('Ctrl Pts',(-7.33567447960377,-8.9,138.725102901459));
#41747=CARTESIAN_POINT('Ctrl Pts',(-7.42019005119801,-9.,139.127626895905));
#41748=CARTESIAN_POINT('Ctrl Pts',(-7.42019005119801,-8.9,139.127626895905));
#41749=CARTESIAN_POINT('',(-7.1838323622942,-8.9,138.493042945862));
#41750=CARTESIAN_POINT('',(-7.1838323622942,-9.,138.493042945862));
#41751=CARTESIAN_POINT('',(-7.42019005119801,-8.9,139.127626895905));
#41752=CARTESIAN_POINT('Ctrl Pts',(-7.1838323622942,-8.9,138.493042945862));
#41753=CARTESIAN_POINT('Ctrl Pts',(-7.33567447960377,-8.9,138.725102901459));
#41754=CARTESIAN_POINT('Ctrl Pts',(-7.42019005119801,-8.9,139.127626895905));
#41755=CARTESIAN_POINT('',(-7.42019005119801,-9.,139.127626895905));
#41756=CARTESIAN_POINT('Ctrl Pts',(-6.64808912575245,-9.,137.997408390045));
#41757=CARTESIAN_POINT('Ctrl Pts',(-6.64808912575245,-8.9,137.997408390045));
#41758=CARTESIAN_POINT('Ctrl Pts',(-6.97469206154346,-9.,138.166440010071));
#41759=CARTESIAN_POINT('Ctrl Pts',(-6.97469206154346,-8.9,138.166440010071));
#41760=CARTESIAN_POINT('Ctrl Pts',(-7.1838323622942,-9.,138.493042945862));
#41761=CARTESIAN_POINT('Ctrl Pts',(-7.1838323622942,-8.9,138.493042945862));
#41762=CARTESIAN_POINT('',(-6.64808912575245,-8.9,137.997408390045));
#41763=CARTESIAN_POINT('',(-6.64808912575245,-9.,137.997408390045));
#41764=CARTESIAN_POINT('Ctrl Pts',(-6.64808912575245,-8.9,137.997408390045));
#41765=CARTESIAN_POINT('Ctrl Pts',(-6.97469206154346,-8.9,138.166440010071));
#41766=CARTESIAN_POINT('Ctrl Pts',(-7.1838323622942,-8.9,138.493042945862));
#41767=CARTESIAN_POINT('Ctrl Pts',(-5.7914721518755,-9.,137.828377246857));
#41768=CARTESIAN_POINT('Ctrl Pts',(-5.7914721518755,-8.9,137.828377246857));
#41769=CARTESIAN_POINT('Ctrl Pts',(-6.32148618996143,-9.,137.828377246857));
#41770=CARTESIAN_POINT('Ctrl Pts',(-6.32148618996143,-8.9,137.828377246857));
#41771=CARTESIAN_POINT('Ctrl Pts',(-6.64808912575245,-9.,137.997408390045));
#41772=CARTESIAN_POINT('Ctrl Pts',(-6.64808912575245,-8.9,137.997408390045));
#41773=CARTESIAN_POINT('',(-5.7914721518755,-8.9,137.828377246857));
#41774=CARTESIAN_POINT('',(-5.7914721518755,-9.,137.828377246857));
#41775=CARTESIAN_POINT('Ctrl Pts',(-5.7914721518755,-8.9,137.828377246857));
#41776=CARTESIAN_POINT('Ctrl Pts',(-6.32148618996143,-8.9,137.828377246857));
#41777=CARTESIAN_POINT('Ctrl Pts',(-6.64808912575245,-8.9,137.997408390045));
#41778=CARTESIAN_POINT('Ctrl Pts',(-4.45927591621876,-9.,138.358390808105));
#41779=CARTESIAN_POINT('Ctrl Pts',(-4.45927591621876,-8.9,138.358390808105));
#41780=CARTESIAN_POINT('Ctrl Pts',(-4.84604234993458,-9.,137.828377246857));
#41781=CARTESIAN_POINT('Ctrl Pts',(-4.84604234993458,-8.9,137.828377246857));
#41782=CARTESIAN_POINT('Ctrl Pts',(-5.7914721518755,-9.,137.828377246857));
#41783=CARTESIAN_POINT('Ctrl Pts',(-5.7914721518755,-8.9,137.828377246857));
#41784=CARTESIAN_POINT('',(-4.45927591621876,-8.9,138.358390808105));
#41785=CARTESIAN_POINT('',(-4.45927591621876,-9.,138.358390808105));
#41786=CARTESIAN_POINT('Ctrl Pts',(-4.45927591621876,-8.9,138.358390808105));
#41787=CARTESIAN_POINT('Ctrl Pts',(-4.84604234993458,-8.9,137.828377246857));
#41788=CARTESIAN_POINT('Ctrl Pts',(-5.7914721518755,-8.9,137.828377246857));
#41789=CARTESIAN_POINT('Ctrl Pts',(-4.07250948250294,-9.,140.031514644623));
#41790=CARTESIAN_POINT('Ctrl Pts',(-4.07250948250294,-8.9,140.031514644623));
#41791=CARTESIAN_POINT('Ctrl Pts',(-4.07250948250294,-9.,138.888404369354));
#41792=CARTESIAN_POINT('Ctrl Pts',(-4.07250948250294,-8.9,138.888404369354));
#41793=CARTESIAN_POINT('Ctrl Pts',(-4.45927591621876,-9.,138.358390808105));
#41794=CARTESIAN_POINT('Ctrl Pts',(-4.45927591621876,-8.9,138.358390808105));
#41795=CARTESIAN_POINT('',(-4.07250948250294,-8.9,140.031514644623));
#41796=CARTESIAN_POINT('',(-4.07250948250294,-9.,140.031514644623));
#41797=CARTESIAN_POINT('Ctrl Pts',(-4.07250948250294,-8.9,140.031514644623));
#41798=CARTESIAN_POINT('Ctrl Pts',(-4.07250948250294,-8.9,138.888404369354));
#41799=CARTESIAN_POINT('Ctrl Pts',(-4.45927591621876,-8.9,138.358390808105));
#41800=CARTESIAN_POINT('Ctrl Pts',(-4.18997164070606,-9.,141.011323928833));
#41801=CARTESIAN_POINT('Ctrl Pts',(-4.18997164070606,-8.9,141.011323928833));
#41802=CARTESIAN_POINT('Ctrl Pts',(-4.07250948250294,-9.,140.541473865509));
#41803=CARTESIAN_POINT('Ctrl Pts',(-4.07250948250294,-8.9,140.541473865509));
#41804=CARTESIAN_POINT('Ctrl Pts',(-4.07250948250294,-9.,140.031514644623));
#41805=CARTESIAN_POINT('Ctrl Pts',(-4.07250948250294,-8.9,140.031514644623));
#41806=CARTESIAN_POINT('',(-4.18997164070606,-8.9,141.011323928833));
#41807=CARTESIAN_POINT('',(-4.18997164070606,-9.,141.011323928833));
#41808=CARTESIAN_POINT('Ctrl Pts',(-4.18997164070606,-8.9,141.011323928833));
#41809=CARTESIAN_POINT('Ctrl Pts',(-4.07250948250294,-8.9,140.541473865509));
#41810=CARTESIAN_POINT('Ctrl Pts',(-4.07250948250294,-8.9,140.031514644623));
#41811=CARTESIAN_POINT('Ctrl Pts',(-4.34897585213184,-9.,141.442497253418));
#41812=CARTESIAN_POINT('Ctrl Pts',(-4.34897585213184,-8.9,141.442497253418));
#41813=CARTESIAN_POINT('Ctrl Pts',(-4.25013513863087,-9.,141.2577085495));
#41814=CARTESIAN_POINT('Ctrl Pts',(-4.25013513863087,-8.9,141.2577085495));
#41815=CARTESIAN_POINT('Ctrl Pts',(-4.18997164070606,-9.,141.011323928833));
#41816=CARTESIAN_POINT('Ctrl Pts',(-4.18997164070606,-8.9,141.011323928833));
#41817=CARTESIAN_POINT('',(-4.34897585213184,-8.9,141.442497253418));
#41818=CARTESIAN_POINT('',(-4.34897585213184,-9.,141.442497253418));
#41819=CARTESIAN_POINT('Ctrl Pts',(-4.34897585213184,-8.9,141.442497253418));
#41820=CARTESIAN_POINT('Ctrl Pts',(-4.25013513863087,-8.9,141.2577085495));
#41821=CARTESIAN_POINT('Ctrl Pts',(-4.18997164070606,-8.9,141.011323928833));
#41822=CARTESIAN_POINT('Ctrl Pts',(-4.61971254646778,-9.,141.794884681702));
#41823=CARTESIAN_POINT('Ctrl Pts',(-4.61971254646778,-8.9,141.794884681702));
#41824=CARTESIAN_POINT('Ctrl Pts',(-4.44781656563282,-9.,141.627285718918));
#41825=CARTESIAN_POINT('Ctrl Pts',(-4.44781656563282,-8.9,141.627285718918));
#41826=CARTESIAN_POINT('Ctrl Pts',(-4.34897585213184,-9.,141.442497253418));
#41827=CARTESIAN_POINT('Ctrl Pts',(-4.34897585213184,-8.9,141.442497253418));
#41828=CARTESIAN_POINT('',(-4.61971254646778,-8.9,141.794884681702));
#41829=CARTESIAN_POINT('',(-4.61971254646778,-9.,141.794884681702));
#41830=CARTESIAN_POINT('Ctrl Pts',(-4.61971254646778,-8.9,141.794884681702));
#41831=CARTESIAN_POINT('Ctrl Pts',(-4.44781656563282,-8.9,141.627285718918));
#41832=CARTESIAN_POINT('Ctrl Pts',(-4.34897585213184,-8.9,141.442497253418));
#41833=CARTESIAN_POINT('Ctrl Pts',(-5.06377764046192,-9.,142.067054271698));
#41834=CARTESIAN_POINT('Ctrl Pts',(-5.06377764046192,-8.9,142.067054271698));
#41835=CARTESIAN_POINT('Ctrl Pts',(-4.79160852730274,-9.,141.962483882904));
#41836=CARTESIAN_POINT('Ctrl Pts',(-4.79160852730274,-8.9,141.962483882904));
#41837=CARTESIAN_POINT('Ctrl Pts',(-4.61971254646778,-9.,141.794884681702));
#41838=CARTESIAN_POINT('Ctrl Pts',(-4.61971254646778,-8.9,141.794884681702));
#41839=CARTESIAN_POINT('',(-5.06377764046192,-8.9,142.067054271698));
#41840=CARTESIAN_POINT('',(-5.06377764046192,-9.,142.067054271698));
#41841=CARTESIAN_POINT('Ctrl Pts',(-5.06377764046192,-8.9,142.067054271698));
#41842=CARTESIAN_POINT('Ctrl Pts',(-4.79160852730274,-8.9,141.962483882904));
#41843=CARTESIAN_POINT('Ctrl Pts',(-4.61971254646778,-8.9,141.794884681702));
#41844=CARTESIAN_POINT('Ctrl Pts',(-5.75995798408985,-9.,142.171624183655));
#41845=CARTESIAN_POINT('Ctrl Pts',(-5.75995798408985,-8.9,142.171624183655));
#41846=CARTESIAN_POINT('Ctrl Pts',(-5.3359467536211,-9.,142.171624183655));
#41847=CARTESIAN_POINT('Ctrl Pts',(-5.3359467536211,-8.9,142.171624183655));
#41848=CARTESIAN_POINT('Ctrl Pts',(-5.06377764046192,-9.,142.067054271698));
#41849=CARTESIAN_POINT('Ctrl Pts',(-5.06377764046192,-8.9,142.067054271698));
#41850=CARTESIAN_POINT('',(-5.75995798408985,-8.9,142.171624183655));
#41851=CARTESIAN_POINT('',(-5.75995798408985,-9.,142.171624183655));
#41852=CARTESIAN_POINT('Ctrl Pts',(-5.75995798408985,-8.9,142.171624183655));
#41853=CARTESIAN_POINT('Ctrl Pts',(-5.3359467536211,-8.9,142.171624183655));
#41854=CARTESIAN_POINT('Ctrl Pts',(-5.06377764046192,-8.9,142.067054271698));
#41855=CARTESIAN_POINT('Ctrl Pts',(-7.07353182137012,-9.,141.693179368973));
#41856=CARTESIAN_POINT('Ctrl Pts',(-7.07353182137012,-8.9,141.693179368973));
#41857=CARTESIAN_POINT('Ctrl Pts',(-6.64235849678516,-9.,142.171624183655));
#41858=CARTESIAN_POINT('Ctrl Pts',(-6.64235849678516,-8.9,142.171624183655));
#41859=CARTESIAN_POINT('Ctrl Pts',(-5.75995798408985,-9.,142.171624183655));
#41860=CARTESIAN_POINT('Ctrl Pts',(-5.75995798408985,-8.9,142.171624183655));
#41861=CARTESIAN_POINT('',(-7.07353182137012,-8.9,141.693179368973));
#41862=CARTESIAN_POINT('',(-7.07353182137012,-9.,141.693179368973));
#41863=CARTESIAN_POINT('Ctrl Pts',(-7.07353182137012,-8.9,141.693179368973));
#41864=CARTESIAN_POINT('Ctrl Pts',(-6.64235849678516,-8.9,142.171624183655));
#41865=CARTESIAN_POINT('Ctrl Pts',(-5.75995798408985,-8.9,142.171624183655));
#41866=CARTESIAN_POINT('Ctrl Pts',(-7.50470562279224,-9.,140.01719045639));
#41867=CARTESIAN_POINT('Ctrl Pts',(-7.50470562279224,-8.9,140.01719045639));
#41868=CARTESIAN_POINT('Ctrl Pts',(-7.50470562279224,-9.,141.214734554291));
#41869=CARTESIAN_POINT('Ctrl Pts',(-7.50470562279224,-8.9,141.214734554291));
#41870=CARTESIAN_POINT('Ctrl Pts',(-7.07353182137012,-9.,141.693179368973));
#41871=CARTESIAN_POINT('Ctrl Pts',(-7.07353182137012,-8.9,141.693179368973));
#41872=CARTESIAN_POINT('',(-7.50470562279224,-8.9,140.01719045639));
#41873=CARTESIAN_POINT('',(-7.50470562279224,-9.,140.01719045639));
#41874=CARTESIAN_POINT('Ctrl Pts',(-7.50470562279224,-8.9,140.01719045639));
#41875=CARTESIAN_POINT('Ctrl Pts',(-7.50470562279224,-8.9,141.214734554291));
#41876=CARTESIAN_POINT('Ctrl Pts',(-7.07353182137012,-8.9,141.693179368973));
#41877=CARTESIAN_POINT('Ctrl Pts',(-7.42019005119801,-9.,139.127626895905));
#41878=CARTESIAN_POINT('Ctrl Pts',(-7.42019005119801,-8.9,139.127626895905));
#41879=CARTESIAN_POINT('Ctrl Pts',(-7.50470562279224,-9.,139.53015089035));
#41880=CARTESIAN_POINT('Ctrl Pts',(-7.50470562279224,-8.9,139.53015089035));
#41881=CARTESIAN_POINT('Ctrl Pts',(-7.50470562279224,-9.,140.01719045639));
#41882=CARTESIAN_POINT('Ctrl Pts',(-7.50470562279224,-8.9,140.01719045639));
#41883=CARTESIAN_POINT('Ctrl Pts',(-7.42019005119801,-8.9,139.127626895905));
#41884=CARTESIAN_POINT('Ctrl Pts',(-7.50470562279224,-8.9,139.53015089035));
#41885=CARTESIAN_POINT('Ctrl Pts',(-7.50470562279224,-8.9,140.01719045639));
#41886=CARTESIAN_POINT('Origin',(-5.78860755264759,-8.9,140.000000715256));
#41887=CARTESIAN_POINT('Origin',(-9.82530565559864,-9.,138.851160049438));
#41888=CARTESIAN_POINT('',(-9.82530565559864,-8.9,138.851160049438));
#41889=CARTESIAN_POINT('',(-9.82530565559864,-9.,138.851160049438));
#41890=CARTESIAN_POINT('',(-8.00320501625538,-8.9,138.851160049438));
#41891=CARTESIAN_POINT('',(-9.82530565559864,-8.9,138.851160049438));
#41892=CARTESIAN_POINT('',(-8.00320501625538,-9.,138.851160049438));
#41893=CARTESIAN_POINT('Ctrl Pts',(-9.54597444832325,-9.,139.106139659882));
#41894=CARTESIAN_POINT('Ctrl Pts',(-9.54597444832325,-8.9,139.106139659882));
#41895=CARTESIAN_POINT('Ctrl Pts',(-9.66486950218678,-9.,139.008731842041));
#41896=CARTESIAN_POINT('Ctrl Pts',(-9.66486950218678,-8.9,139.008731842041));
#41897=CARTESIAN_POINT('Ctrl Pts',(-9.82530565559864,-9.,138.851160049438));
#41898=CARTESIAN_POINT('Ctrl Pts',(-9.82530565559864,-8.9,138.851160049438));
#41899=CARTESIAN_POINT('',(-9.54597444832325,-8.9,139.106139659882));
#41900=CARTESIAN_POINT('',(-9.54597444832325,-9.,139.106139659882));
#41901=CARTESIAN_POINT('Ctrl Pts',(-9.54597444832325,-8.9,139.106139659882));
#41902=CARTESIAN_POINT('Ctrl Pts',(-9.66486950218678,-8.9,139.008731842041));
#41903=CARTESIAN_POINT('Ctrl Pts',(-9.82530565559864,-8.9,138.851160049438));
#41904=CARTESIAN_POINT('Ctrl Pts',(-9.07469196617603,-9.,139.447067260742));
#41905=CARTESIAN_POINT('Ctrl Pts',(-9.07469196617603,-8.9,139.447067260742));
#41906=CARTESIAN_POINT('Ctrl Pts',(-9.42707939445972,-9.,139.203547477722));
#41907=CARTESIAN_POINT('Ctrl Pts',(-9.42707939445972,-8.9,139.203547477722));
#41908=CARTESIAN_POINT('Ctrl Pts',(-9.54597444832325,-9.,139.106139659882));
#41909=CARTESIAN_POINT('Ctrl Pts',(-9.54597444832325,-8.9,139.106139659882));
#41910=CARTESIAN_POINT('',(-9.07469196617603,-8.9,139.447067260742));
#41911=CARTESIAN_POINT('',(-9.07469196617603,-9.,139.447067260742));
#41912=CARTESIAN_POINT('Ctrl Pts',(-9.07469196617603,-8.9,139.447067260742));
#41913=CARTESIAN_POINT('Ctrl Pts',(-9.42707939445972,-8.9,139.203547477722));
#41914=CARTESIAN_POINT('Ctrl Pts',(-9.54597444832325,-8.9,139.106139659882));
#41915=CARTESIAN_POINT('Ctrl Pts',(-8.25675220787525,-9.,140.214870929718));
#41916=CARTESIAN_POINT('Ctrl Pts',(-8.25675220787525,-8.9,140.214870929718));
#41917=CARTESIAN_POINT('Ctrl Pts',(-8.48165006935596,-9.,139.865348339081));
#41918=CARTESIAN_POINT('Ctrl Pts',(-8.48165006935596,-8.9,139.865348339081));
#41919=CARTESIAN_POINT('Ctrl Pts',(-9.07469196617603,-9.,139.447067260742));
#41920=CARTESIAN_POINT('Ctrl Pts',(-9.07469196617603,-8.9,139.447067260742));
#41921=CARTESIAN_POINT('',(-8.25675220787525,-8.9,140.214870929718));
#41922=CARTESIAN_POINT('',(-8.25675220787525,-9.,140.214870929718));
#41923=CARTESIAN_POINT('Ctrl Pts',(-8.25675220787525,-8.9,140.214870929718));
#41924=CARTESIAN_POINT('Ctrl Pts',(-8.48165006935596,-8.9,139.865348339081));
#41925=CARTESIAN_POINT('Ctrl Pts',(-9.07469196617603,-8.9,139.447067260742));
#41926=CARTESIAN_POINT('Ctrl Pts',(-8.03185434639454,-9.,140.948295116425));
#41927=CARTESIAN_POINT('Ctrl Pts',(-8.03185434639454,-8.9,140.948295116425));
#41928=CARTESIAN_POINT('Ctrl Pts',(-8.03185434639454,-9.,140.564393520355));
#41929=CARTESIAN_POINT('Ctrl Pts',(-8.03185434639454,-8.9,140.564393520355));
#41930=CARTESIAN_POINT('Ctrl Pts',(-8.25675220787525,-9.,140.214870929718));
#41931=CARTESIAN_POINT('Ctrl Pts',(-8.25675220787525,-8.9,140.214870929718));
#41932=CARTESIAN_POINT('',(-8.03185434639454,-8.9,140.948295116425));
#41933=CARTESIAN_POINT('',(-8.03185434639454,-9.,140.948295116425));
#41934=CARTESIAN_POINT('Ctrl Pts',(-8.03185434639454,-8.9,140.948295116425));
#41935=CARTESIAN_POINT('Ctrl Pts',(-8.03185434639454,-8.9,140.564393520355));
#41936=CARTESIAN_POINT('Ctrl Pts',(-8.25675220787525,-8.9,140.214870929718));
#41937=CARTESIAN_POINT('Ctrl Pts',(-8.22810240089893,-9.,141.600068569183));
#41938=CARTESIAN_POINT('Ctrl Pts',(-8.22810240089893,-8.9,141.600068569183));
#41939=CARTESIAN_POINT('Ctrl Pts',(-8.03185434639454,-9.,141.309277296066));
#41940=CARTESIAN_POINT('Ctrl Pts',(-8.03185434639454,-8.9,141.309277296066));
#41941=CARTESIAN_POINT('Ctrl Pts',(-8.03185434639454,-9.,140.948295116425));
#41942=CARTESIAN_POINT('Ctrl Pts',(-8.03185434639454,-8.9,140.948295116425));
#41943=CARTESIAN_POINT('',(-8.22810240089893,-8.9,141.600068569183));
#41944=CARTESIAN_POINT('',(-8.22810240089893,-9.,141.600068569183));
#41945=CARTESIAN_POINT('Ctrl Pts',(-8.22810240089893,-8.9,141.600068569183));
#41946=CARTESIAN_POINT('Ctrl Pts',(-8.03185434639454,-8.9,141.309277296066));
#41947=CARTESIAN_POINT('Ctrl Pts',(-8.03185434639454,-8.9,140.948295116425));
#41948=CARTESIAN_POINT('Ctrl Pts',(-8.76671095192432,-9.,142.031241893768));
#41949=CARTESIAN_POINT('Ctrl Pts',(-8.76671095192432,-8.9,142.031241893768));
#41950=CARTESIAN_POINT('Ctrl Pts',(-8.42435093224049,-9.,141.8908598423));
#41951=CARTESIAN_POINT('Ctrl Pts',(-8.42435093224049,-8.9,141.8908598423));
#41952=CARTESIAN_POINT('Ctrl Pts',(-8.22810240089893,-9.,141.600068569183));
#41953=CARTESIAN_POINT('Ctrl Pts',(-8.22810240089893,-8.9,141.600068569183));
#41954=CARTESIAN_POINT('',(-8.76671095192432,-8.9,142.031241893768));
#41955=CARTESIAN_POINT('',(-8.76671095192432,-9.,142.031241893768));
#41956=CARTESIAN_POINT('Ctrl Pts',(-8.76671095192432,-8.9,142.031241893768));
#41957=CARTESIAN_POINT('Ctrl Pts',(-8.42435093224049,-8.9,141.8908598423));
#41958=CARTESIAN_POINT('Ctrl Pts',(-8.22810240089893,-8.9,141.600068569183));
#41959=CARTESIAN_POINT('Ctrl Pts',(-9.72503300011158,-9.,142.171623706818));
#41960=CARTESIAN_POINT('Ctrl Pts',(-9.72503300011158,-8.9,142.171623706818));
#41961=CARTESIAN_POINT('Ctrl Pts',(-9.10907144844532,-9.,142.171623706818));
#41962=CARTESIAN_POINT('Ctrl Pts',(-9.10907144844532,-8.9,142.171623706818));
#41963=CARTESIAN_POINT('Ctrl Pts',(-8.76671095192432,-9.,142.031241893768));
#41964=CARTESIAN_POINT('Ctrl Pts',(-8.76671095192432,-8.9,142.031241893768));
#41965=CARTESIAN_POINT('',(-9.72503300011158,-8.9,142.171623706818));
#41966=CARTESIAN_POINT('',(-9.72503300011158,-9.,142.171623706818));
#41967=CARTESIAN_POINT('Ctrl Pts',(-9.72503300011158,-8.9,142.171623706818));
#41968=CARTESIAN_POINT('Ctrl Pts',(-9.10907144844532,-8.9,142.171623706818));
#41969=CARTESIAN_POINT('Ctrl Pts',(-8.76671095192432,-8.9,142.031241893768));
#41970=CARTESIAN_POINT('Ctrl Pts',(-10.6489760428667,-9.,142.024079322815));
#41971=CARTESIAN_POINT('Ctrl Pts',(-10.6489760428667,-8.9,142.024079322815));
#41972=CARTESIAN_POINT('Ctrl Pts',(-10.3152105361223,-9.,142.171623706818));
#41973=CARTESIAN_POINT('Ctrl Pts',(-10.3152105361223,-8.9,142.171623706818));
#41974=CARTESIAN_POINT('Ctrl Pts',(-9.72503300011158,-9.,142.171623706818));
#41975=CARTESIAN_POINT('Ctrl Pts',(-9.72503300011158,-8.9,142.171623706818));
#41976=CARTESIAN_POINT('',(-10.6489760428667,-8.9,142.024079322815));
#41977=CARTESIAN_POINT('',(-10.6489760428667,-9.,142.024079322815));
#41978=CARTESIAN_POINT('Ctrl Pts',(-10.6489760428667,-8.9,142.024079322815));
#41979=CARTESIAN_POINT('Ctrl Pts',(-10.3152105361223,-8.9,142.171623706818));
#41980=CARTESIAN_POINT('Ctrl Pts',(-9.72503300011158,-8.9,142.171623706818));
#41981=CARTESIAN_POINT('Ctrl Pts',(-11.1660971194506,-9.,141.600068569183));
#41982=CARTESIAN_POINT('Ctrl Pts',(-11.1660971194506,-8.9,141.600068569183));
#41983=CARTESIAN_POINT('Ctrl Pts',(-10.9827410727739,-9.,141.876535177231));
#41984=CARTESIAN_POINT('Ctrl Pts',(-10.9827410727739,-8.9,141.876535177231));
#41985=CARTESIAN_POINT('Ctrl Pts',(-10.6489760428667,-9.,142.024079322815));
#41986=CARTESIAN_POINT('Ctrl Pts',(-10.6489760428667,-8.9,142.024079322815));
#41987=CARTESIAN_POINT('',(-11.1660971194506,-8.9,141.600068569183));
#41988=CARTESIAN_POINT('',(-11.1660971194506,-9.,141.600068569183));
#41989=CARTESIAN_POINT('Ctrl Pts',(-11.1660971194506,-8.9,141.600068569183));
#41990=CARTESIAN_POINT('Ctrl Pts',(-10.9827410727739,-8.9,141.876535177231));
#41991=CARTESIAN_POINT('Ctrl Pts',(-10.6489760428667,-8.9,142.024079322815));
#41992=CARTESIAN_POINT('Ctrl Pts',(-11.4182116538286,-9.,140.830832958221));
#41993=CARTESIAN_POINT('Ctrl Pts',(-11.4182116538286,-8.9,140.830832958221));
#41994=CARTESIAN_POINT('Ctrl Pts',(-11.3494531661272,-9.,141.323601961136));
#41995=CARTESIAN_POINT('Ctrl Pts',(-11.3494531661272,-8.9,141.323601961136));
#41996=CARTESIAN_POINT('Ctrl Pts',(-11.1660971194506,-9.,141.600068569183));
#41997=CARTESIAN_POINT('Ctrl Pts',(-11.1660971194506,-8.9,141.600068569183));
#41998=CARTESIAN_POINT('',(-11.4182116538286,-8.9,140.830832958221));
#41999=CARTESIAN_POINT('',(-11.4182116538286,-9.,140.830832958221));
#42000=CARTESIAN_POINT('Ctrl Pts',(-11.4182116538286,-8.9,140.830832958221));
#42001=CARTESIAN_POINT('Ctrl Pts',(-11.3494531661272,-8.9,141.323601961136));
#42002=CARTESIAN_POINT('Ctrl Pts',(-11.1660971194506,-8.9,141.600068569183));
#42003=CARTESIAN_POINT('Origin',(-10.2493168860674,-9.,140.73628950119));
#42004=CARTESIAN_POINT('',(-10.2493168860674,-8.9,140.73628950119));
#42005=CARTESIAN_POINT('',(-10.2493168860674,-9.,140.73628950119));
#42006=CARTESIAN_POINT('',(-10.2493168860674,-8.9,140.73628950119));
#42007=CARTESIAN_POINT('Ctrl Pts',(-10.058798506856,-9.,141.231924057007));
#42008=CARTESIAN_POINT('Ctrl Pts',(-10.058798506856,-8.9,141.231924057007));
#42009=CARTESIAN_POINT('Ctrl Pts',(-10.2006127387285,-9.,141.09154176712));
#42010=CARTESIAN_POINT('Ctrl Pts',(-10.2006127387285,-8.9,141.09154176712));
#42011=CARTESIAN_POINT('Ctrl Pts',(-10.2493168860674,-9.,140.73628950119));
#42012=CARTESIAN_POINT('Ctrl Pts',(-10.2493168860674,-8.9,140.73628950119));
#42013=CARTESIAN_POINT('',(-10.058798506856,-8.9,141.231924057007));
#42014=CARTESIAN_POINT('',(-10.058798506856,-9.,141.231924057007));
#42015=CARTESIAN_POINT('Ctrl Pts',(-10.058798506856,-8.9,141.231924057007));
#42016=CARTESIAN_POINT('Ctrl Pts',(-10.2006127387285,-8.9,141.09154176712));
#42017=CARTESIAN_POINT('Ctrl Pts',(-10.2493168860674,-8.9,140.73628950119));
#42018=CARTESIAN_POINT('Ctrl Pts',(-9.69351883232594,-9.,141.372305870056));
#42019=CARTESIAN_POINT('Ctrl Pts',(-9.69351883232594,-8.9,141.372305870056));
#42020=CARTESIAN_POINT('Ctrl Pts',(-9.91698379814625,-9.,141.372305870056));
#42021=CARTESIAN_POINT('Ctrl Pts',(-9.91698379814625,-8.9,141.372305870056));
#42022=CARTESIAN_POINT('Ctrl Pts',(-10.058798506856,-9.,141.231924057007));
#42023=CARTESIAN_POINT('Ctrl Pts',(-10.058798506856,-8.9,141.231924057007));
#42024=CARTESIAN_POINT('',(-9.69351883232594,-8.9,141.372305870056));
#42025=CARTESIAN_POINT('',(-9.69351883232594,-9.,141.372305870056));
#42026=CARTESIAN_POINT('Ctrl Pts',(-9.69351883232594,-8.9,141.372305870056));
#42027=CARTESIAN_POINT('Ctrl Pts',(-9.91698379814625,-8.9,141.372305870056));
#42028=CARTESIAN_POINT('Ctrl Pts',(-10.058798506856,-8.9,141.231924057007));
#42029=CARTESIAN_POINT('Ctrl Pts',(-9.33683367073536,-9.,141.236221313477));
#42030=CARTESIAN_POINT('Ctrl Pts',(-9.33683367073536,-8.9,141.236221313477));
#42031=CARTESIAN_POINT('Ctrl Pts',(-9.47864837944508,-9.,141.372305870056));
#42032=CARTESIAN_POINT('Ctrl Pts',(-9.47864837944508,-8.9,141.372305870056));
#42033=CARTESIAN_POINT('Ctrl Pts',(-9.69351883232594,-9.,141.372305870056));
#42034=CARTESIAN_POINT('Ctrl Pts',(-9.69351883232594,-8.9,141.372305870056));
#42035=CARTESIAN_POINT('',(-9.33683367073536,-8.9,141.236221313477));
#42036=CARTESIAN_POINT('',(-9.33683367073536,-9.,141.236221313477));
#42037=CARTESIAN_POINT('Ctrl Pts',(-9.33683367073536,-8.9,141.236221313477));
#42038=CARTESIAN_POINT('Ctrl Pts',(-9.47864837944508,-8.9,141.372305870056));
#42039=CARTESIAN_POINT('Ctrl Pts',(-9.69351883232594,-8.9,141.372305870056));
#42040=CARTESIAN_POINT('Ctrl Pts',(-9.1950194388628,-9.,140.908185958862));
#42041=CARTESIAN_POINT('Ctrl Pts',(-9.1950194388628,-8.9,140.908185958862));
#42042=CARTESIAN_POINT('Ctrl Pts',(-9.1950194388628,-9.,141.100136756897));
#42043=CARTESIAN_POINT('Ctrl Pts',(-9.1950194388628,-8.9,141.100136756897));
#42044=CARTESIAN_POINT('Ctrl Pts',(-9.33683367073536,-9.,141.236221313477));
#42045=CARTESIAN_POINT('Ctrl Pts',(-9.33683367073536,-8.9,141.236221313477));
#42046=CARTESIAN_POINT('',(-9.1950194388628,-8.9,140.908185958862));
#42047=CARTESIAN_POINT('',(-9.1950194388628,-9.,140.908185958862));
#42048=CARTESIAN_POINT('Ctrl Pts',(-9.1950194388628,-8.9,140.908185958862));
#42049=CARTESIAN_POINT('Ctrl Pts',(-9.1950194388628,-8.9,141.100136756897));
#42050=CARTESIAN_POINT('Ctrl Pts',(-9.33683367073536,-8.9,141.236221313477));
#42051=CARTESIAN_POINT('Ctrl Pts',(-9.3382660895586,-9.,140.53287935257));
#42052=CARTESIAN_POINT('Ctrl Pts',(-9.3382660895586,-8.9,140.53287935257));
#42053=CARTESIAN_POINT('Ctrl Pts',(-9.1950194388628,-9.,140.730559825897));
#42054=CARTESIAN_POINT('Ctrl Pts',(-9.1950194388628,-8.9,140.730559825897));
#42055=CARTESIAN_POINT('Ctrl Pts',(-9.1950194388628,-9.,140.908185958862));
#42056=CARTESIAN_POINT('Ctrl Pts',(-9.1950194388628,-8.9,140.908185958862));
#42057=CARTESIAN_POINT('',(-9.3382660895586,-8.9,140.53287935257));
#42058=CARTESIAN_POINT('',(-9.3382660895586,-9.,140.53287935257));
#42059=CARTESIAN_POINT('Ctrl Pts',(-9.3382660895586,-8.9,140.53287935257));
#42060=CARTESIAN_POINT('Ctrl Pts',(-9.1950194388628,-8.9,140.730559825897));
#42061=CARTESIAN_POINT('Ctrl Pts',(-9.1950194388628,-8.9,140.908185958862));
#42062=CARTESIAN_POINT('Ctrl Pts',(-9.99433727562428,-9.,139.954161167145));
#42063=CARTESIAN_POINT('Ctrl Pts',(-9.99433727562428,-8.9,139.954161167145));
#42064=CARTESIAN_POINT('Ctrl Pts',(-9.48151321709156,-9.,140.335197925568));
#42065=CARTESIAN_POINT('Ctrl Pts',(-9.48151321709156,-8.9,140.335197925568));
#42066=CARTESIAN_POINT('Ctrl Pts',(-9.3382660895586,-9.,140.53287935257));
#42067=CARTESIAN_POINT('Ctrl Pts',(-9.3382660895586,-8.9,140.53287935257));
#42068=CARTESIAN_POINT('',(-9.99433727562428,-8.9,139.954161167145));
#42069=CARTESIAN_POINT('',(-9.99433727562428,-9.,139.954161167145));
#42070=CARTESIAN_POINT('Ctrl Pts',(-9.99433727562428,-8.9,139.954161167145));
#42071=CARTESIAN_POINT('Ctrl Pts',(-9.48151321709156,-8.9,140.335197925568));
#42072=CARTESIAN_POINT('Ctrl Pts',(-9.3382660895586,-8.9,140.53287935257));
#42073=CARTESIAN_POINT('Ctrl Pts',(-11.1388804465532,-9.,138.875512123108));
#42074=CARTESIAN_POINT('Ctrl Pts',(-11.1388804465532,-8.9,138.875512123108));
#42075=CARTESIAN_POINT('Ctrl Pts',(-10.833764269948,-9.,139.332469940186));
#42076=CARTESIAN_POINT('Ctrl Pts',(-10.833764269948,-8.9,139.332469940186));
#42077=CARTESIAN_POINT('Ctrl Pts',(-9.99433727562428,-9.,139.954161167145));
#42078=CARTESIAN_POINT('Ctrl Pts',(-9.99433727562428,-8.9,139.954161167145));
#42079=CARTESIAN_POINT('',(-11.1388804465532,-8.9,138.875512123108));
#42080=CARTESIAN_POINT('',(-11.1388804465532,-9.,138.875512123108));
#42081=CARTESIAN_POINT('Ctrl Pts',(-11.1388804465532,-8.9,138.875512123108));
#42082=CARTESIAN_POINT('Ctrl Pts',(-10.833764269948,-8.9,139.332469940186));
#42083=CARTESIAN_POINT('Ctrl Pts',(-9.99433727562428,-8.9,139.954161167145));
#42084=CARTESIAN_POINT('Ctrl Pts',(-11.5041598826647,-9.,137.900000572205));
#42085=CARTESIAN_POINT('Ctrl Pts',(-11.5041598826647,-8.9,137.900000572205));
#42086=CARTESIAN_POINT('Ctrl Pts',(-11.4439961463213,-9.,138.41855430603));
#42087=CARTESIAN_POINT('Ctrl Pts',(-11.4439961463213,-8.9,138.41855430603));
#42088=CARTESIAN_POINT('Ctrl Pts',(-11.1388804465532,-9.,138.875512123108));
#42089=CARTESIAN_POINT('Ctrl Pts',(-11.1388804465532,-8.9,138.875512123108));
#42090=CARTESIAN_POINT('',(-11.5041598826647,-8.9,137.900000572205));
#42091=CARTESIAN_POINT('',(-11.5041598826647,-9.,137.900000572205));
#42092=CARTESIAN_POINT('Ctrl Pts',(-11.5041598826647,-8.9,137.900000572205));
#42093=CARTESIAN_POINT('Ctrl Pts',(-11.4439961463213,-8.9,138.41855430603));
#42094=CARTESIAN_POINT('Ctrl Pts',(-11.1388804465532,-8.9,138.875512123108));
#42095=CARTESIAN_POINT('Origin',(-8.00320501625538,-9.,137.900000572205));
#42096=CARTESIAN_POINT('',(-8.00320501625538,-8.9,137.900000572205));
#42097=CARTESIAN_POINT('',(-8.00320501625538,-9.,137.900000572205));
#42098=CARTESIAN_POINT('',(-8.00320501625538,-8.9,137.900000572205));
#42099=CARTESIAN_POINT('Origin',(-8.00320501625538,-9.,138.851160049438));
#42100=CARTESIAN_POINT('',(-8.00320501625538,-8.9,138.851160049438));
#42101=CARTESIAN_POINT('Origin',(-9.75368244946003,-8.9,140.035812139511));
#42102=CARTESIAN_POINT('Origin',(8.70797948539257,-9.,137.900000572205));
#42103=CARTESIAN_POINT('',(8.70797948539257,-8.9,137.900000572205));
#42104=CARTESIAN_POINT('',(8.70797948539257,-9.,137.900000572205));
#42105=CARTESIAN_POINT('',(7.4875166863203,-8.9,137.900000572205));
#42106=CARTESIAN_POINT('',(8.70797948539257,-8.9,137.900000572205));
#42107=CARTESIAN_POINT('',(7.4875166863203,-9.,137.900000572205));
#42108=CARTESIAN_POINT('Origin',(8.70797948539257,-9.,140.206097126007));
#42109=CARTESIAN_POINT('',(8.70797948539257,-8.9,140.206097126007));
#42110=CARTESIAN_POINT('',(8.70797948539257,-9.,140.206097126007));
#42111=CARTESIAN_POINT('',(8.70797948539257,-8.9,140.206097126007));
#42112=CARTESIAN_POINT('Origin',(10.2808306664228,-9.,137.900000572205));
#42113=CARTESIAN_POINT('',(10.2808306664228,-8.9,137.900000572205));
#42114=CARTESIAN_POINT('',(10.2808306664228,-9.,137.900000572205));
#42115=CARTESIAN_POINT('',(10.2808306664228,-8.9,137.900000572205));
#42116=CARTESIAN_POINT('Origin',(11.5041602104902,-9.,137.900000572205));
#42117=CARTESIAN_POINT('',(11.5041602104902,-8.9,137.900000572205));
#42118=CARTESIAN_POINT('',(11.5041602104902,-9.,137.900000572205));
#42119=CARTESIAN_POINT('',(11.5041602104902,-8.9,137.900000572205));
#42120=CARTESIAN_POINT('Origin',(11.5041602104902,-9.,142.10000038147));
#42121=CARTESIAN_POINT('',(11.5041602104902,-8.9,142.10000038147));
#42122=CARTESIAN_POINT('',(11.5041602104902,-9.,142.10000038147));
#42123=CARTESIAN_POINT('',(11.5041602104902,-8.9,142.10000038147));
#42124=CARTESIAN_POINT('Origin',(10.2808306664228,-9.,142.10000038147));
#42125=CARTESIAN_POINT('',(10.2808306664228,-8.9,142.10000038147));
#42126=CARTESIAN_POINT('',(10.2808306664228,-9.,142.10000038147));
#42127=CARTESIAN_POINT('',(10.2808306664228,-8.9,142.10000038147));
#42128=CARTESIAN_POINT('Origin',(10.2808306664228,-9.,139.776356220245));
#42129=CARTESIAN_POINT('',(10.2808306664228,-8.9,139.776356220245));
#42130=CARTESIAN_POINT('',(10.2808306664228,-9.,139.776356220245));
#42131=CARTESIAN_POINT('',(10.2808306664228,-8.9,139.776356220245));
#42132=CARTESIAN_POINT('Origin',(8.69938497245312,-9.,142.10000038147));
#42133=CARTESIAN_POINT('',(8.69938497245312,-8.9,142.10000038147));
#42134=CARTESIAN_POINT('',(8.69938497245312,-9.,142.10000038147));
#42135=CARTESIAN_POINT('',(8.69938497245312,-8.9,142.10000038147));
#42136=CARTESIAN_POINT('Origin',(7.4875166863203,-9.,142.10000038147));
#42137=CARTESIAN_POINT('',(7.4875166863203,-8.9,142.10000038147));
#42138=CARTESIAN_POINT('',(7.4875166863203,-9.,142.10000038147));
#42139=CARTESIAN_POINT('',(7.4875166863203,-8.9,142.10000038147));
#42140=CARTESIAN_POINT('Origin',(7.4875166863203,-9.,137.900000572205));
#42141=CARTESIAN_POINT('',(7.4875166863203,-8.9,137.900000572205));
#42142=CARTESIAN_POINT('Origin',(9.49583844840527,-8.9,140.000000476837));
#42143=CARTESIAN_POINT('Origin',(-38.,-9.,145.));
#42144=CARTESIAN_POINT('Origin',(-38.,-9.,145.));
#42145=CARTESIAN_POINT('Origin',(0.,0.,135.));
#42146=CARTESIAN_POINT('',(-25.8,9.,135.));
#42147=CARTESIAN_POINT('Origin',(-25.8,9.,134.));
#42148=CARTESIAN_POINT('',(-25.8,0.,135.));
#42149=CARTESIAN_POINT('Origin',(-38.,4.,135.));
#42150=CARTESIAN_POINT('Origin',(-38.,4.8,144.2));
#42151=CARTESIAN_POINT('Origin',(-38.,-9.,135.));
#42152=CARTESIAN_POINT('Origin',(-38.,-4.8,144.2));
#42153=CARTESIAN_POINT('',(0.,0.,0.));
#42154=CARTESIAN_POINT('Origin',(-37.95,-4.65,103.7));
#42155=CARTESIAN_POINT('',(-37.9,-4.7,98.6));
#42156=CARTESIAN_POINT('',(-37.9,-4.7,105.4));
#42157=CARTESIAN_POINT('',(-37.9,-4.7,103.7));
#42158=CARTESIAN_POINT('',(-38.,-4.6,105.5));
#42159=CARTESIAN_POINT('',(-37.1875,-5.41250000000001,104.6875));
#42160=CARTESIAN_POINT('',(-38.,-4.6,98.5));
#42161=CARTESIAN_POINT('',(-38.,-4.6,103.7));
#42162=CARTESIAN_POINT('',(-38.,-4.6,98.5));
#42163=CARTESIAN_POINT('Origin',(-37.95,-5.525,98.55));
#42164=CARTESIAN_POINT('',(-38.,-8.5,98.5));
#42165=CARTESIAN_POINT('',(-38.,-5.525,98.5));
#42166=CARTESIAN_POINT('',(-37.95,-8.55,98.55));
#42167=CARTESIAN_POINT('',(-38.1625,-8.33749999999998,98.3375));
#42168=CARTESIAN_POINT('',(-37.9,-8.5,98.6));
#42169=CARTESIAN_POINT('',(-37.4541666666667,-8.05416666666666,99.0458333333333));
#42170=CARTESIAN_POINT('',(-37.9,-5.525,98.6));
#42171=CARTESIAN_POINT('Origin',(-38.,-4.7,105.4));
#42172=CARTESIAN_POINT('',(37.9,-4.7,98.6));
#42173=CARTESIAN_POINT('',(-38.,-4.7,98.6));
#42174=CARTESIAN_POINT('',(37.9,-4.7,105.4));
#42175=CARTESIAN_POINT('',(37.9,-4.7,103.7));
#42176=CARTESIAN_POINT('',(-38.,-4.7,105.4));
#42177=CARTESIAN_POINT('Origin',(-38.,-4.7,98.6));
#42178=CARTESIAN_POINT('',(37.9,-8.5,98.6));
#42179=CARTESIAN_POINT('',(-38.,-8.5,98.6));
#42180=CARTESIAN_POINT('',(37.9,-5.525,98.6));
#42181=CARTESIAN_POINT('Origin',(-38.,-8.55,98.55));
#42182=CARTESIAN_POINT('',(-37.9,-8.6,98.5));
#42183=CARTESIAN_POINT('',(-38.25,-8.25000000000001,98.85));
#42184=CARTESIAN_POINT('',(37.9,-8.6,98.5));
#42185=CARTESIAN_POINT('',(-38.,-8.6,98.5));
#42186=CARTESIAN_POINT('',(37.95,-8.55,98.55));
#42187=CARTESIAN_POINT('',(25.5833333333338,-20.9166666666669,86.1833333333338));
#42188=CARTESIAN_POINT('',(24.7875000000004,4.61250000000026,111.7125));
#42189=CARTESIAN_POINT('Origin',(-37.95,7.475,98.55));
#42190=CARTESIAN_POINT('',(-37.9,4.7,98.6));
#42191=CARTESIAN_POINT('',(-37.9,8.5,98.6));
#42192=CARTESIAN_POINT('',(-37.9,7.475,98.6));
#42193=CARTESIAN_POINT('',(-37.95,8.55,98.55));
#42194=CARTESIAN_POINT('',(-37.7791666666667,8.37916666666666,98.7208333333333));
#42195=CARTESIAN_POINT('',(-38.,8.5,98.5));
#42196=CARTESIAN_POINT('',(-37.8875,8.61249999999999,98.6125));
#42197=CARTESIAN_POINT('',(-38.,4.6,98.5));
#42198=CARTESIAN_POINT('',(-38.,7.475,98.5));
#42199=CARTESIAN_POINT('',(-38.,4.6,98.5));
#42200=CARTESIAN_POINT('Origin',(-37.95,4.65,100.3));
#42201=CARTESIAN_POINT('',(-37.9,4.7,105.4));
#42202=CARTESIAN_POINT('',(-37.9,4.7,100.3));
#42203=CARTESIAN_POINT('',(-38.,4.6,105.5));
#42204=CARTESIAN_POINT('',(-38.,4.6,100.3));
#42205=CARTESIAN_POINT('',(-38.,4.6,105.5));
#42206=CARTESIAN_POINT('Origin',(-37.95,5.525,105.45));
#42207=CARTESIAN_POINT('',(-38.,8.5,105.5));
#42208=CARTESIAN_POINT('',(-38.,5.525,105.5));
#42209=CARTESIAN_POINT('',(-37.95,8.55,105.45));
#42210=CARTESIAN_POINT('',(-38.1625,8.33749999999997,105.6625));
#42211=CARTESIAN_POINT('',(-37.9,8.5,105.4));
#42212=CARTESIAN_POINT('',(-37.4541666666667,8.05416666666663,104.954166666667));
#42213=CARTESIAN_POINT('',(-37.9,5.525,105.4));
#42214=CARTESIAN_POINT('Origin',(-38.,8.55,98.55));
#42215=CARTESIAN_POINT('',(37.9,8.5,98.6));
#42216=CARTESIAN_POINT('',(-38.,8.5,98.6));
#42217=CARTESIAN_POINT('',(37.95,8.54999999999999,98.55));
#42218=CARTESIAN_POINT('',(25.1125000000005,-4.28750000000024,111.3875));
#42219=CARTESIAN_POINT('',(37.9,8.6,98.5));
#42220=CARTESIAN_POINT('',(25.5333333333338,20.9666666666669,86.1333333333338));
#42221=CARTESIAN_POINT('',(-37.9,8.6,98.5));
#42222=CARTESIAN_POINT('',(-38.,8.6,98.5));
#42223=CARTESIAN_POINT('',(-38.2,8.3,98.8));
#42224=CARTESIAN_POINT('Origin',(-38.,8.6,98.6));
#42225=CARTESIAN_POINT('',(37.9,4.7,98.6));
#42226=CARTESIAN_POINT('',(-38.,4.7,98.6));
#42227=CARTESIAN_POINT('',(37.9,7.475,98.6));
#42228=CARTESIAN_POINT('Origin',(-38.,4.7,98.6));
#42229=CARTESIAN_POINT('',(37.9,4.7,105.4));
#42230=CARTESIAN_POINT('',(-38.,4.7,105.4));
#42231=CARTESIAN_POINT('',(37.9,4.7,100.3));
#42232=CARTESIAN_POINT('Origin',(-38.,4.7,105.4));
#42233=CARTESIAN_POINT('',(37.9,8.5,105.4));
#42234=CARTESIAN_POINT('',(-38.,8.5,105.4));
#42235=CARTESIAN_POINT('',(37.9,5.525,105.4));
#42236=CARTESIAN_POINT('Origin',(-38.,8.55,105.45));
#42237=CARTESIAN_POINT('',(-37.9,8.6,105.5));
#42238=CARTESIAN_POINT('',(-38.25,8.25,105.15));
#42239=CARTESIAN_POINT('',(37.9,8.6,105.5));
#42240=CARTESIAN_POINT('',(-38.,8.6,105.5));
#42241=CARTESIAN_POINT('',(37.95,8.55,105.45));
#42242=CARTESIAN_POINT('',(25.5833333333338,20.9166666666669,117.816666666666));
#42243=CARTESIAN_POINT('',(24.7875000000004,-4.61250000000026,92.2875000000004));
#42244=CARTESIAN_POINT('Origin',(-37.95,-5.225,105.95));
#42245=CARTESIAN_POINT('',(-37.95,-8.55,105.95));
#42246=CARTESIAN_POINT('',(-37.9,-8.5,106.));
#42247=CARTESIAN_POINT('',(-37.4041666666666,-8.00416666666666,106.495833333333));
#42248=CARTESIAN_POINT('',(-37.9,-4.2,106.));
#42249=CARTESIAN_POINT('',(-37.9,-5.225,106.));
#42250=CARTESIAN_POINT('',(-37.95,-4.15,105.95));
#42251=CARTESIAN_POINT('',(-37.7791666666667,-4.32083333333333,106.120833333333));
#42252=CARTESIAN_POINT('',(-38.,-4.2,105.9));
#42253=CARTESIAN_POINT('',(-39.1208333333333,-5.32083333333331,104.779166666667));
#42254=CARTESIAN_POINT('',(-38.,-8.5,105.9));
#42255=CARTESIAN_POINT('',(-38.,-5.225,105.9));
#42256=CARTESIAN_POINT('',(-38.8291666666667,-7.67083333333333,105.070833333333));
#42257=CARTESIAN_POINT('Origin',(-38.,-8.55,105.95));
#42258=CARTESIAN_POINT('',(-37.9,-8.6,105.9));
#42259=CARTESIAN_POINT('',(-37.6333333333333,-8.86666666666666,105.633333333333));
#42260=CARTESIAN_POINT('',(-25.7,-8.6,105.9));
#42261=CARTESIAN_POINT('',(-38.,-8.6,105.9));
#42262=CARTESIAN_POINT('',(-25.8,-8.5,106.));
#42263=CARTESIAN_POINT('',(-25.7,-8.6,105.9));
#42264=CARTESIAN_POINT('',(-38.,-8.5,106.));
#42265=CARTESIAN_POINT('Origin',(-37.95,-8.55,104.));
#42266=CARTESIAN_POINT('',(-38.,-8.5,105.5));
#42267=CARTESIAN_POINT('',(-38.,-8.5,104.));
#42268=CARTESIAN_POINT('',(-37.95,-8.55000000000001,105.45));
#42269=CARTESIAN_POINT('',(-37.8875,-8.61249999999999,105.3875));
#42270=CARTESIAN_POINT('',(-37.9,-8.6,105.5));
#42271=CARTESIAN_POINT('',(-38.2,-8.30000000000001,105.2));
#42272=CARTESIAN_POINT('',(-37.9,-8.6,104.));
#42273=CARTESIAN_POINT('Origin',(-38.,-6.35,102.));
#42274=CARTESIAN_POINT('',(-38.,-7.475,105.5));
#42275=CARTESIAN_POINT('',(-38.,-4.2,98.1));
#42276=CARTESIAN_POINT('',(-38.,-4.2,100.));
#42277=CARTESIAN_POINT('',(-38.,-8.5,98.1));
#42278=CARTESIAN_POINT('',(-38.,-7.475,98.1));
#42279=CARTESIAN_POINT('',(-38.,-8.5,100.3));
#42280=CARTESIAN_POINT('Origin',(-38.,-8.55,105.95));
#42281=CARTESIAN_POINT('',(25.7,-8.6,105.9));
#42282=CARTESIAN_POINT('',(37.9,-8.6,105.9));
#42283=CARTESIAN_POINT('',(-38.,-8.6,105.9));
#42284=CARTESIAN_POINT('',(37.95,-8.55000000000001,105.95));
#42285=CARTESIAN_POINT('',(24.9666666666671,-21.5333333333336,92.9666666666671));
#42286=CARTESIAN_POINT('',(37.9,-8.5,106.));
#42287=CARTESIAN_POINT('',(24.7375000000004,4.66250000000027,119.1625));
#42288=CARTESIAN_POINT('',(25.8,-8.5,106.));
#42289=CARTESIAN_POINT('',(-38.,-8.5,106.));
#42290=CARTESIAN_POINT('',(25.8,-8.5,106.));
#42291=CARTESIAN_POINT('Origin',(25.75,-8.55,106.));
#42292=CARTESIAN_POINT('',(25.8,-8.5,106.85));
#42293=CARTESIAN_POINT('',(25.8,-8.5,106.));
#42294=CARTESIAN_POINT('',(25.75,-8.55,106.9));
#42295=CARTESIAN_POINT('',(26.6,-7.70000000000001,106.05));
#42296=CARTESIAN_POINT('',(25.7,-8.6,106.85));
#42297=CARTESIAN_POINT('',(18.1500000000004,-16.1499999999998,99.2999999999999));
#42298=CARTESIAN_POINT('',(25.7,-8.6,106.));
#42299=CARTESIAN_POINT('Origin',(-38.,-8.6,106.));
#42300=CARTESIAN_POINT('',(-25.7,-8.6,106.85));
#42301=CARTESIAN_POINT('',(-19.,-8.6,106.85));
#42302=CARTESIAN_POINT('',(-25.7,-8.6,106.));
#42303=CARTESIAN_POINT('',(37.9,-8.6,105.5));
#42304=CARTESIAN_POINT('',(-38.,-8.6,105.5));
#42305=CARTESIAN_POINT('',(37.9,-8.6,104.));
#42306=CARTESIAN_POINT('Origin',(-19.,-8.525,106.925));
#42307=CARTESIAN_POINT('',(25.65,-8.45,107.));
#42308=CARTESIAN_POINT('',(25.65,-8.45,107.));
#42309=CARTESIAN_POINT('',(-25.65,-8.45,107.));
#42310=CARTESIAN_POINT('',(-19.,-8.45,107.));
#42311=CARTESIAN_POINT('',(-25.75,-8.55,106.9));
#42312=CARTESIAN_POINT('',(-25.65,-8.45,107.));
#42313=CARTESIAN_POINT('',(-24.4833333333334,-9.81666666666663,105.633333333333));
#42314=CARTESIAN_POINT('Origin',(25.725,-4.3,106.925));
#42315=CARTESIAN_POINT('',(25.8,8.5,106.85));
#42316=CARTESIAN_POINT('',(25.8,-4.3,106.85));
#42317=CARTESIAN_POINT('',(25.75,8.55,106.9));
#42318=CARTESIAN_POINT('',(28.0833333333333,6.21666666666668,104.566666666667));
#42319=CARTESIAN_POINT('',(25.65,8.45,107.));
#42320=CARTESIAN_POINT('',(25.65,8.45,107.));
#42321=CARTESIAN_POINT('',(25.65,-4.3,107.));
#42322=CARTESIAN_POINT('Origin',(-37.95,-7.475,105.45));
#42323=CARTESIAN_POINT('',(-37.9,-8.5,105.4));
#42324=CARTESIAN_POINT('',(-37.9,-7.475,105.4));
#42325=CARTESIAN_POINT('',(-37.7791666666667,-8.37916666666666,105.279166666667));
#42326=CARTESIAN_POINT('Origin',(-38.,-8.55,105.45));
#42327=CARTESIAN_POINT('',(37.9,-8.5,105.4));
#42328=CARTESIAN_POINT('',(-38.,-8.5,105.4));
#42329=CARTESIAN_POINT('',(37.95,-8.54999999999999,105.45));
#42330=CARTESIAN_POINT('',(25.1125000000005,4.28750000000024,92.6125000000005));
#42331=CARTESIAN_POINT('',(25.5333333333338,-20.9666666666669,117.866666666666));
#42332=CARTESIAN_POINT('Origin',(37.95,-8.55,104.));
#42333=CARTESIAN_POINT('',(38.,-8.5,105.5));
#42334=CARTESIAN_POINT('',(37.8875,-8.61249999999999,105.3875));
#42335=CARTESIAN_POINT('',(38.,-8.5,105.9));
#42336=CARTESIAN_POINT('',(38.,-8.5,104.));
#42337=CARTESIAN_POINT('',(38.8291666666667,-7.67083333333329,105.070833333333));
#42338=CARTESIAN_POINT('Origin',(37.95,-7.475,105.45));
#42339=CARTESIAN_POINT('',(37.9,-7.475,105.4));
#42340=CARTESIAN_POINT('',(38.,-4.6,105.5));
#42341=CARTESIAN_POINT('',(38.,-4.6,105.5));
#42342=CARTESIAN_POINT('',(38.,-7.475,105.5));
#42343=CARTESIAN_POINT('Origin',(-37.95,8.55,100.));
#42344=CARTESIAN_POINT('',(-37.9,8.6,98.1));
#42345=CARTESIAN_POINT('',(-37.9,8.6,100.));
#42346=CARTESIAN_POINT('',(-37.95,8.55000000000001,98.05));
#42347=CARTESIAN_POINT('',(-37.6333333333333,8.86666666666667,98.3666666666667));
#42348=CARTESIAN_POINT('',(-38.,8.5,98.1));
#42349=CARTESIAN_POINT('',(-38.8291666666667,7.67083333333329,98.9291666666667));
#42350=CARTESIAN_POINT('',(-38.,8.5,100.));
#42351=CARTESIAN_POINT('Origin',(-38.,8.6,98.));
#42352=CARTESIAN_POINT('',(37.9,8.6,98.1));
#42353=CARTESIAN_POINT('',(37.9,8.6,100.));
#42354=CARTESIAN_POINT('',(25.7,8.6,98.1));
#42355=CARTESIAN_POINT('',(-38.,8.6,98.1));
#42356=CARTESIAN_POINT('',(25.7,8.6,97.15));
#42357=CARTESIAN_POINT('',(25.7,8.6,97.5));
#42358=CARTESIAN_POINT('',(-25.7,8.6,97.15));
#42359=CARTESIAN_POINT('',(-19.,8.6,97.15));
#42360=CARTESIAN_POINT('',(-25.7,8.6,98.1));
#42361=CARTESIAN_POINT('',(-25.7,8.6,97.5));
#42362=CARTESIAN_POINT('',(-38.,8.6,98.1));
#42363=CARTESIAN_POINT('Origin',(-38.,8.55,98.05));
#42364=CARTESIAN_POINT('',(-25.8,8.5,98.));
#42365=CARTESIAN_POINT('',(-27.8833333333335,6.41666666666659,95.9166666666667));
#42366=CARTESIAN_POINT('',(-37.9,8.5,98.));
#42367=CARTESIAN_POINT('',(-38.,8.5,98.));
#42368=CARTESIAN_POINT('',(-37.4041666666667,8.00416666666663,97.5041666666666));
#42369=CARTESIAN_POINT('Origin',(-37.95,5.225,98.05));
#42370=CARTESIAN_POINT('',(-37.9,4.2,98.));
#42371=CARTESIAN_POINT('',(-37.9,5.225,98.));
#42372=CARTESIAN_POINT('',(-38.,4.2,98.1));
#42373=CARTESIAN_POINT('',(-37.9,4.2,98.));
#42374=CARTESIAN_POINT('',(-38.,5.225,98.1));
#42375=CARTESIAN_POINT('Origin',(-25.75,-8.55,106.));
#42376=CARTESIAN_POINT('',(-25.8,-8.5,106.85));
#42377=CARTESIAN_POINT('',(-28.0333333333333,-6.26666666666668,104.616666666667));
#42378=CARTESIAN_POINT('',(-25.8,-8.5,106.));
#42379=CARTESIAN_POINT('Origin',(-38.,-4.1,106.));
#42380=CARTESIAN_POINT('',(-25.8,-4.2,106.));
#42381=CARTESIAN_POINT('',(-25.8,2.25,106.));
#42382=CARTESIAN_POINT('',(-38.,-4.2,106.));
#42383=CARTESIAN_POINT('Origin',(-25.8,8.6,106.));
#42384=CARTESIAN_POINT('',(-25.8,8.5,106.85));
#42385=CARTESIAN_POINT('',(-25.8,4.3,106.85));
#42386=CARTESIAN_POINT('',(-25.8,8.5,106.));
#42387=CARTESIAN_POINT('',(-25.8,8.5,105.7));
#42388=CARTESIAN_POINT('',(-25.8,4.2,106.));
#42389=CARTESIAN_POINT('',(-25.8,8.6,106.));
#42390=CARTESIAN_POINT('',(-25.8,4.1,105.9));
#42391=CARTESIAN_POINT('',(-25.8,5.27500000000006,107.075));
#42392=CARTESIAN_POINT('',(-25.8,4.1,106.1));
#42393=CARTESIAN_POINT('',(-25.8,4.1,106.));
#42394=CARTESIAN_POINT('',(-25.8,-4.1,106.1));
#42395=CARTESIAN_POINT('',(-25.8,4.3,106.1));
#42396=CARTESIAN_POINT('',(-25.8,-4.1,105.9));
#42397=CARTESIAN_POINT('',(-25.8,-4.1,102.));
#42398=CARTESIAN_POINT('',(-25.8,-0.974999999999829,102.775));
#42399=CARTESIAN_POINT('Origin',(-25.725,4.3,106.925));
#42400=CARTESIAN_POINT('',(-25.65,8.45,107.));
#42401=CARTESIAN_POINT('',(-25.65,4.3,107.));
#42402=CARTESIAN_POINT('',(-25.75,8.55,106.9));
#42403=CARTESIAN_POINT('',(-25.65,8.45,107.));
#42404=CARTESIAN_POINT('',(-26.65,7.65000000000004,106.));
#42405=CARTESIAN_POINT('Origin',(-38.,4.2,98.1));
#42406=CARTESIAN_POINT('',(-37.9,4.1,98.1));
#42407=CARTESIAN_POINT('',(-37.9,4.1,98.1));
#42408=CARTESIAN_POINT('',(-38.,4.2,98.1));
#42409=CARTESIAN_POINT('Origin',(-37.95,4.15,104.));
#42410=CARTESIAN_POINT('',(-37.95,4.15,105.95));
#42411=CARTESIAN_POINT('',(-38.,4.2,105.9));
#42412=CARTESIAN_POINT('',(-38.8291666666667,5.02916666666671,105.070833333333));
#42413=CARTESIAN_POINT('',(-38.,4.2,104.));
#42414=CARTESIAN_POINT('',(-37.9,4.1,105.9));
#42415=CARTESIAN_POINT('',(-37.9,4.1,104.));
#42416=CARTESIAN_POINT('',(-37.6333333333333,3.83333333333332,105.633333333333));
#42417=CARTESIAN_POINT('Origin',(-38.,4.15,98.05));
#42418=CARTESIAN_POINT('',(-25.8,4.2,98.));
#42419=CARTESIAN_POINT('',(-25.8,4.1,98.1));
#42420=CARTESIAN_POINT('',(-25.8,5.52500000000006,96.675));
#42421=CARTESIAN_POINT('',(-38.,4.1,98.1));
#42422=CARTESIAN_POINT('',(-38.,4.2,98.));
#42423=CARTESIAN_POINT('Origin',(-38.,6.35,102.));
#42424=CARTESIAN_POINT('',(-38.,8.5,105.9));
#42425=CARTESIAN_POINT('',(-38.,7.475,105.9));
#42426=CARTESIAN_POINT('',(-38.,8.5,103.7));
#42427=CARTESIAN_POINT('Origin',(-37.95,7.475,105.95));
#42428=CARTESIAN_POINT('',(-37.9,4.2,106.));
#42429=CARTESIAN_POINT('',(-38.,4.1,105.9));
#42430=CARTESIAN_POINT('',(-37.9,8.5,106.));
#42431=CARTESIAN_POINT('',(-37.9,7.475,106.));
#42432=CARTESIAN_POINT('',(-37.95,8.55,105.95));
#42433=CARTESIAN_POINT('',(-37.7791666666667,8.37916666666665,106.120833333333));
#42434=CARTESIAN_POINT('',(-38.5041666666667,7.99583333333331,105.395833333333));
#42435=CARTESIAN_POINT('Origin',(-38.,4.15,105.95));
#42436=CARTESIAN_POINT('',(-38.,4.1,105.9));
#42437=CARTESIAN_POINT('',(-38.,4.2,106.));
#42438=CARTESIAN_POINT('Origin',(-38.,4.1,106.));
#42439=CARTESIAN_POINT('',(-25.8,4.1,97.9));
#42440=CARTESIAN_POINT('',(-25.8,4.1,101.5));
#42441=CARTESIAN_POINT('',(-25.7,4.1,98.));
#42442=CARTESIAN_POINT('',(-26.8000000000002,4.1,96.8999999999998));
#42443=CARTESIAN_POINT('',(25.7,4.1,98.));
#42444=CARTESIAN_POINT('',(-38.,4.1,98.));
#42445=CARTESIAN_POINT('',(25.8,4.1,97.9));
#42446=CARTESIAN_POINT('',(7.79999999999887,4.1,115.9));
#42447=CARTESIAN_POINT('',(25.8,4.1,98.1));
#42448=CARTESIAN_POINT('',(25.8,4.1,101.5));
#42449=CARTESIAN_POINT('',(37.9,4.1,98.1));
#42450=CARTESIAN_POINT('',(-38.,4.1,98.1));
#42451=CARTESIAN_POINT('',(37.9,4.1,105.9));
#42452=CARTESIAN_POINT('',(37.9,4.1,104.));
#42453=CARTESIAN_POINT('',(25.8,4.1,105.9));
#42454=CARTESIAN_POINT('',(-38.,4.1,105.9));
#42455=CARTESIAN_POINT('',(25.8,4.1,106.1));
#42456=CARTESIAN_POINT('',(25.8,4.1,106.));
#42457=CARTESIAN_POINT('',(25.7,4.1,106.));
#42458=CARTESIAN_POINT('',(9.79999999999887,4.1,90.1));
#42459=CARTESIAN_POINT('',(-25.7,4.1,106.));
#42460=CARTESIAN_POINT('',(-38.,4.1,106.));
#42461=CARTESIAN_POINT('',(-28.8000000000002,4.1,109.1));
#42462=CARTESIAN_POINT('Origin',(-38.,4.15,105.95));
#42463=CARTESIAN_POINT('',(37.95,4.15,105.95));
#42464=CARTESIAN_POINT('',(37.9,4.2,106.));
#42465=CARTESIAN_POINT('',(24.7375000000004,17.3625000000003,119.1625));
#42466=CARTESIAN_POINT('',(25.8,4.2,106.));
#42467=CARTESIAN_POINT('',(-38.,4.2,106.));
#42468=CARTESIAN_POINT('',(25.8,0.974999999999829,102.775));
#42469=CARTESIAN_POINT('',(24.9666666666671,-8.83333333333357,92.9666666666671));
#42470=CARTESIAN_POINT('Origin',(37.95,7.475,105.95));
#42471=CARTESIAN_POINT('',(38.,4.2,105.9));
#42472=CARTESIAN_POINT('',(38.,4.2,105.9));
#42473=CARTESIAN_POINT('',(38.,8.5,105.9));
#42474=CARTESIAN_POINT('',(38.,7.475,105.9));
#42475=CARTESIAN_POINT('',(37.95,8.55,105.95));
#42476=CARTESIAN_POINT('',(38.5041666666667,7.99583333333331,105.395833333333));
#42477=CARTESIAN_POINT('',(37.9,8.5,106.));
#42478=CARTESIAN_POINT('',(25.1125000000004,-4.28750000000023,118.7875));
#42479=CARTESIAN_POINT('',(37.9,7.475,106.));
#42480=CARTESIAN_POINT('Origin',(37.95,4.15,104.));
#42481=CARTESIAN_POINT('',(37.95,4.15,98.05));
#42482=CARTESIAN_POINT('',(24.3000000000005,-9.50000000000025,111.7));
#42483=CARTESIAN_POINT('',(38.,4.2,98.1));
#42484=CARTESIAN_POINT('',(38.,4.2,98.1));
#42485=CARTESIAN_POINT('',(38.,4.2,104.));
#42486=CARTESIAN_POINT('Origin',(-38.,8.55,98.05));
#42487=CARTESIAN_POINT('',(37.95,8.55000000000001,98.05));
#42488=CARTESIAN_POINT('',(24.9666666666671,21.5333333333336,111.033333333333));
#42489=CARTESIAN_POINT('',(37.9,8.5,98.));
#42490=CARTESIAN_POINT('',(24.7375000000004,-4.66250000000027,84.8375000000004));
#42491=CARTESIAN_POINT('',(25.8,8.5,98.));
#42492=CARTESIAN_POINT('',(-38.,8.5,98.));
#42493=CARTESIAN_POINT('',(25.8,8.5,98.));
#42494=CARTESIAN_POINT('Origin',(25.75,8.55,97.5));
#42495=CARTESIAN_POINT('',(25.8,8.5,97.15));
#42496=CARTESIAN_POINT('',(25.8,8.5,97.5));
#42497=CARTESIAN_POINT('',(25.75,8.55,97.1));
#42498=CARTESIAN_POINT('',(27.9499999999999,6.35000000000002,99.3000000000001));
#42499=CARTESIAN_POINT('',(18.2333333333337,16.0666666666664,104.616666666667));
#42500=CARTESIAN_POINT('Origin',(37.95,8.55,100.));
#42501=CARTESIAN_POINT('',(38.,8.5,98.5));
#42502=CARTESIAN_POINT('',(37.8875,8.61249999999999,98.6125));
#42503=CARTESIAN_POINT('',(38.,8.5,98.1));
#42504=CARTESIAN_POINT('',(38.,8.5,100.));
#42505=CARTESIAN_POINT('',(38.8291666666667,7.67083333333329,98.9291666666667));
#42506=CARTESIAN_POINT('Origin',(-19.,8.525,97.075));
#42507=CARTESIAN_POINT('',(25.65,8.45,97.));
#42508=CARTESIAN_POINT('',(25.65,8.45,97.));
#42509=CARTESIAN_POINT('',(-25.65,8.45,97.));
#42510=CARTESIAN_POINT('',(-19.,8.45,97.));
#42511=CARTESIAN_POINT('',(-25.75,8.55,97.1));
#42512=CARTESIAN_POINT('',(-25.8,8.6,97.15));
#42513=CARTESIAN_POINT('',(-24.5666666666667,9.73333333333331,98.2833333333334));
#42514=CARTESIAN_POINT('Origin',(25.75,-4.3,97.95));
#42515=CARTESIAN_POINT('',(25.7,-4.1,98.));
#42516=CARTESIAN_POINT('',(25.8,-4.1,97.9));
#42517=CARTESIAN_POINT('',(9.79999999999887,-4.1,113.9));
#42518=CARTESIAN_POINT('',(25.8,-4.3,97.9));
#42519=CARTESIAN_POINT('',(25.7,-4.3,98.));
#42520=CARTESIAN_POINT('Origin',(25.8,-8.6,97.));
#42521=CARTESIAN_POINT('',(25.8,4.2,98.));
#42522=CARTESIAN_POINT('',(25.8,-2.25,98.));
#42523=CARTESIAN_POINT('',(25.8,1.22499999999983,100.975));
#42524=CARTESIAN_POINT('',(25.8,-4.1,98.1));
#42525=CARTESIAN_POINT('',(25.8,-4.1,97.5));
#42526=CARTESIAN_POINT('',(25.8,-4.2,98.));
#42527=CARTESIAN_POINT('',(25.8,-5.52500000000006,96.675));
#42528=CARTESIAN_POINT('',(25.8,-8.5,98.));
#42529=CARTESIAN_POINT('',(25.8,-8.6,98.));
#42530=CARTESIAN_POINT('',(25.8,-8.5,97.15));
#42531=CARTESIAN_POINT('',(25.8,-8.5,97.8));
#42532=CARTESIAN_POINT('',(25.8,-4.3,97.15));
#42533=CARTESIAN_POINT('Origin',(-38.,4.15,98.05));
#42534=CARTESIAN_POINT('',(37.9,4.2,98.));
#42535=CARTESIAN_POINT('',(-38.,4.2,98.));
#42536=CARTESIAN_POINT('',(25.1125000000005,16.9875000000002,85.2125000000004));
#42537=CARTESIAN_POINT('Origin',(37.95,5.225,98.05));
#42538=CARTESIAN_POINT('',(38.,5.225,98.1));
#42539=CARTESIAN_POINT('',(37.9,5.225,98.));
#42540=CARTESIAN_POINT('Origin',(37.95,5.525,105.45));
#42541=CARTESIAN_POINT('',(38.,8.5,105.5));
#42542=CARTESIAN_POINT('',(38.1625,8.33749999999997,105.6625));
#42543=CARTESIAN_POINT('',(38.,4.6,105.5));
#42544=CARTESIAN_POINT('',(38.,5.525,105.5));
#42545=CARTESIAN_POINT('',(38.,4.6,105.5));
#42546=CARTESIAN_POINT('Origin',(37.95,4.65,100.3));
#42547=CARTESIAN_POINT('',(38.,4.6,98.5));
#42548=CARTESIAN_POINT('',(38.,4.6,100.3));
#42549=CARTESIAN_POINT('',(38.,4.6,98.5));
#42550=CARTESIAN_POINT('Origin',(37.95,7.475,98.55));
#42551=CARTESIAN_POINT('',(38.,7.475,98.5));
#42552=CARTESIAN_POINT('Origin',(38.,6.35,102.));
#42553=CARTESIAN_POINT('',(38.,8.5,103.7));
#42554=CARTESIAN_POINT('Origin',(37.95,8.55,103.7));
#42555=CARTESIAN_POINT('',(37.9,8.6,105.9));
#42556=CARTESIAN_POINT('',(37.9,8.6,103.7));
#42557=CARTESIAN_POINT('',(24.9166666666671,21.5833333333336,92.9166666666671));
#42558=CARTESIAN_POINT('Origin',(-38.,4.1,98.));
#42559=CARTESIAN_POINT('Origin',(-38.,8.6,106.));
#42560=CARTESIAN_POINT('',(25.8,8.5,106.));
#42561=CARTESIAN_POINT('',(-38.,8.5,106.));
#42562=CARTESIAN_POINT('',(25.8,0.,106.));
#42563=CARTESIAN_POINT('Origin',(-38.,8.55,105.95));
#42564=CARTESIAN_POINT('',(25.7,8.6,105.9));
#42565=CARTESIAN_POINT('',(-38.,8.6,105.9));
#42566=CARTESIAN_POINT('',(25.7,8.6,105.9));
#42567=CARTESIAN_POINT('Origin',(-38.,8.6,105.4));
#42568=CARTESIAN_POINT('',(-37.9,8.6,105.9));
#42569=CARTESIAN_POINT('',(-37.9,8.6,103.7));
#42570=CARTESIAN_POINT('',(-25.7,8.6,105.9));
#42571=CARTESIAN_POINT('',(-38.,8.6,105.9));
#42572=CARTESIAN_POINT('',(-25.7,8.6,106.85));
#42573=CARTESIAN_POINT('',(-25.7,8.6,105.7));
#42574=CARTESIAN_POINT('',(25.7,8.6,106.85));
#42575=CARTESIAN_POINT('',(-19.,8.6,106.85));
#42576=CARTESIAN_POINT('',(25.7,8.6,105.7));
#42577=CARTESIAN_POINT('Origin',(25.75,8.55,105.7));
#42578=CARTESIAN_POINT('',(18.1000000000004,16.1999999999998,99.2499999999999));
#42579=CARTESIAN_POINT('',(25.8,8.5,105.7));
#42580=CARTESIAN_POINT('Origin',(-19.,8.525,106.925));
#42581=CARTESIAN_POINT('',(-24.4333333333333,9.86666666666665,105.583333333333));
#42582=CARTESIAN_POINT('',(-19.,8.45,107.));
#42583=CARTESIAN_POINT('Origin',(-25.75,8.55,105.7));
#42584=CARTESIAN_POINT('',(-25.7,8.6,105.9));
#42585=CARTESIAN_POINT('Origin',(-38.,8.55,105.95));
#42586=CARTESIAN_POINT('',(-37.5833333333333,8.91666666666667,105.583333333333));
#42587=CARTESIAN_POINT('',(-38.,8.5,106.));
#42588=CARTESIAN_POINT('Origin',(-38.,8.6,106.));
#42589=CARTESIAN_POINT('Origin',(-25.75,8.55,97.5));
#42590=CARTESIAN_POINT('',(-25.8,8.5,97.15));
#42591=CARTESIAN_POINT('',(-26.5166666666666,7.78333333333337,97.8666666666667));
#42592=CARTESIAN_POINT('',(-25.8,8.5,97.5));
#42593=CARTESIAN_POINT('Origin',(-25.75,4.3,97.95));
#42594=CARTESIAN_POINT('',(-25.8,-4.1,97.9));
#42595=CARTESIAN_POINT('',(-25.8,4.3,97.9));
#42596=CARTESIAN_POINT('',(-25.7,-4.1,98.));
#42597=CARTESIAN_POINT('',(-28.8000000000002,-4.1,94.9));
#42598=CARTESIAN_POINT('',(-25.7,4.3,98.));
#42599=CARTESIAN_POINT('Origin',(-25.8,8.6,97.));
#42600=CARTESIAN_POINT('',(-25.8,-8.5,97.15));
#42601=CARTESIAN_POINT('',(-25.8,4.3,97.15));
#42602=CARTESIAN_POINT('',(-25.8,-8.5,98.));
#42603=CARTESIAN_POINT('',(-25.8,-8.5,97.8));
#42604=CARTESIAN_POINT('',(-25.8,-4.2,98.));
#42605=CARTESIAN_POINT('',(-25.8,0.,98.));
#42606=CARTESIAN_POINT('',(-25.8,-4.1,98.1));
#42607=CARTESIAN_POINT('',(-25.8,-1.22499999999983,100.975));
#42608=CARTESIAN_POINT('',(-25.8,-4.1,97.5));
#42609=CARTESIAN_POINT('',(-25.8,6.35,98.));
#42610=CARTESIAN_POINT('Origin',(25.75,-4.3,106.05));
#42611=CARTESIAN_POINT('',(25.8,-4.1,106.1));
#42612=CARTESIAN_POINT('',(25.8,-4.3,106.1));
#42613=CARTESIAN_POINT('',(25.7,-4.1,106.));
#42614=CARTESIAN_POINT('',(7.79999999999887,-4.1,88.1000000000002));
#42615=CARTESIAN_POINT('',(25.7,-4.3,106.));
#42616=CARTESIAN_POINT('Origin',(0.,0.,106.));
#42617=CARTESIAN_POINT('',(-25.7,-4.1,106.));
#42618=CARTESIAN_POINT('',(-38.,-4.1,106.));
#42619=CARTESIAN_POINT('',(-25.7,4.3,106.));
#42620=CARTESIAN_POINT('',(-19.105,7.40911313484149E-17,106.));
#42621=CARTESIAN_POINT('Origin',(-18.5,0.,106.));
#42622=CARTESIAN_POINT('',(17.895,7.40911313484149E-17,106.));
#42623=CARTESIAN_POINT('Origin',(18.5,0.,106.));
#42624=CARTESIAN_POINT('Origin',(-38.,-4.15,105.95));
#42625=CARTESIAN_POINT('',(37.95,-4.15,105.95));
#42626=CARTESIAN_POINT('',(37.9,-4.1,105.9));
#42627=CARTESIAN_POINT('',(24.3000000000005,9.50000000000025,92.3000000000005));
#42628=CARTESIAN_POINT('',(25.8,-4.1,105.9));
#42629=CARTESIAN_POINT('',(-38.,-4.1,105.9));
#42630=CARTESIAN_POINT('',(25.8,-4.2,106.));
#42631=CARTESIAN_POINT('',(25.8,-5.27500000000006,107.075));
#42632=CARTESIAN_POINT('',(37.9,-4.2,106.));
#42633=CARTESIAN_POINT('',(-38.,-4.2,106.));
#42634=CARTESIAN_POINT('',(25.1125000000005,-16.9875000000002,118.7875));
#42635=CARTESIAN_POINT('Origin',(-38.,-4.1,98.));
#42636=CARTESIAN_POINT('',(25.8,-4.1,102.));
#42637=CARTESIAN_POINT('',(37.9,-4.1,98.1));
#42638=CARTESIAN_POINT('',(37.9,-4.1,100.));
#42639=CARTESIAN_POINT('',(-38.,-4.1,98.1));
#42640=CARTESIAN_POINT('',(-38.,-4.1,98.));
#42641=CARTESIAN_POINT('',(-37.9,-4.1,98.1));
#42642=CARTESIAN_POINT('',(-38.,-4.1,98.1));
#42643=CARTESIAN_POINT('',(-37.9,-4.1,105.9));
#42644=CARTESIAN_POINT('',(-37.9,-4.1,100.));
#42645=CARTESIAN_POINT('',(-38.,-4.1,105.9));
#42646=CARTESIAN_POINT('',(-26.8000000000002,-4.1,107.1));
#42647=CARTESIAN_POINT('Origin',(37.95,-4.15,100.));
#42648=CARTESIAN_POINT('',(38.,-4.2,105.9));
#42649=CARTESIAN_POINT('',(38.,-4.2,105.9));
#42650=CARTESIAN_POINT('',(38.,-4.2,98.1));
#42651=CARTESIAN_POINT('',(38.,-4.2,100.));
#42652=CARTESIAN_POINT('',(38.,-4.2,98.1));
#42653=CARTESIAN_POINT('Origin',(37.95,-5.225,105.95));
#42654=CARTESIAN_POINT('',(38.,-5.225,105.9));
#42655=CARTESIAN_POINT('',(37.9,-5.225,106.));
#42656=CARTESIAN_POINT('Origin',(-37.95,8.55,103.7));
#42657=CARTESIAN_POINT('Origin',(-25.75,4.3,106.05));
#42658=CARTESIAN_POINT('Origin',(-37.95,-4.15,100.));
#42659=CARTESIAN_POINT('',(-38.,-4.2,106.));
#42660=CARTESIAN_POINT('',(-37.95,-4.15,98.05));
#42661=CARTESIAN_POINT('',(-37.6333333333333,-3.83333333333334,98.3666666666666));
#42662=CARTESIAN_POINT('',(-38.8291666666667,-5.02916666666667,98.9291666666666));
#42663=CARTESIAN_POINT('Origin',(-38.,-4.15,105.95));
#42664=CARTESIAN_POINT('Origin',(-38.,-4.15,98.05));
#42665=CARTESIAN_POINT('',(-37.9,-4.2,98.));
#42666=CARTESIAN_POINT('',(-38.,-4.2,98.));
#42667=CARTESIAN_POINT('',(-38.,-4.1,98.1));
#42668=CARTESIAN_POINT('Origin',(37.95,-5.525,98.55));
#42669=CARTESIAN_POINT('',(38.,-8.5,98.5));
#42670=CARTESIAN_POINT('',(38.1625,-8.33749999999997,98.3375));
#42671=CARTESIAN_POINT('',(38.,-4.6,98.5));
#42672=CARTESIAN_POINT('',(38.,-5.525,98.5));
#42673=CARTESIAN_POINT('',(38.,-4.6,98.5));
#42674=CARTESIAN_POINT('Origin',(37.95,-4.65,103.7));
#42675=CARTESIAN_POINT('',(38.,-4.6,103.7));
#42676=CARTESIAN_POINT('Origin',(38.,-6.35,102.));
#42677=CARTESIAN_POINT('',(38.,-8.5,98.1));
#42678=CARTESIAN_POINT('',(38.,-8.5,100.3));
#42679=CARTESIAN_POINT('',(38.,-7.475,98.1));
#42680=CARTESIAN_POINT('Origin',(37.95,-8.55,100.3));
#42681=CARTESIAN_POINT('',(37.9,-8.6,98.1));
#42682=CARTESIAN_POINT('',(37.9,-8.6,100.3));
#42683=CARTESIAN_POINT('',(37.95,-8.55,98.05));
#42684=CARTESIAN_POINT('',(24.9166666666671,-21.5833333333336,111.083333333333));
#42685=CARTESIAN_POINT('',(38.5041666666667,-7.99583333333331,98.6041666666667));
#42686=CARTESIAN_POINT('Origin',(37.9,-4.1,98.1));
#42687=CARTESIAN_POINT('',(37.9,-4.2,98.));
#42688=CARTESIAN_POINT('',(37.9,-4.2,98.));
#42689=CARTESIAN_POINT('',(37.9,-4.1,98.1));
#42690=CARTESIAN_POINT('Origin',(-38.,-4.15,98.05));
#42691=CARTESIAN_POINT('',(-38.,-4.2,98.));
#42692=CARTESIAN_POINT('Origin',(37.95,-7.475,98.05));
#42693=CARTESIAN_POINT('',(37.9,-8.5,98.));
#42694=CARTESIAN_POINT('',(25.1125000000004,4.28750000000023,85.2125000000004));
#42695=CARTESIAN_POINT('',(37.9,-7.475,98.));
#42696=CARTESIAN_POINT('Origin',(-38.,-8.6,98.));
#42697=CARTESIAN_POINT('',(-38.,-8.5,98.));
#42698=CARTESIAN_POINT('Origin',(-38.,-8.55,98.05));
#42699=CARTESIAN_POINT('',(25.7,-8.6,98.1));
#42700=CARTESIAN_POINT('',(-38.,-8.6,98.1));
#42701=CARTESIAN_POINT('',(25.7,-8.6,98.1));
#42702=CARTESIAN_POINT('Origin',(-37.95,-7.475,98.05));
#42703=CARTESIAN_POINT('',(-37.9,-8.5,98.));
#42704=CARTESIAN_POINT('',(-37.9,-7.475,98.));
#42705=CARTESIAN_POINT('',(-37.95,-8.55,98.05));
#42706=CARTESIAN_POINT('',(-37.7791666666667,-8.37916666666666,97.8791666666667));
#42707=CARTESIAN_POINT('',(-38.5041666666667,-7.99583333333334,98.6041666666666));
#42708=CARTESIAN_POINT('Origin',(-38.,-8.55,98.05));
#42709=CARTESIAN_POINT('',(-38.,-8.5,98.));
#42710=CARTESIAN_POINT('',(-25.7,-8.6,98.1));
#42711=CARTESIAN_POINT('',(-25.7,-8.6,98.1));
#42712=CARTESIAN_POINT('',(-37.9,-8.6,98.1));
#42713=CARTESIAN_POINT('',(-38.,-8.6,98.1));
#42714=CARTESIAN_POINT('',(-37.5833333333333,-8.91666666666666,98.4166666666666));
#42715=CARTESIAN_POINT('Origin',(-38.,-8.6,98.));
#42716=CARTESIAN_POINT('Origin',(-38.,-8.6,98.6));
#42717=CARTESIAN_POINT('',(-37.9,-8.6,100.3));
#42718=CARTESIAN_POINT('',(-25.7,-8.6,97.15));
#42719=CARTESIAN_POINT('',(-25.7,-8.6,97.8));
#42720=CARTESIAN_POINT('',(25.7,-8.6,97.15));
#42721=CARTESIAN_POINT('',(-19.,-8.6,97.15));
#42722=CARTESIAN_POINT('',(25.7,-8.6,97.8));
#42723=CARTESIAN_POINT('Origin',(25.75,-8.55,97.8));
#42724=CARTESIAN_POINT('',(25.75,-8.55,97.1));
#42725=CARTESIAN_POINT('',(18.1833333333337,-16.1166666666664,104.666666666667));
#42726=CARTESIAN_POINT('',(26.5666666666666,-7.73333333333334,97.9166666666667));
#42727=CARTESIAN_POINT('Origin',(25.725,-4.3,97.075));
#42728=CARTESIAN_POINT('',(25.65,-8.45,97.));
#42729=CARTESIAN_POINT('',(25.65,-8.45,97.));
#42730=CARTESIAN_POINT('',(25.65,-4.3,97.));
#42731=CARTESIAN_POINT('Origin',(-19.,-8.525,97.075));
#42732=CARTESIAN_POINT('',(-25.75,-8.55,97.1));
#42733=CARTESIAN_POINT('',(-24.5166666666667,-9.7833333333333,98.3333333333333));
#42734=CARTESIAN_POINT('',(-25.65,-8.45,97.));
#42735=CARTESIAN_POINT('',(-25.65,-8.45,97.));
#42736=CARTESIAN_POINT('',(-19.,-8.45,97.));
#42737=CARTESIAN_POINT('Origin',(-25.75,-8.55,97.8));
#42738=CARTESIAN_POINT('',(-27.9999999999999,-6.30000000000002,99.3500000000001));
#42739=CARTESIAN_POINT('Origin',(-25.725,4.3,97.075));
#42740=CARTESIAN_POINT('',(-25.65,4.3,97.));
#42741=CARTESIAN_POINT('Origin',(-37.95,-8.55,100.3));
#42742=CARTESIAN_POINT('Origin',(0.,-7.4375534806121E-17,91.2146446609407));
#42743=CARTESIAN_POINT('',(2.5,-3.06161699786838E-16,91.3));
#42744=CARTESIAN_POINT('',(-2.5,-3.06161699786838E-16,91.3));
#42745=CARTESIAN_POINT('Origin',(0.,0.,91.3));
#42746=CARTESIAN_POINT('Origin',(0.,0.,91.3));
#42747=CARTESIAN_POINT('',(2.42928932188135,2.97502139224484E-16,91.1292893218813));
#42748=CARTESIAN_POINT('',(2.46464466094067,3.01831919505661E-16,91.2146446609407));
#42749=CARTESIAN_POINT('',(-2.42928932188135,-2.97502139224484E-16,91.1292893218813));
#42750=CARTESIAN_POINT('Origin',(0.,-1.48751069612242E-16,91.1292893218813));
#42751=CARTESIAN_POINT('Origin',(0.,-1.48751069612242E-16,91.1292893218813));
#42752=CARTESIAN_POINT('Origin',(0.,0.,91.1));
#42753=CARTESIAN_POINT('',(-2.37071067811866,-2.90328324366247E-16,91.0707106781187));
#42754=CARTESIAN_POINT('',(-2.4,-2.93915231795365E-16,91.1));
#42755=CARTESIAN_POINT('',(2.37071067811866,-2.90328324366247E-16,91.0707106781187));
#42756=CARTESIAN_POINT('Origin',(0.,-1.45164162183123E-16,91.0707106781187));
#42757=CARTESIAN_POINT('Origin',(0.,-1.45164162183123E-16,91.0707106781187));
#42758=CARTESIAN_POINT('Origin',(0.,0.,93.95));
#42759=CARTESIAN_POINT('',(-2.5,-3.06161699786838E-16,96.7));
#42760=CARTESIAN_POINT('Origin',(0.,0.,96.7));
#42761=CARTESIAN_POINT('',(-2.5,-3.06161699786838E-16,93.95));
#42762=CARTESIAN_POINT('Origin',(0.,-7.25820810915617E-17,91.0353553390593));
#42763=CARTESIAN_POINT('',(2.2,2.69422295812418E-16,91.));
#42764=CARTESIAN_POINT('',(2.28535533905933,2.79875310089332E-16,91.0353553390593));
#42765=CARTESIAN_POINT('Origin',(0.,0.,91.));
#42766=CARTESIAN_POINT('Origin',(2.3,0.,91.));
#42767=CARTESIAN_POINT('Origin',(18.5,0.,106.05));
#42768=CARTESIAN_POINT('',(17.995,-6.18446633569412E-17,106.1));
#42769=CARTESIAN_POINT('',(17.945,6.79678973526781E-17,106.05));
#42770=CARTESIAN_POINT('Origin',(18.5,0.,106.1));
#42771=CARTESIAN_POINT('Origin',(18.5,0.,106.));
#42772=CARTESIAN_POINT('',(17.995,6.18446633569412E-17,106.9));
#42773=CARTESIAN_POINT('',(17.995,-6.18446633569412E-17,106.));
#42774=CARTESIAN_POINT('Origin',(18.5,0.,106.9));
#42775=CARTESIAN_POINT('Origin',(18.5,0.,106.95));
#42776=CARTESIAN_POINT('',(17.895,-7.40911313484149E-17,107.));
#42777=CARTESIAN_POINT('Origin',(18.5,0.,107.));
#42778=CARTESIAN_POINT('',(17.945,-6.79678973526781E-17,106.95));
#42779=CARTESIAN_POINT('Origin',(0.,0.,107.));
#42780=CARTESIAN_POINT('',(-19.105,-7.40911313484149E-17,107.));
#42781=CARTESIAN_POINT('Origin',(-18.5,0.,107.));
#42782=CARTESIAN_POINT('Origin',(-18.5,0.,106.05));
#42783=CARTESIAN_POINT('',(-19.005,-6.18446633569412E-17,106.1));
#42784=CARTESIAN_POINT('',(-19.055,6.79678973526781E-17,106.05));
#42785=CARTESIAN_POINT('Origin',(-18.5,0.,106.1));
#42786=CARTESIAN_POINT('Origin',(-18.5,0.,106.));
#42787=CARTESIAN_POINT('',(-19.005,6.18446633569412E-17,106.9));
#42788=CARTESIAN_POINT('',(-19.005,-6.18446633569412E-17,106.));
#42789=CARTESIAN_POINT('Origin',(-18.5,0.,106.9));
#42790=CARTESIAN_POINT('Origin',(-18.5,0.,106.95));
#42791=CARTESIAN_POINT('',(-19.055,-6.79678973526781E-17,106.95));
#42792=CARTESIAN_POINT('Origin',(0.,0.,96.875));
#42793=CARTESIAN_POINT('',(-2.75714285714286,-3.37652617479199E-16,97.));
#42794=CARTESIAN_POINT('Origin',(0.,0.,97.));
#42795=CARTESIAN_POINT('',(-2.65,-3.24531401774049E-16,96.875));
#42796=CARTESIAN_POINT('Origin',(-38.,-8.6,105.4));
#42797=CARTESIAN_POINT('Origin',(-38.,4.1,98.));
#42798=CARTESIAN_POINT('Origin',(0.,0.,97.));
#42799=CARTESIAN_POINT('Origin',(0.,0.,98.));
#42800=CARTESIAN_POINT('Origin',(25.8,-8.6,106.));
#42801=CARTESIAN_POINT('',(25.8,-6.35,106.));
#42802=CARTESIAN_POINT('Origin',(-38.,-4.1,106.));
#42803=CARTESIAN_POINT('',(0.,0.,0.));
#42804=CARTESIAN_POINT('Origin',(34.55,2.05,77.05));
#42805=CARTESIAN_POINT('',(34.5,4.1,77.1));
#42806=CARTESIAN_POINT('',(34.6,4.1,77.));
#42807=CARTESIAN_POINT('',(14.175,4.1,97.425));
#42808=CARTESIAN_POINT('',(34.6,-4.1,77.));
#42809=CARTESIAN_POINT('',(34.6,2.05,77.));
#42810=CARTESIAN_POINT('',(34.5,-4.1,77.1));
#42811=CARTESIAN_POINT('',(16.675,-4.1,94.925));
#42812=CARTESIAN_POINT('',(34.5,2.05,77.1));
#42813=CARTESIAN_POINT('Origin',(36.25,0.,77.));
#42814=CARTESIAN_POINT('',(37.9,4.1,77.));
#42815=CARTESIAN_POINT('',(-0.875,4.1,77.));
#42816=CARTESIAN_POINT('',(37.9,-4.1,77.));
#42817=CARTESIAN_POINT('',(37.9,3.3,77.));
#42818=CARTESIAN_POINT('',(-0.875,-4.1,77.));
#42819=CARTESIAN_POINT('Origin',(-38.,9.05,76.05));
#42820=CARTESIAN_POINT('',(37.95,9.05000000000001,76.05));
#42821=CARTESIAN_POINT('',(37.9,9.,76.));
#42822=CARTESIAN_POINT('',(24.6750000000004,-4.22500000000027,62.7750000000004));
#42823=CARTESIAN_POINT('',(-37.9,9.,76.));
#42824=CARTESIAN_POINT('',(-38.,9.,76.));
#42825=CARTESIAN_POINT('',(-37.95,9.05000000000001,76.05));
#42826=CARTESIAN_POINT('',(-36.2416666666666,7.34166666666655,74.3416666666666));
#42827=CARTESIAN_POINT('',(-37.9,9.1,76.1));
#42828=CARTESIAN_POINT('',(-37.55,9.45000000000001,76.45));
#42829=CARTESIAN_POINT('',(37.9,9.1,76.1));
#42830=CARTESIAN_POINT('',(-38.,9.1,76.1));
#42831=CARTESIAN_POINT('',(24.8833333333338,22.1166666666669,89.1166666666662));
#42832=CARTESIAN_POINT('Origin',(-38.,9.1,76.));
#42833=CARTESIAN_POINT('',(-37.9,9.1,76.5));
#42834=CARTESIAN_POINT('',(-37.9,9.1,78.5));
#42835=CARTESIAN_POINT('',(37.9,9.1,76.5));
#42836=CARTESIAN_POINT('',(-38.,9.1,76.5));
#42837=CARTESIAN_POINT('',(37.9,9.1,78.5));
#42838=CARTESIAN_POINT('Origin',(-37.95,9.05,78.5));
#42839=CARTESIAN_POINT('',(-38.,9.,76.1));
#42840=CARTESIAN_POINT('',(-40.075,6.92499999999987,78.175));
#42841=CARTESIAN_POINT('',(-38.,9.,76.5));
#42842=CARTESIAN_POINT('',(-38.,9.,78.5));
#42843=CARTESIAN_POINT('',(-37.95,9.04999999999999,76.55));
#42844=CARTESIAN_POINT('',(-38.925,8.07499999999991,75.575));
#42845=CARTESIAN_POINT('',(-38.2833333333333,8.71666666666666,76.8833333333333));
#42846=CARTESIAN_POINT('Origin',(-37.95,-1.25,76.05));
#42847=CARTESIAN_POINT('',(-37.9,4.2,76.));
#42848=CARTESIAN_POINT('',(-37.9,-1.25,76.));
#42849=CARTESIAN_POINT('',(-37.95,4.15,76.05));
#42850=CARTESIAN_POINT('',(-38.8583333333333,3.2416666666666,76.9583333333333));
#42851=CARTESIAN_POINT('',(-38.,4.2,76.1));
#42852=CARTESIAN_POINT('',(-38.,4.2,76.1));
#42853=CARTESIAN_POINT('',(-38.,-1.25,76.1));
#42854=CARTESIAN_POINT('Origin',(34.55,2.05,84.95));
#42855=CARTESIAN_POINT('',(34.6,4.1,85.));
#42856=CARTESIAN_POINT('',(34.5,4.1,84.9));
#42857=CARTESIAN_POINT('',(16.6749999999987,4.1,67.075));
#42858=CARTESIAN_POINT('',(34.5,-4.1,84.9));
#42859=CARTESIAN_POINT('',(34.5,2.05,84.9));
#42860=CARTESIAN_POINT('',(34.6,-4.1,85.));
#42861=CARTESIAN_POINT('',(14.1749999999987,-4.1,64.5750000000002));
#42862=CARTESIAN_POINT('',(34.6,2.05,85.));
#42863=CARTESIAN_POINT('Origin',(34.5,4.1,77.));
#42864=CARTESIAN_POINT('',(34.5,-4.1,76.5));
#42865=CARTESIAN_POINT('',(34.5,4.1,81.5));
#42866=CARTESIAN_POINT('Origin',(-34.55,-2.05,77.05));
#42867=CARTESIAN_POINT('',(-34.5,-4.1,77.1));
#42868=CARTESIAN_POINT('',(-34.6,-4.1,77.));
#42869=CARTESIAN_POINT('',(-35.675,-4.1,75.925));
#42870=CARTESIAN_POINT('',(-34.6,4.1,77.));
#42871=CARTESIAN_POINT('',(-34.6,-2.05,77.));
#42872=CARTESIAN_POINT('',(-34.5,4.1,77.1));
#42873=CARTESIAN_POINT('',(-33.175,4.1,78.425));
#42874=CARTESIAN_POINT('',(-34.5,-2.05,77.1));
#42875=CARTESIAN_POINT('Origin',(-36.25,0.,77.));
#42876=CARTESIAN_POINT('',(-37.9,-4.1,77.));
#42877=CARTESIAN_POINT('',(-37.125,-4.1,77.));
#42878=CARTESIAN_POINT('',(-37.9,4.1,77.));
#42879=CARTESIAN_POINT('',(-37.9,-3.3,77.));
#42880=CARTESIAN_POINT('',(-37.125,4.1,77.));
#42881=CARTESIAN_POINT('Origin',(-38.,-9.05,76.55));
#42882=CARTESIAN_POINT('',(37.95,-9.05,76.55));
#42883=CARTESIAN_POINT('',(37.9,-9.,76.6));
#42884=CARTESIAN_POINT('',(23.6250000000004,5.27500000000034,90.8749999999996));
#42885=CARTESIAN_POINT('',(-37.9,-9.,76.6));
#42886=CARTESIAN_POINT('',(-38.,-9.,76.6));
#42887=CARTESIAN_POINT('',(-37.95,-9.05,76.55));
#42888=CARTESIAN_POINT('',(-37.3916666666667,-8.49166666666665,77.1083333333333));
#42889=CARTESIAN_POINT('',(-37.9,-9.1,76.5));
#42890=CARTESIAN_POINT('',(-38.3333333333333,-8.66666666666668,76.9333333333333));
#42891=CARTESIAN_POINT('',(37.9,-9.1,76.5));
#42892=CARTESIAN_POINT('',(-38.,-9.1,76.5));
#42893=CARTESIAN_POINT('',(25.6666666666671,-21.3333333333336,64.2666666666671));
#42894=CARTESIAN_POINT('Origin',(37.95,-9.05,78.8));
#42895=CARTESIAN_POINT('',(37.9,-9.1,76.1));
#42896=CARTESIAN_POINT('',(37.9,-9.1,78.8));
#42897=CARTESIAN_POINT('',(37.95,-9.05,76.05));
#42898=CARTESIAN_POINT('',(24.8333333333338,-22.1666666666669,89.1666666666662));
#42899=CARTESIAN_POINT('',(38.,-9.,76.1));
#42900=CARTESIAN_POINT('',(39.7083333333333,-7.29166666666657,77.8083333333333));
#42901=CARTESIAN_POINT('',(38.,-9.,76.5));
#42902=CARTESIAN_POINT('',(38.,-9.,78.8));
#42903=CARTESIAN_POINT('',(39.2416666666667,-7.75833333333322,75.2583333333333));
#42904=CARTESIAN_POINT('Origin',(-38.,-9.1,76.6));
#42905=CARTESIAN_POINT('',(-37.9,-9.1,76.1));
#42906=CARTESIAN_POINT('',(-37.9,-9.1,78.8));
#42907=CARTESIAN_POINT('',(-38.,-9.1,76.1));
#42908=CARTESIAN_POINT('Origin',(-37.95,-9.05,78.8));
#42909=CARTESIAN_POINT('',(-38.,-9.,76.5));
#42910=CARTESIAN_POINT('',(-38.1416666666667,-8.85833333333331,76.3583333333333));
#42911=CARTESIAN_POINT('',(-38.,-9.,76.1));
#42912=CARTESIAN_POINT('',(-38.,-9.,78.8));
#42913=CARTESIAN_POINT('',(-37.95,-9.05000000000001,76.05));
#42914=CARTESIAN_POINT('',(-38.6083333333333,-8.39166666666668,76.7083333333333));
#42915=CARTESIAN_POINT('',(-37.5,-9.49999999999999,76.5));
#42916=CARTESIAN_POINT('Origin',(-38.,-9.05,76.05));
#42917=CARTESIAN_POINT('',(-37.9,-9.,76.));
#42918=CARTESIAN_POINT('',(-37.7583333333333,-8.85833333333333,75.8583333333333));
#42919=CARTESIAN_POINT('',(37.9,-9.,76.));
#42920=CARTESIAN_POINT('',(-38.,-9.,76.));
#42921=CARTESIAN_POINT('',(23.9916666666671,4.90833333333365,62.0916666666671));
#42922=CARTESIAN_POINT('Origin',(37.95,-1.25,76.05));
#42923=CARTESIAN_POINT('',(37.9,-4.2,76.));
#42924=CARTESIAN_POINT('',(37.9,-1.25,76.));
#42925=CARTESIAN_POINT('',(38.,-4.2,76.1));
#42926=CARTESIAN_POINT('',(37.9,-4.2,76.));
#42927=CARTESIAN_POINT('',(38.,-1.25,76.1));
#42928=CARTESIAN_POINT('Origin',(-38.,-9.1,76.));
#42929=CARTESIAN_POINT('',(-37.9,-4.2,76.));
#42930=CARTESIAN_POINT('',(-37.9,-7.85,76.));
#42931=CARTESIAN_POINT('',(-38.,-4.2,76.));
#42932=CARTESIAN_POINT('Origin',(-37.95,-7.85,76.05));
#42933=CARTESIAN_POINT('',(-38.,-4.2,76.1));
#42934=CARTESIAN_POINT('',(-38.,-7.85,76.1));
#42935=CARTESIAN_POINT('',(-37.95,-4.15,76.05));
#42936=CARTESIAN_POINT('',(-38.,-4.2,76.1));
#42937=CARTESIAN_POINT('',(-37.3416666666666,-4.75833333333335,75.4416666666667));
#42938=CARTESIAN_POINT('Origin',(37.95,0.95,76.55));
#42939=CARTESIAN_POINT('',(38.,-4.6,76.5));
#42940=CARTESIAN_POINT('',(38.,0.95,76.5));
#42941=CARTESIAN_POINT('',(37.9,-4.7,76.6));
#42942=CARTESIAN_POINT('',(38.,-4.6,76.5));
#42943=CARTESIAN_POINT('',(37.9,0.95,76.6));
#42944=CARTESIAN_POINT('Origin',(37.95,-4.65,83.2));
#42945=CARTESIAN_POINT('',(38.,-4.6,85.5));
#42946=CARTESIAN_POINT('',(38.,-4.6,83.2));
#42947=CARTESIAN_POINT('',(37.9,-4.7,85.4));
#42948=CARTESIAN_POINT('',(38.1416666666667,-4.45833333333329,85.6416666666667));
#42949=CARTESIAN_POINT('',(37.9,-4.7,83.2));
#42950=CARTESIAN_POINT('Origin',(-38.,-4.7,76.6));
#42951=CARTESIAN_POINT('',(-37.9,-4.7,76.6));
#42952=CARTESIAN_POINT('',(-38.,-4.7,76.6));
#42953=CARTESIAN_POINT('',(-37.9,-5.65,76.6));
#42954=CARTESIAN_POINT('Origin',(-38.,-4.7,85.4));
#42955=CARTESIAN_POINT('',(-37.9,-4.7,85.4));
#42956=CARTESIAN_POINT('',(-38.,-4.7,85.4));
#42957=CARTESIAN_POINT('',(-37.9,-4.7,83.2));
#42958=CARTESIAN_POINT('Origin',(-34.55,-2.05,84.95));
#42959=CARTESIAN_POINT('',(-34.6,-4.1,85.));
#42960=CARTESIAN_POINT('',(-34.5,-4.1,84.9));
#42961=CARTESIAN_POINT('',(-33.1750000000001,-4.1,83.5750000000002));
#42962=CARTESIAN_POINT('',(-34.5,4.1,84.9));
#42963=CARTESIAN_POINT('',(-34.5,-2.05,84.9));
#42964=CARTESIAN_POINT('',(-34.6,4.1,85.));
#42965=CARTESIAN_POINT('',(-35.6750000000001,4.1,86.075));
#42966=CARTESIAN_POINT('',(-34.6,-2.05,85.));
#42967=CARTESIAN_POINT('Origin',(-34.5,-4.1,77.));
#42968=CARTESIAN_POINT('',(-34.5,4.1,81.5));
#42969=CARTESIAN_POINT('',(-34.5,-4.1,76.5));
#42970=CARTESIAN_POINT('Origin',(37.9,-4.1,76.1));
#42971=CARTESIAN_POINT('',(37.9,-4.1,76.1));
#42972=CARTESIAN_POINT('',(37.9,-4.1,76.1));
#42973=CARTESIAN_POINT('',(38.,-4.2,76.1));
#42974=CARTESIAN_POINT('Origin',(-38.,-4.15,76.05));
#42975=CARTESIAN_POINT('',(-37.9,-4.1,76.1));
#42976=CARTESIAN_POINT('',(-37.55,-3.75000000000001,76.45));
#42977=CARTESIAN_POINT('',(-38.,-4.1,76.1));
#42978=CARTESIAN_POINT('Origin',(37.9,4.2,76.));
#42979=CARTESIAN_POINT('',(37.9,4.1,76.1));
#42980=CARTESIAN_POINT('',(38.,4.2,76.1));
#42981=CARTESIAN_POINT('',(37.9,4.1,76.1));
#42982=CARTESIAN_POINT('',(37.9,4.2,76.));
#42983=CARTESIAN_POINT('',(37.9,4.2,76.));
#42984=CARTESIAN_POINT('',(38.,4.2,76.1));
#42985=CARTESIAN_POINT('Origin',(-38.,4.15,76.05));
#42986=CARTESIAN_POINT('',(-38.,4.2,76.));
#42987=CARTESIAN_POINT('',(-37.9,4.1,76.1));
#42988=CARTESIAN_POINT('',(-38.,4.1,76.1));
#42989=CARTESIAN_POINT('',(-36.7166666666667,2.91666666666664,77.2833333333333));
#42990=CARTESIAN_POINT('Origin',(37.95,5.35,76.05));
#42991=CARTESIAN_POINT('',(38.,9.,76.1));
#42992=CARTESIAN_POINT('',(38.975,8.02499999999995,77.075));
#42993=CARTESIAN_POINT('',(38.,5.35,76.1));
#42994=CARTESIAN_POINT('',(37.9,5.35,76.));
#42995=CARTESIAN_POINT('Origin',(37.95,4.15,83.5));
#42996=CARTESIAN_POINT('',(37.9,4.1,83.5));
#42997=CARTESIAN_POINT('',(38.,4.2,77.1));
#42998=CARTESIAN_POINT('',(38.,4.2,83.5));
#42999=CARTESIAN_POINT('',(38.,4.2,77.1));
#43000=CARTESIAN_POINT('Origin',(37.95,3.3,77.05));
#43001=CARTESIAN_POINT('',(38.,-4.2,77.1));
#43002=CARTESIAN_POINT('',(38.,3.3,77.1));
#43003=CARTESIAN_POINT('',(38.,-4.2,77.1));
#43004=CARTESIAN_POINT('Origin',(37.95,-4.15,78.5));
#43005=CARTESIAN_POINT('',(38.,-4.2,78.5));
#43006=CARTESIAN_POINT('',(37.9,-4.1,78.5));
#43007=CARTESIAN_POINT('Origin',(-37.95,-4.15,78.5));
#43008=CARTESIAN_POINT('',(-38.,-4.2,77.1));
#43009=CARTESIAN_POINT('',(-38.,-4.2,78.5));
#43010=CARTESIAN_POINT('',(-38.,-4.2,77.1));
#43011=CARTESIAN_POINT('',(-37.9,-4.1,78.5));
#43012=CARTESIAN_POINT('Origin',(38.,6.6,81.));
#43013=CARTESIAN_POINT('',(38.,9.,76.5));
#43014=CARTESIAN_POINT('',(38.,9.,78.5));
#43015=CARTESIAN_POINT('',(38.,4.6,76.5));
#43016=CARTESIAN_POINT('',(38.,7.85,76.5));
#43017=CARTESIAN_POINT('',(38.,4.6,85.5));
#43018=CARTESIAN_POINT('',(38.,4.6,78.8));
#43019=CARTESIAN_POINT('',(38.,9.,85.5));
#43020=CARTESIAN_POINT('',(38.,5.65,85.5));
#43021=CARTESIAN_POINT('',(38.,9.,85.9));
#43022=CARTESIAN_POINT('',(38.,9.,83.2));
#43023=CARTESIAN_POINT('',(38.,4.2,85.9));
#43024=CARTESIAN_POINT('',(38.,7.85,85.9));
#43025=CARTESIAN_POINT('',(38.,4.2,84.9));
#43026=CARTESIAN_POINT('',(38.,4.2,83.5));
#43027=CARTESIAN_POINT('',(38.,-4.2,84.9));
#43028=CARTESIAN_POINT('',(38.,3.3,84.9));
#43029=CARTESIAN_POINT('',(38.,-4.2,85.9));
#43030=CARTESIAN_POINT('',(38.,-4.2,78.5));
#43031=CARTESIAN_POINT('',(38.,-9.,85.9));
#43032=CARTESIAN_POINT('',(38.,1.25,85.9));
#43033=CARTESIAN_POINT('',(38.,-9.,85.5));
#43034=CARTESIAN_POINT('',(38.,-9.,83.5));
#43035=CARTESIAN_POINT('',(38.,-1.25,85.5));
#43036=CARTESIAN_POINT('Origin',(-38.,9.05,76.55));
#43037=CARTESIAN_POINT('',(37.95,9.04999999999999,76.55));
#43038=CARTESIAN_POINT('',(25.6166666666671,21.3833333333336,64.2166666666671));
#43039=CARTESIAN_POINT('',(-37.9,9.,76.6));
#43040=CARTESIAN_POINT('',(-36.6583333333333,7.75833333333324,77.8416666666667));
#43041=CARTESIAN_POINT('',(37.9,9.,76.6));
#43042=CARTESIAN_POINT('',(-38.,9.,76.6));
#43043=CARTESIAN_POINT('',(25.0916666666671,-3.80833333333358,89.4083333333329));
#43044=CARTESIAN_POINT('Origin',(37.95,7.85,76.55));
#43045=CARTESIAN_POINT('',(37.9,4.7,76.6));
#43046=CARTESIAN_POINT('',(37.9,7.85,76.6));
#43047=CARTESIAN_POINT('',(38.,4.6,76.5));
#43048=CARTESIAN_POINT('',(37.825,9.17499999999999,76.675));
#43049=CARTESIAN_POINT('Origin',(-38.,9.1,76.6));
#43050=CARTESIAN_POINT('',(-37.9,4.7,76.6));
#43051=CARTESIAN_POINT('',(-37.9,1.25,76.6));
#43052=CARTESIAN_POINT('',(-38.,4.7,76.6));
#43053=CARTESIAN_POINT('Origin',(-37.95,1.25,76.55));
#43054=CARTESIAN_POINT('',(-38.,4.6,76.5));
#43055=CARTESIAN_POINT('',(-38.,1.25,76.5));
#43056=CARTESIAN_POINT('',(-38.,4.6,76.5));
#43057=CARTESIAN_POINT('Origin',(37.95,4.65,78.8));
#43058=CARTESIAN_POINT('',(37.9,4.7,85.4));
#43059=CARTESIAN_POINT('',(37.9,4.7,78.8));
#43060=CARTESIAN_POINT('',(36.675,5.92500000000003,84.175));
#43061=CARTESIAN_POINT('Origin',(37.95,-4.15,78.5));
#43062=CARTESIAN_POINT('',(37.9,-4.1,85.));
#43063=CARTESIAN_POINT('',(37.9,-4.1,85.9));
#43064=CARTESIAN_POINT('',(37.9,-4.1,78.5));
#43065=CARTESIAN_POINT('',(37.95,-4.15,85.95));
#43066=CARTESIAN_POINT('',(24.0500000000005,9.75000000000025,72.0500000000005));
#43067=CARTESIAN_POINT('',(38.2916666666666,-4.49166666666663,85.6083333333334));
#43068=CARTESIAN_POINT('',(38.,-4.2,84.9));
#43069=CARTESIAN_POINT('Origin',(37.95,3.3,84.95));
#43070=CARTESIAN_POINT('',(37.9,4.1,85.));
#43071=CARTESIAN_POINT('',(38.,4.2,84.9));
#43072=CARTESIAN_POINT('',(37.9,3.3,85.));
#43073=CARTESIAN_POINT('Origin',(37.9,4.1,85.9));
#43074=CARTESIAN_POINT('',(37.9,4.2,86.));
#43075=CARTESIAN_POINT('',(37.9,4.2,86.));
#43076=CARTESIAN_POINT('',(37.9,4.1,85.9));
#43077=CARTESIAN_POINT('',(37.9,4.1,85.9));
#43078=CARTESIAN_POINT('',(38.,4.2,85.9));
#43079=CARTESIAN_POINT('Origin',(-38.,4.15,85.95));
#43080=CARTESIAN_POINT('',(-37.95,4.15,85.95));
#43081=CARTESIAN_POINT('',(-37.9,4.1,85.9));
#43082=CARTESIAN_POINT('',(-37.55,3.74999999999999,85.55));
#43083=CARTESIAN_POINT('',(-38.,4.1,85.9));
#43084=CARTESIAN_POINT('',(-37.9,4.2,86.));
#43085=CARTESIAN_POINT('',(-38.,4.2,86.));
#43086=CARTESIAN_POINT('',(-38.4416666666667,3.6583333333333,85.4583333333333));
#43087=CARTESIAN_POINT('Origin',(37.95,4.15,83.5));
#43088=CARTESIAN_POINT('',(37.9,4.1,83.5));
#43089=CARTESIAN_POINT('Origin',(37.95,7.85,85.95));
#43090=CARTESIAN_POINT('',(37.95,9.05000000000001,85.95));
#43091=CARTESIAN_POINT('',(37.9,9.,86.));
#43092=CARTESIAN_POINT('',(25.0916666666671,-3.80833333333357,98.8083333333329));
#43093=CARTESIAN_POINT('',(37.9,7.85,86.));
#43094=CARTESIAN_POINT('',(38.6083333333333,8.39166666666664,85.2916666666667));
#43095=CARTESIAN_POINT('Origin',(36.25,0.,85.));
#43096=CARTESIAN_POINT('',(-0.875,-4.1,85.));
#43097=CARTESIAN_POINT('',(-0.875,4.1,85.));
#43098=CARTESIAN_POINT('Origin',(-38.,4.1,86.));
#43099=CARTESIAN_POINT('',(-37.9,4.1,85.));
#43100=CARTESIAN_POINT('',(-37.9,4.1,83.5));
#43101=CARTESIAN_POINT('',(-37.125,4.1,85.));
#43102=CARTESIAN_POINT('',(-37.9,4.1,83.5));
#43103=CARTESIAN_POINT('Origin',(-37.95,4.15,83.5));
#43104=CARTESIAN_POINT('',(-38.,4.2,85.9));
#43105=CARTESIAN_POINT('',(-38.,4.2,85.9));
#43106=CARTESIAN_POINT('',(-38.,4.2,84.9));
#43107=CARTESIAN_POINT('',(-38.,4.2,83.5));
#43108=CARTESIAN_POINT('',(-38.,4.2,84.9));
#43109=CARTESIAN_POINT('Origin',(-37.95,1.25,85.95));
#43110=CARTESIAN_POINT('',(-37.9,9.,86.));
#43111=CARTESIAN_POINT('',(-37.9,1.25,86.));
#43112=CARTESIAN_POINT('',(-37.95,9.05,85.95));
#43113=CARTESIAN_POINT('',(-36.6583333333333,7.75833333333324,87.2416666666667));
#43114=CARTESIAN_POINT('',(-38.,9.,85.9));
#43115=CARTESIAN_POINT('',(-39.7083333333333,7.29166666666657,84.1916666666667));
#43116=CARTESIAN_POINT('',(-38.,1.25,85.9));
#43117=CARTESIAN_POINT('Origin',(-38.,9.1,86.));
#43118=CARTESIAN_POINT('',(-38.,9.,86.));
#43119=CARTESIAN_POINT('',(-6.,6.1,86.));
#43120=CARTESIAN_POINT('',(6.,6.1,86.));
#43121=CARTESIAN_POINT('',(-16.,6.1,86.));
#43122=CARTESIAN_POINT('',(-6.,7.7,86.));
#43123=CARTESIAN_POINT('Origin',(-6.,6.9,86.));
#43124=CARTESIAN_POINT('',(6.,7.7,86.));
#43125=CARTESIAN_POINT('',(-22.,7.7,86.));
#43126=CARTESIAN_POINT('Origin',(6.,6.9,86.));
#43127=CARTESIAN_POINT('Origin',(-38.,9.05,85.95));
#43128=CARTESIAN_POINT('',(37.9,9.1,85.9));
#43129=CARTESIAN_POINT('',(24.8333333333338,22.1666666666669,72.8333333333338));
#43130=CARTESIAN_POINT('',(-37.9,9.1,85.9));
#43131=CARTESIAN_POINT('',(-38.,9.1,85.9));
#43132=CARTESIAN_POINT('',(-37.5,9.50000000000001,85.5));
#43133=CARTESIAN_POINT('Origin',(-37.95,9.05,83.2));
#43134=CARTESIAN_POINT('',(-37.9,9.1,85.5));
#43135=CARTESIAN_POINT('',(-37.9,9.1,83.2));
#43136=CARTESIAN_POINT('',(-37.95,9.05,85.45));
#43137=CARTESIAN_POINT('',(-38.3333333333333,8.66666666666666,85.0666666666667));
#43138=CARTESIAN_POINT('',(-38.,9.,85.5));
#43139=CARTESIAN_POINT('',(-39.2416666666667,7.75833333333322,86.7416666666667));
#43140=CARTESIAN_POINT('',(-38.,9.,83.2));
#43141=CARTESIAN_POINT('Origin',(-38.,9.05,85.45));
#43142=CARTESIAN_POINT('',(37.95,9.05,85.45));
#43143=CARTESIAN_POINT('',(37.9,9.,85.4));
#43144=CARTESIAN_POINT('',(24.7250000000004,-4.17500000000027,72.2250000000004));
#43145=CARTESIAN_POINT('',(-37.9,9.,85.4));
#43146=CARTESIAN_POINT('',(-38.,9.,85.4));
#43147=CARTESIAN_POINT('',(-36.2916666666666,7.39166666666655,83.7916666666666));
#43148=CARTESIAN_POINT('',(37.9,9.1,85.5));
#43149=CARTESIAN_POINT('',(-38.,9.1,85.5));
#43150=CARTESIAN_POINT('',(25.6666666666671,21.3333333333336,97.7333333333329));
#43151=CARTESIAN_POINT('Origin',(-37.95,-0.95,85.45));
#43152=CARTESIAN_POINT('',(-37.9,4.7,85.4));
#43153=CARTESIAN_POINT('',(-37.9,-0.95,85.4));
#43154=CARTESIAN_POINT('',(-38.,4.6,85.5));
#43155=CARTESIAN_POINT('',(-38.,4.6,85.5));
#43156=CARTESIAN_POINT('',(-38.,-0.95,85.5));
#43157=CARTESIAN_POINT('Origin',(-38.,4.7,85.4));
#43158=CARTESIAN_POINT('',(37.9,5.65,85.4));
#43159=CARTESIAN_POINT('',(-38.,4.7,85.4));
#43160=CARTESIAN_POINT('',(6.,6.1,85.4));
#43161=CARTESIAN_POINT('',(-6.,6.1,85.4));
#43162=CARTESIAN_POINT('',(-16.,6.1,85.4));
#43163=CARTESIAN_POINT('',(6.,7.7,85.4));
#43164=CARTESIAN_POINT('Origin',(6.,6.9,85.4));
#43165=CARTESIAN_POINT('',(-6.,7.7,85.4));
#43166=CARTESIAN_POINT('',(-22.,7.7,85.4));
#43167=CARTESIAN_POINT('Origin',(-6.,6.9,85.4));
#43168=CARTESIAN_POINT('Origin',(37.95,5.65,85.45));
#43169=CARTESIAN_POINT('',(38.1416666666667,8.8583333333333,85.6416666666667));
#43170=CARTESIAN_POINT('Origin',(37.95,9.05,83.2));
#43171=CARTESIAN_POINT('',(37.9,9.1,83.2));
#43172=CARTESIAN_POINT('Origin',(-37.95,-3.3,77.05));
#43173=CARTESIAN_POINT('',(-38.,4.2,77.1));
#43174=CARTESIAN_POINT('',(-38.,-3.3,77.1));
#43175=CARTESIAN_POINT('',(-38.,4.2,77.1));
#43176=CARTESIAN_POINT('Origin',(-37.95,4.15,83.5));
#43177=CARTESIAN_POINT('',(-38.,4.2,83.5));
#43178=CARTESIAN_POINT('Origin',(-38.,-6.6,81.));
#43179=CARTESIAN_POINT('',(-38.,-4.6,76.5));
#43180=CARTESIAN_POINT('',(-38.,-5.65,76.5));
#43181=CARTESIAN_POINT('',(-38.,-4.6,85.5));
#43182=CARTESIAN_POINT('',(-38.,-4.6,83.2));
#43183=CARTESIAN_POINT('',(-38.,-9.,85.5));
#43184=CARTESIAN_POINT('',(-38.,-7.85,85.5));
#43185=CARTESIAN_POINT('',(-38.,-9.,85.9));
#43186=CARTESIAN_POINT('',(-38.,-9.,83.5));
#43187=CARTESIAN_POINT('',(-38.,-4.2,85.9));
#43188=CARTESIAN_POINT('',(-38.,-5.35,85.9));
#43189=CARTESIAN_POINT('',(-38.,-4.2,84.9));
#43190=CARTESIAN_POINT('',(-38.,-4.2,78.5));
#43191=CARTESIAN_POINT('',(-38.,-3.3,84.9));
#43192=CARTESIAN_POINT('',(-38.,4.6,78.8));
#43193=CARTESIAN_POINT('Origin',(-37.95,4.65,78.8));
#43194=CARTESIAN_POINT('',(-37.9,4.7,78.8));
#43195=CARTESIAN_POINT('Origin',(-38.,4.7,76.6));
#43196=CARTESIAN_POINT('Origin',(-38.,-4.2,85.9));
#43197=CARTESIAN_POINT('',(-37.9,-4.1,85.9));
#43198=CARTESIAN_POINT('',(-37.9,-4.2,86.));
#43199=CARTESIAN_POINT('',(-37.9,-4.1,85.9));
#43200=CARTESIAN_POINT('',(-38.,-4.2,85.9));
#43201=CARTESIAN_POINT('',(-37.9,-4.2,86.));
#43202=CARTESIAN_POINT('Origin',(-37.95,-4.15,78.5));
#43203=CARTESIAN_POINT('',(-37.9,-4.1,85.));
#43204=CARTESIAN_POINT('',(-37.9,-4.1,78.5));
#43205=CARTESIAN_POINT('',(-37.9,-4.1,85.));
#43206=CARTESIAN_POINT('Origin',(-37.95,-5.35,85.95));
#43207=CARTESIAN_POINT('',(-37.95,-9.05,85.95));
#43208=CARTESIAN_POINT('',(-37.9,-9.,86.));
#43209=CARTESIAN_POINT('',(-37.3416666666666,-8.44166666666665,86.5583333333333));
#43210=CARTESIAN_POINT('',(-37.9,-5.35,86.));
#43211=CARTESIAN_POINT('',(-38.975,-8.025,84.925));
#43212=CARTESIAN_POINT('Origin',(-38.,-4.15,85.95));
#43213=CARTESIAN_POINT('',(-38.,-4.1,85.9));
#43214=CARTESIAN_POINT('',(37.9,-4.2,86.));
#43215=CARTESIAN_POINT('',(-38.,-4.2,86.));
#43216=CARTESIAN_POINT('',(37.9,-4.2,86.));
#43217=CARTESIAN_POINT('Origin',(-37.95,-3.3,84.95));
#43218=CARTESIAN_POINT('',(-37.9,-3.3,85.));
#43219=CARTESIAN_POINT('Origin',(37.95,1.25,85.95));
#43220=CARTESIAN_POINT('',(37.9,-9.,86.));
#43221=CARTESIAN_POINT('',(37.9,1.25,86.));
#43222=CARTESIAN_POINT('',(37.95,-9.05,85.95));
#43223=CARTESIAN_POINT('',(23.5750000000004,5.32500000000035,100.325));
#43224=CARTESIAN_POINT('',(40.075,-6.92499999999987,83.825));
#43225=CARTESIAN_POINT('Origin',(-36.25,0.,85.));
#43226=CARTESIAN_POINT('',(-37.125,-4.1,85.));
#43227=CARTESIAN_POINT('Origin',(-38.,-4.1,76.));
#43228=CARTESIAN_POINT('Origin',(37.95,-9.05,83.5));
#43229=CARTESIAN_POINT('',(37.9,-9.1,85.9));
#43230=CARTESIAN_POINT('',(24.8833333333338,-22.1166666666669,72.8833333333338));
#43231=CARTESIAN_POINT('',(37.9,-9.1,85.5));
#43232=CARTESIAN_POINT('',(37.9,-9.1,83.5));
#43233=CARTESIAN_POINT('',(37.95,-9.05,85.45));
#43234=CARTESIAN_POINT('',(25.6166666666671,-21.3833333333336,97.7833333333329));
#43235=CARTESIAN_POINT('',(38.925,-8.07499999999991,86.425));
#43236=CARTESIAN_POINT('Origin',(-37.95,-4.65,83.2));
#43237=CARTESIAN_POINT('',(-37.0416666666667,-5.55833333333334,84.5416666666667));
#43238=CARTESIAN_POINT('',(-38.,-4.6,76.5));
#43239=CARTESIAN_POINT('Origin',(-37.95,-5.65,76.55));
#43240=CARTESIAN_POINT('Origin',(37.95,-1.25,85.45));
#43241=CARTESIAN_POINT('',(37.9,-9.,85.4));
#43242=CARTESIAN_POINT('',(23.9916666666671,4.90833333333365,71.4916666666671));
#43243=CARTESIAN_POINT('',(37.9,-1.25,85.4));
#43244=CARTESIAN_POINT('Origin',(-38.,-9.1,85.4));
#43245=CARTESIAN_POINT('',(-37.9,-9.,85.4));
#43246=CARTESIAN_POINT('',(-38.,-9.,85.4));
#43247=CARTESIAN_POINT('',(-37.9,-7.85,85.4));
#43248=CARTESIAN_POINT('',(6.,-7.7,85.4));
#43249=CARTESIAN_POINT('',(-6.,-7.7,85.4));
#43250=CARTESIAN_POINT('',(-16.,-7.7,85.4));
#43251=CARTESIAN_POINT('',(6.,-6.1,85.4));
#43252=CARTESIAN_POINT('Origin',(6.,-6.9,85.4));
#43253=CARTESIAN_POINT('',(-6.,-6.1,85.4));
#43254=CARTESIAN_POINT('',(-22.,-6.1,85.4));
#43255=CARTESIAN_POINT('Origin',(-6.,-6.9,85.4));
#43256=CARTESIAN_POINT('Origin',(-38.,-9.05,85.45));
#43257=CARTESIAN_POINT('',(-37.9,-9.1,85.5));
#43258=CARTESIAN_POINT('',(-38.,-9.1,85.5));
#43259=CARTESIAN_POINT('',(-37.95,-9.05,85.45));
#43260=CARTESIAN_POINT('',(-38.2833333333333,-8.71666666666668,85.1166666666667));
#43261=CARTESIAN_POINT('',(-37.7583333333333,-8.85833333333333,85.2583333333333));
#43262=CARTESIAN_POINT('Origin',(-37.95,-7.85,85.45));
#43263=CARTESIAN_POINT('',(-37.825,-9.17499999999998,85.325));
#43264=CARTESIAN_POINT('Origin',(-37.95,-9.05,83.5));
#43265=CARTESIAN_POINT('',(-37.9,-9.1,85.9));
#43266=CARTESIAN_POINT('',(-37.9,-9.1,83.5));
#43267=CARTESIAN_POINT('',(-37.55,-9.44999999999999,85.55));
#43268=CARTESIAN_POINT('Origin',(-38.,-9.05,85.95));
#43269=CARTESIAN_POINT('',(-38.,-9.1,85.9));
#43270=CARTESIAN_POINT('',(-38.,-9.,86.));
#43271=CARTESIAN_POINT('Origin',(-38.,-4.1,86.));
#43272=CARTESIAN_POINT('',(-6.,-7.7,86.));
#43273=CARTESIAN_POINT('',(6.,-7.7,86.));
#43274=CARTESIAN_POINT('',(-16.,-7.7,86.));
#43275=CARTESIAN_POINT('',(-6.,-6.1,86.));
#43276=CARTESIAN_POINT('Origin',(-6.,-6.9,86.));
#43277=CARTESIAN_POINT('',(6.,-6.1,86.));
#43278=CARTESIAN_POINT('',(-22.,-6.1,86.));
#43279=CARTESIAN_POINT('Origin',(6.,-6.9,86.));
#43280=CARTESIAN_POINT('Origin',(-16.,6.15,85.45));
#43281=CARTESIAN_POINT('',(6.,6.2,85.5));
#43282=CARTESIAN_POINT('',(6.,6.2,85.5));
#43283=CARTESIAN_POINT('',(-6.,6.2,85.5));
#43284=CARTESIAN_POINT('',(-6.,6.1,85.4));
#43285=CARTESIAN_POINT('',(-16.,6.2,85.5));
#43286=CARTESIAN_POINT('Origin',(6.,6.9,85.45));
#43287=CARTESIAN_POINT('',(6.,7.6,85.5));
#43288=CARTESIAN_POINT('',(6.,7.6,85.5));
#43289=CARTESIAN_POINT('Origin',(6.,6.9,85.5));
#43290=CARTESIAN_POINT('Origin',(-22.,7.65,85.45));
#43291=CARTESIAN_POINT('',(-6.,7.6,85.5));
#43292=CARTESIAN_POINT('',(-6.,7.6,85.5));
#43293=CARTESIAN_POINT('',(-22.,7.6,85.5));
#43294=CARTESIAN_POINT('Origin',(-6.,6.9,85.45));
#43295=CARTESIAN_POINT('Origin',(-6.,6.9,85.5));
#43296=CARTESIAN_POINT('Origin',(6.,6.9,86.));
#43297=CARTESIAN_POINT('',(6.,6.2,85.9));
#43298=CARTESIAN_POINT('',(6.,6.2,86.));
#43299=CARTESIAN_POINT('',(6.,7.6,85.9));
#43300=CARTESIAN_POINT('Origin',(6.,6.9,85.9));
#43301=CARTESIAN_POINT('',(6.,7.6,86.));
#43302=CARTESIAN_POINT('Origin',(6.,6.2,86.));
#43303=CARTESIAN_POINT('',(-6.,6.2,85.9));
#43304=CARTESIAN_POINT('',(-6.,6.2,86.));
#43305=CARTESIAN_POINT('',(-16.,6.2,85.9));
#43306=CARTESIAN_POINT('Origin',(-16.,6.15,85.95));
#43307=CARTESIAN_POINT('',(-6.,6.2,85.9));
#43308=CARTESIAN_POINT('',(6.,6.1,86.));
#43309=CARTESIAN_POINT('Origin',(-6.,6.9,85.95));
#43310=CARTESIAN_POINT('',(-6.,7.6,85.9));
#43311=CARTESIAN_POINT('',(-6.,7.6,85.9));
#43312=CARTESIAN_POINT('Origin',(-6.,6.9,85.9));
#43313=CARTESIAN_POINT('Origin',(-22.,7.65,85.95));
#43314=CARTESIAN_POINT('',(6.,7.6,85.9));
#43315=CARTESIAN_POINT('',(-22.,7.6,85.9));
#43316=CARTESIAN_POINT('Origin',(6.,6.9,85.95));
#43317=CARTESIAN_POINT('Origin',(-6.,6.9,86.));
#43318=CARTESIAN_POINT('',(-6.,7.6,86.));
#43319=CARTESIAN_POINT('Origin',(-16.,-7.65,85.45));
#43320=CARTESIAN_POINT('',(6.,-7.6,85.5));
#43321=CARTESIAN_POINT('',(6.,-7.6,85.5));
#43322=CARTESIAN_POINT('',(-6.,-7.6,85.5));
#43323=CARTESIAN_POINT('',(-6.,-7.7,85.4));
#43324=CARTESIAN_POINT('',(-16.,-7.6,85.5));
#43325=CARTESIAN_POINT('Origin',(6.,-6.9,85.45));
#43326=CARTESIAN_POINT('',(6.,-6.2,85.5));
#43327=CARTESIAN_POINT('',(6.,-6.2,85.5));
#43328=CARTESIAN_POINT('Origin',(6.,-6.9,85.5));
#43329=CARTESIAN_POINT('Origin',(-22.,-6.15,85.45));
#43330=CARTESIAN_POINT('',(-6.,-6.2,85.5));
#43331=CARTESIAN_POINT('',(-6.,-6.2,85.5));
#43332=CARTESIAN_POINT('',(-22.,-6.2,85.5));
#43333=CARTESIAN_POINT('Origin',(-6.,-6.9,85.45));
#43334=CARTESIAN_POINT('Origin',(-6.,-6.9,85.5));
#43335=CARTESIAN_POINT('Origin',(6.,-6.9,86.));
#43336=CARTESIAN_POINT('',(6.,-7.6,85.9));
#43337=CARTESIAN_POINT('',(6.,-7.6,86.));
#43338=CARTESIAN_POINT('',(6.,-6.2,85.9));
#43339=CARTESIAN_POINT('Origin',(6.,-6.9,85.9));
#43340=CARTESIAN_POINT('',(6.,-6.2,86.));
#43341=CARTESIAN_POINT('Origin',(6.,-7.6,86.));
#43342=CARTESIAN_POINT('',(-6.,-7.6,85.9));
#43343=CARTESIAN_POINT('',(-6.,-7.6,86.));
#43344=CARTESIAN_POINT('',(-16.,-7.6,85.9));
#43345=CARTESIAN_POINT('Origin',(-16.,-7.65,85.95));
#43346=CARTESIAN_POINT('',(-6.,-7.6,85.9));
#43347=CARTESIAN_POINT('',(6.,-7.7,86.));
#43348=CARTESIAN_POINT('Origin',(-6.,-6.9,85.95));
#43349=CARTESIAN_POINT('',(-6.,-6.2,85.9));
#43350=CARTESIAN_POINT('',(-6.,-6.2,85.9));
#43351=CARTESIAN_POINT('Origin',(-6.,-6.9,85.9));
#43352=CARTESIAN_POINT('Origin',(-22.,-6.15,85.95));
#43353=CARTESIAN_POINT('',(6.,-6.2,85.9));
#43354=CARTESIAN_POINT('',(-22.,-6.2,85.9));
#43355=CARTESIAN_POINT('Origin',(6.,-6.9,85.95));
#43356=CARTESIAN_POINT('Origin',(-6.,-6.9,86.));
#43357=CARTESIAN_POINT('',(-6.,-6.2,86.));
#43358=CARTESIAN_POINT('Origin',(-6.,-6.2,86.));
#43359=CARTESIAN_POINT('Origin',(-6.,7.6,86.));
#43360=CARTESIAN_POINT('Origin',(-38.,-9.1,86.));
#43361=CARTESIAN_POINT('Origin',(37.95,9.05,78.5));
#43362=CARTESIAN_POINT('Origin',(-38.,9.1,85.4));
#43363=CARTESIAN_POINT('Origin',(-38.,4.1,76.));
#43364=CARTESIAN_POINT('',(0.,0.,0.));
#43365=CARTESIAN_POINT('Origin',(-34.,8.95,31.45));
#43366=CARTESIAN_POINT('',(33.95,8.95,31.45));
#43367=CARTESIAN_POINT('',(33.9,9.,31.4));
#43368=CARTESIAN_POINT('',(22.7583333333341,20.1416666666665,20.2583333333335));
#43369=CARTESIAN_POINT('',(-33.9,9.,31.4));
#43370=CARTESIAN_POINT('',(-34.,9.,31.4));
#43371=CARTESIAN_POINT('',(-33.95,8.95,31.45));
#43372=CARTESIAN_POINT('',(-34.0916666666667,8.80833333333333,31.5916666666667));
#43373=CARTESIAN_POINT('',(-33.9,8.9,31.5));
#43374=CARTESIAN_POINT('',(-33.7583333333333,8.75833333333332,31.6416666666667));
#43375=CARTESIAN_POINT('',(33.9,8.9,31.5));
#43376=CARTESIAN_POINT('',(-34.,8.9,31.5));
#43377=CARTESIAN_POINT('',(22.4250000000011,-2.57499999999974,42.9749999999997));
#43378=CARTESIAN_POINT('Origin',(-33.95,8.95,32.25));
#43379=CARTESIAN_POINT('',(-33.9,9.,31.1));
#43380=CARTESIAN_POINT('',(-33.9,9.,32.25));
#43381=CARTESIAN_POINT('',(-33.95,8.95,31.05));
#43382=CARTESIAN_POINT('',(-33.7583333333333,9.14166666666667,31.2416666666667));
#43383=CARTESIAN_POINT('',(-34.,8.9,31.1));
#43384=CARTESIAN_POINT('',(-33.9,9.,31.));
#43385=CARTESIAN_POINT('',(-34.,8.9,31.4));
#43386=CARTESIAN_POINT('',(-34.,8.9,32.25));
#43387=CARTESIAN_POINT('',(-34.,8.9,31.4));
#43388=CARTESIAN_POINT('Origin',(-34.,9.,31.));
#43389=CARTESIAN_POINT('',(33.9,9.,31.1));
#43390=CARTESIAN_POINT('',(33.9,9.,32.25));
#43391=CARTESIAN_POINT('',(-34.,9.,31.1));
#43392=CARTESIAN_POINT('Origin',(33.95,8.95,32.25));
#43393=CARTESIAN_POINT('',(34.,8.9,31.4));
#43394=CARTESIAN_POINT('',(34.,8.9,31.4));
#43395=CARTESIAN_POINT('',(34.,8.9,31.1));
#43396=CARTESIAN_POINT('',(34.,8.9,32.25));
#43397=CARTESIAN_POINT('',(33.95,8.95,31.05));
#43398=CARTESIAN_POINT('',(34.,8.9,31.1));
#43399=CARTESIAN_POINT('',(22.4250000000009,20.4749999999997,42.5749999999999));
#43400=CARTESIAN_POINT('Origin',(-34.,8.95,31.05));
#43401=CARTESIAN_POINT('',(33.9,8.9,31.));
#43402=CARTESIAN_POINT('',(22.0083333333343,-2.99166666666635,19.1083333333334));
#43403=CARTESIAN_POINT('',(-33.9,8.9,31.));
#43404=CARTESIAN_POINT('',(-34.,8.9,31.));
#43405=CARTESIAN_POINT('',(-33.3416666666667,8.34166666666665,30.4416666666666));
#43406=CARTESIAN_POINT('Origin',(-34.,4.45,35.95));
#43407=CARTESIAN_POINT('',(33.95,4.45,35.95));
#43408=CARTESIAN_POINT('',(33.9,4.5,35.9));
#43409=CARTESIAN_POINT('',(22.0500000000009,16.3499999999997,24.0500000000001));
#43410=CARTESIAN_POINT('',(-33.9,4.5,35.9));
#43411=CARTESIAN_POINT('',(-34.,4.5,35.9));
#43412=CARTESIAN_POINT('',(-33.95,4.45,35.95));
#43413=CARTESIAN_POINT('',(-33.3833333333333,5.01666666666669,35.3833333333333));
#43414=CARTESIAN_POINT('',(-33.9,4.4,36.));
#43415=CARTESIAN_POINT('',(-34.1333333333333,4.63333333333334,35.7666666666667));
#43416=CARTESIAN_POINT('',(33.9,4.4,36.));
#43417=CARTESIAN_POINT('',(-34.,4.4,36.));
#43418=CARTESIAN_POINT('',(22.8000000000009,-6.69999999999966,47.0999999999999));
#43419=CARTESIAN_POINT('Origin',(-33.95,5.5,35.95));
#43420=CARTESIAN_POINT('',(-34.,4.4,35.9));
#43421=CARTESIAN_POINT('',(-34.,4.4,35.9));
#43422=CARTESIAN_POINT('',(-34.,4.1,35.9));
#43423=CARTESIAN_POINT('',(-34.,5.5,35.9));
#43424=CARTESIAN_POINT('',(-33.95,4.05,35.95));
#43425=CARTESIAN_POINT('',(-34.,4.1,35.9));
#43426=CARTESIAN_POINT('',(-33.9,4.1,36.));
#43427=CARTESIAN_POINT('',(-33.7166666666667,4.28333333333336,36.1833333333334));
#43428=CARTESIAN_POINT('',(-33.9,5.5,36.));
#43429=CARTESIAN_POINT('Origin',(-33.95,4.45,32.5));
#43430=CARTESIAN_POINT('',(-33.9,4.5,31.5));
#43431=CARTESIAN_POINT('',(-33.9,4.5,32.5));
#43432=CARTESIAN_POINT('',(-34.,4.4,31.4));
#43433=CARTESIAN_POINT('',(-34.,4.4,31.4));
#43434=CARTESIAN_POINT('',(-34.,4.4,32.5));
#43435=CARTESIAN_POINT('Origin',(-34.,4.5,31.5));
#43436=CARTESIAN_POINT('',(33.9,4.5,31.5));
#43437=CARTESIAN_POINT('',(33.9,4.5,32.5));
#43438=CARTESIAN_POINT('',(-34.,4.5,31.5));
#43439=CARTESIAN_POINT('',(29.025,4.5,33.5));
#43440=CARTESIAN_POINT('Origin',(30.,4.5,33.5));
#43441=CARTESIAN_POINT('',(-30.975,4.5,33.5));
#43442=CARTESIAN_POINT('Origin',(-30.,4.5,33.5));
#43443=CARTESIAN_POINT('Origin',(-34.,4.05,31.05));
#43444=CARTESIAN_POINT('',(33.95,4.05,31.05));
#43445=CARTESIAN_POINT('',(33.9,4.,31.1));
#43446=CARTESIAN_POINT('',(22.0083333333343,-7.89166666666636,42.9916666666666));
#43447=CARTESIAN_POINT('',(-33.9,4.,31.1));
#43448=CARTESIAN_POINT('',(-34.,4.,31.1));
#43449=CARTESIAN_POINT('',(-33.95,4.05,31.05));
#43450=CARTESIAN_POINT('',(-33.3416666666667,3.44166666666664,31.6583333333334));
#43451=CARTESIAN_POINT('',(-33.9,4.1,31.));
#43452=CARTESIAN_POINT('',(-33.7583333333333,4.24166666666667,30.8583333333333));
#43453=CARTESIAN_POINT('',(33.9,4.1,31.));
#43454=CARTESIAN_POINT('',(-34.,4.1,31.));
#43455=CARTESIAN_POINT('',(22.4250000000009,15.5749999999997,19.5250000000001));
#43456=CARTESIAN_POINT('Origin',(-33.95,4.05,34.75));
#43457=CARTESIAN_POINT('',(-33.9,4.,35.9));
#43458=CARTESIAN_POINT('',(-33.9,4.,34.75));
#43459=CARTESIAN_POINT('',(-33.7583333333333,3.85833333333333,35.7583333333333));
#43460=CARTESIAN_POINT('',(-34.,4.1,31.1));
#43461=CARTESIAN_POINT('',(-34.,4.1,34.75));
#43462=CARTESIAN_POINT('',(-34.,4.1,31.1));
#43463=CARTESIAN_POINT('Origin',(-34.,4.,36.));
#43464=CARTESIAN_POINT('',(33.9,4.,35.9));
#43465=CARTESIAN_POINT('',(33.9,4.,34.75));
#43466=CARTESIAN_POINT('',(-34.,4.,35.9));
#43467=CARTESIAN_POINT('',(-30.975,4.,33.5));
#43468=CARTESIAN_POINT('Origin',(-30.,4.,33.5));
#43469=CARTESIAN_POINT('',(29.025,4.,33.5));
#43470=CARTESIAN_POINT('Origin',(30.,4.,33.5));
#43471=CARTESIAN_POINT('Origin',(33.95,4.05,34.75));
#43472=CARTESIAN_POINT('',(34.,4.1,31.1));
#43473=CARTESIAN_POINT('',(34.,4.1,31.1));
#43474=CARTESIAN_POINT('',(34.,4.1,35.9));
#43475=CARTESIAN_POINT('',(34.,4.1,34.75));
#43476=CARTESIAN_POINT('',(33.95,4.05,35.95));
#43477=CARTESIAN_POINT('',(34.,4.1,35.9));
#43478=CARTESIAN_POINT('',(22.4250000000004,-7.4750000000002,24.4250000000004));
#43479=CARTESIAN_POINT('Origin',(-34.,4.05,35.95));
#43480=CARTESIAN_POINT('',(33.9,4.1,36.));
#43481=CARTESIAN_POINT('',(22.3833333333348,15.6166666666666,47.516666666666));
#43482=CARTESIAN_POINT('',(-34.,4.1,36.));
#43483=CARTESIAN_POINT('Origin',(33.95,5.5,35.95));
#43484=CARTESIAN_POINT('',(33.9,5.5,36.));
#43485=CARTESIAN_POINT('',(34.,4.4,35.9));
#43486=CARTESIAN_POINT('',(34.,5.5,35.9));
#43487=CARTESIAN_POINT('',(34.,4.4,35.9));
#43488=CARTESIAN_POINT('Origin',(30.,4.45,33.5));
#43489=CARTESIAN_POINT('',(29.125,4.4,33.5));
#43490=CARTESIAN_POINT('',(29.075,4.45,33.5));
#43491=CARTESIAN_POINT('Origin',(30.,4.4,33.5));
#43492=CARTESIAN_POINT('Origin',(30.,0.,33.5));
#43493=CARTESIAN_POINT('',(29.125,4.1,33.5));
#43494=CARTESIAN_POINT('Origin',(30.,4.1,33.5));
#43495=CARTESIAN_POINT('',(29.125,0.,33.5));
#43496=CARTESIAN_POINT('Origin',(30.,4.05,33.5));
#43497=CARTESIAN_POINT('',(29.075,4.05,33.5));
#43498=CARTESIAN_POINT('Origin',(-30.,4.45,33.5));
#43499=CARTESIAN_POINT('',(-30.875,4.4,33.5));
#43500=CARTESIAN_POINT('',(-30.925,4.45,33.5));
#43501=CARTESIAN_POINT('Origin',(-30.,4.4,33.5));
#43502=CARTESIAN_POINT('Origin',(-30.,0.,33.5));
#43503=CARTESIAN_POINT('',(-30.875,4.1,33.5));
#43504=CARTESIAN_POINT('Origin',(-30.,4.1,33.5));
#43505=CARTESIAN_POINT('',(-30.875,0.,33.5));
#43506=CARTESIAN_POINT('Origin',(-30.,4.05,33.5));
#43507=CARTESIAN_POINT('',(-30.925,4.05,33.5));
#43508=CARTESIAN_POINT('Origin',(33.95,4.45,32.5));
#43509=CARTESIAN_POINT('',(34.,4.4,31.4));
#43510=CARTESIAN_POINT('',(34.,4.4,32.5));
#43511=CARTESIAN_POINT('',(34.,4.4,31.4));
#43512=CARTESIAN_POINT('Origin',(33.95,7.75,31.45));
#43513=CARTESIAN_POINT('',(33.9,7.75,31.5));
#43514=CARTESIAN_POINT('',(34.,7.75,31.4));
#43515=CARTESIAN_POINT('Origin',(33.95,5.25,31.05));
#43516=CARTESIAN_POINT('',(34.,5.25,31.1));
#43517=CARTESIAN_POINT('',(33.9,5.25,31.));
#43518=CARTESIAN_POINT('Origin',(-34.,4.5,36.));
#43519=CARTESIAN_POINT('Origin',(34.,6.5,33.5));
#43520=CARTESIAN_POINT('Origin',(-33.95,5.25,31.05));
#43521=CARTESIAN_POINT('',(-33.9,5.25,31.));
#43522=CARTESIAN_POINT('',(-34.,5.25,31.1));
#43523=CARTESIAN_POINT('Origin',(-33.95,7.75,31.45));
#43524=CARTESIAN_POINT('',(-34.,7.75,31.4));
#43525=CARTESIAN_POINT('',(-33.9,7.75,31.5));
#43526=CARTESIAN_POINT('Origin',(-34.,4.,31.));
#43527=CARTESIAN_POINT('Origin',(-34.,6.5,33.5));
#43528=CARTESIAN_POINT('Origin',(-34.,9.,31.5));
#43529=CARTESIAN_POINT('',(0.,0.,0.));
#43530=CARTESIAN_POINT('Origin',(-9.5,-8.5,109.464644660941));
#43531=CARTESIAN_POINT('',(-10.1,-8.5,109.5));
#43532=CARTESIAN_POINT('',(-10.2707106781187,-8.5,109.429289321881));
#43533=CARTESIAN_POINT('',(-10.1,-8.5,109.5));
#43534=CARTESIAN_POINT('',(-9.5,-9.27071067811865,109.429289321881));
#43535=CARTESIAN_POINT('Origin',(-9.5,-8.5,109.429289321881));
#43536=CARTESIAN_POINT('',(-9.5,-9.1,109.5));
#43537=CARTESIAN_POINT('',(-9.5,-9.27071067811865,109.429289321881));
#43538=CARTESIAN_POINT('Origin',(-9.5,-8.5,109.5));
#43539=CARTESIAN_POINT('Origin',(-10.1853553390593,0.8125,109.464644660941));
#43540=CARTESIAN_POINT('',(-10.1,6.,109.5));
#43541=CARTESIAN_POINT('',(-10.2707106781187,6.,109.429289321881));
#43542=CARTESIAN_POINT('',(-10.1,6.,109.5));
#43543=CARTESIAN_POINT('',(-10.2707106781187,0.8125,109.429289321881));
#43544=CARTESIAN_POINT('',(-10.1,0.8125,109.5));
#43545=CARTESIAN_POINT('Origin',(-9.5,6.,109.464644660941));
#43546=CARTESIAN_POINT('',(-9.5,6.6,109.5));
#43547=CARTESIAN_POINT('',(-9.5,6.77071067811865,109.429289321881));
#43548=CARTESIAN_POINT('',(-9.5,6.6,109.5));
#43549=CARTESIAN_POINT('Origin',(-9.5,6.,109.429289321881));
#43550=CARTESIAN_POINT('Origin',(-9.5,6.,109.5));
#43551=CARTESIAN_POINT('Origin',(2.625,6.68535533905934,109.464644660941));
#43552=CARTESIAN_POINT('',(9.5,6.60000000000001,109.5));
#43553=CARTESIAN_POINT('',(9.5,6.77071067811867,109.429289321881));
#43554=CARTESIAN_POINT('',(9.5,6.60000000000001,109.5));
#43555=CARTESIAN_POINT('',(2.625,6.77071067811866,109.429289321881));
#43556=CARTESIAN_POINT('',(2.625,6.60000000000001,109.5));
#43557=CARTESIAN_POINT('Origin',(9.5,6.,109.464644660941));
#43558=CARTESIAN_POINT('',(10.1,6.,109.5));
#43559=CARTESIAN_POINT('',(10.2707106781187,6.,109.429289321881));
#43560=CARTESIAN_POINT('',(10.1,6.,109.5));
#43561=CARTESIAN_POINT('Origin',(9.5,6.,109.429289321881));
#43562=CARTESIAN_POINT('Origin',(9.5,6.,109.5));
#43563=CARTESIAN_POINT('Origin',(10.1853553390593,-3.3125,109.464644660941));
#43564=CARTESIAN_POINT('',(10.1,-8.5,109.5));
#43565=CARTESIAN_POINT('',(10.2707106781187,-8.5,109.429289321881));
#43566=CARTESIAN_POINT('',(10.1,-8.5,109.5));
#43567=CARTESIAN_POINT('',(10.2707106781187,-3.3125,109.429289321881));
#43568=CARTESIAN_POINT('',(10.1,-3.3125,109.5));
#43569=CARTESIAN_POINT('Origin',(9.5,-8.5,109.464644660941));
#43570=CARTESIAN_POINT('',(9.5,-9.1,109.5));
#43571=CARTESIAN_POINT('',(9.5,-9.27071067811865,109.429289321881));
#43572=CARTESIAN_POINT('',(9.5,-9.1,109.5));
#43573=CARTESIAN_POINT('Origin',(9.5,-8.5,109.429289321881));
#43574=CARTESIAN_POINT('Origin',(9.5,-8.5,109.5));
#43575=CARTESIAN_POINT('Origin',(-2.625,-9.18535533905934,109.464644660941));
#43576=CARTESIAN_POINT('',(-2.625,-9.27071067811866,109.429289321881));
#43577=CARTESIAN_POINT('',(-2.625,-9.10000000000001,109.5));
#43578=CARTESIAN_POINT('Origin',(10.35,-5.375,109.35));
#43579=CARTESIAN_POINT('',(10.4292893218813,-8.5,109.270710678119));
#43580=CARTESIAN_POINT('',(10.2,-8.5,109.5));
#43581=CARTESIAN_POINT('',(10.4292893218814,6.,109.270710678119));
#43582=CARTESIAN_POINT('',(10.4292893218813,-7.4375,109.270710678119));
#43583=CARTESIAN_POINT('',(10.2,6.,109.5));
#43584=CARTESIAN_POINT('Origin',(9.5,-8.5,109.35));
#43585=CARTESIAN_POINT('',(9.5,-9.42928932188135,109.270710678119));
#43586=CARTESIAN_POINT('',(9.5,-9.2,109.5));
#43587=CARTESIAN_POINT('Origin',(9.5,-8.5,109.270710678119));
#43588=CARTESIAN_POINT('Origin',(-5.25,-9.35,109.35));
#43589=CARTESIAN_POINT('',(-9.5,-9.42928932188135,109.270710678119));
#43590=CARTESIAN_POINT('',(-9.5,-9.5,109.2));
#43591=CARTESIAN_POINT('',(-7.875,-9.42928932188135,109.270710678119));
#43592=CARTESIAN_POINT('Origin',(-9.5,-8.5,109.35));
#43593=CARTESIAN_POINT('',(-10.4292893218814,-8.5,109.270710678119));
#43594=CARTESIAN_POINT('',(-10.2,-8.5,109.5));
#43595=CARTESIAN_POINT('Origin',(-9.5,-8.5,109.270710678119));
#43596=CARTESIAN_POINT('Origin',(0.,-1.25,109.5));
#43597=CARTESIAN_POINT('',(5.4,-6.61309271539571E-16,109.5));
#43598=CARTESIAN_POINT('Origin',(0.,0.,109.5));
#43599=CARTESIAN_POINT('',(5.2,-7.2,109.5));
#43600=CARTESIAN_POINT('Origin',(7.,-7.2,109.5));
#43601=CARTESIAN_POINT('',(-9.5,1.22464679914735E-16,109.5));
#43602=CARTESIAN_POINT('Origin',(-8.5,0.,109.5));
#43603=CARTESIAN_POINT('Origin',(4.9545806272857,0.211749997425753,118.45));
#43604=CARTESIAN_POINT('',(4.99451026031136,0.23423761364175,124.9));
#43605=CARTESIAN_POINT('',(4.91465099426005,0.189262381209757,124.9));
#43606=CARTESIAN_POINT('',(4.869612960617,0.163897810114468,124.9));
#43607=CARTESIAN_POINT('',(4.91465099426005,0.189262381209757,124.5));
#43608=CARTESIAN_POINT('',(4.91465099426005,0.189262381209757,118.45));
#43609=CARTESIAN_POINT('',(4.99451026031136,0.23423761364175,124.5));
#43610=CARTESIAN_POINT('',(4.94553313233032,0.206654618909699,124.5));
#43611=CARTESIAN_POINT('',(4.99451026031136,0.23423761364175,118.45));
#43612=CARTESIAN_POINT('Origin',(4.85,0.,124.7));
#43613=CARTESIAN_POINT('',(4.91465099426005,-0.189262381209757,124.9));
#43614=CARTESIAN_POINT('Origin',(4.85,0.,124.9));
#43615=CARTESIAN_POINT('',(4.91465099426005,-0.189262381209757,124.5));
#43616=CARTESIAN_POINT('',(4.91465099426005,-0.189262381209757,118.45));
#43617=CARTESIAN_POINT('Origin',(4.85,0.,124.5));
#43618=CARTESIAN_POINT('Origin',(4.9545806272857,-0.211749997425753,118.45));
#43619=CARTESIAN_POINT('',(4.99451026031136,-0.23423761364175,124.5));
#43620=CARTESIAN_POINT('',(4.94553313233032,-0.206654618909699,124.5));
#43621=CARTESIAN_POINT('',(4.99451026031136,-0.23423761364175,124.9));
#43622=CARTESIAN_POINT('',(4.869612960617,-0.163897810114468,124.9));
#43623=CARTESIAN_POINT('',(4.99451026031136,-0.23423761364175,118.45));
#43624=CARTESIAN_POINT('Origin',(-7.875,-9.46464466094067,109.185355339059));
#43625=CARTESIAN_POINT('',(9.5,-9.5,109.1));
#43626=CARTESIAN_POINT('',(9.5,-9.5,109.1));
#43627=CARTESIAN_POINT('',(-9.5,-9.5,109.1));
#43628=CARTESIAN_POINT('',(-9.5,-9.42928932188135,109.270710678119));
#43629=CARTESIAN_POINT('',(-7.875,-9.5,109.1));
#43630=CARTESIAN_POINT('Origin',(9.5,-8.5,109.185355339059));
#43631=CARTESIAN_POINT('',(10.5,-8.5,109.1));
#43632=CARTESIAN_POINT('',(10.5,-8.5,109.1));
#43633=CARTESIAN_POINT('Origin',(9.5,-8.5,109.1));
#43634=CARTESIAN_POINT('Origin',(10.4646446609407,-7.4375,109.185355339059));
#43635=CARTESIAN_POINT('',(10.5,6.,109.1));
#43636=CARTESIAN_POINT('',(10.5,6.,109.1));
#43637=CARTESIAN_POINT('',(10.5,-7.4375,109.1));
#43638=CARTESIAN_POINT('Origin',(9.5,6.,109.185355339059));
#43639=CARTESIAN_POINT('',(9.5,7.,109.1));
#43640=CARTESIAN_POINT('',(9.5,6.92928932188134,109.270710678119));
#43641=CARTESIAN_POINT('',(9.5,7.,109.1));
#43642=CARTESIAN_POINT('Origin',(9.5,6.,109.270710678119));
#43643=CARTESIAN_POINT('Origin',(9.5,6.,109.1));
#43644=CARTESIAN_POINT('Origin',(7.875,6.96464466094067,109.185355339059));
#43645=CARTESIAN_POINT('',(-9.5,7.,109.1));
#43646=CARTESIAN_POINT('',(-9.5,6.92928932188135,109.270710678119));
#43647=CARTESIAN_POINT('',(-9.5,7.,109.1));
#43648=CARTESIAN_POINT('',(7.875,6.92928932188134,109.270710678119));
#43649=CARTESIAN_POINT('',(7.875,7.,109.1));
#43650=CARTESIAN_POINT('Origin',(-9.5,6.,109.185355339059));
#43651=CARTESIAN_POINT('',(-10.5,6.,109.1));
#43652=CARTESIAN_POINT('',(-10.4292893218813,6.,109.270710678119));
#43653=CARTESIAN_POINT('',(-10.5,6.,109.1));
#43654=CARTESIAN_POINT('Origin',(-9.5,6.,109.270710678119));
#43655=CARTESIAN_POINT('Origin',(-9.5,6.,109.1));
#43656=CARTESIAN_POINT('Origin',(-10.4646446609407,4.9375,109.185355339059));
#43657=CARTESIAN_POINT('',(-10.5,-8.5,109.1));
#43658=CARTESIAN_POINT('',(-10.5,-8.5,109.1));
#43659=CARTESIAN_POINT('',(-10.4292893218813,4.9375,109.270710678119));
#43660=CARTESIAN_POINT('',(-10.5,4.9375,109.1));
#43661=CARTESIAN_POINT('Origin',(-9.5,-8.5,109.185355339059));
#43662=CARTESIAN_POINT('Origin',(-9.5,-8.5,109.1));
#43663=CARTESIAN_POINT('Origin',(9.5,6.,107.));
#43664=CARTESIAN_POINT('',(10.5,6.,107.1));
#43665=CARTESIAN_POINT('',(10.5,6.,107.));
#43666=CARTESIAN_POINT('',(9.5,7.,107.1));
#43667=CARTESIAN_POINT('Origin',(9.5,6.,107.1));
#43668=CARTESIAN_POINT('',(9.5,7.,107.));
#43669=CARTESIAN_POINT('Origin',(10.5,-9.5,107.));
#43670=CARTESIAN_POINT('',(10.5,-8.5,107.1));
#43671=CARTESIAN_POINT('',(10.5,-8.5,107.));
#43672=CARTESIAN_POINT('',(10.5,-5.375,107.1));
#43673=CARTESIAN_POINT('Origin',(9.5,-8.5,107.));
#43674=CARTESIAN_POINT('',(9.5,-9.5,107.1));
#43675=CARTESIAN_POINT('',(9.5,-9.5,107.));
#43676=CARTESIAN_POINT('Origin',(9.5,-8.5,107.1));
#43677=CARTESIAN_POINT('Origin',(-10.5,-9.5,107.));
#43678=CARTESIAN_POINT('',(-9.5,-9.5,107.1));
#43679=CARTESIAN_POINT('',(-9.5,-9.5,107.));
#43680=CARTESIAN_POINT('',(-5.25,-9.5,107.1));
#43681=CARTESIAN_POINT('',(3.,-9.5,107.745));
#43682=CARTESIAN_POINT('Origin',(3.,-9.5,108.25));
#43683=CARTESIAN_POINT('Origin',(-9.5,6.,109.35));
#43684=CARTESIAN_POINT('',(-9.5,6.7,109.5));
#43685=CARTESIAN_POINT('',(-10.2,6.,109.5));
#43686=CARTESIAN_POINT('Origin',(-10.35,2.875,109.35));
#43687=CARTESIAN_POINT('Origin',(8.15,-5.8,123.5));
#43688=CARTESIAN_POINT('',(8.2,-5.85,123.5));
#43689=CARTESIAN_POINT('',(8.1,-5.75,123.5));
#43690=CARTESIAN_POINT('',(7.92499999999999,-5.575,123.5));
#43691=CARTESIAN_POINT('',(8.1,-5.75,128.));
#43692=CARTESIAN_POINT('',(8.1,-5.75,123.5));
#43693=CARTESIAN_POINT('',(8.2,-5.85,128.));
#43694=CARTESIAN_POINT('',(8.1,-5.75,128.));
#43695=CARTESIAN_POINT('',(8.2,-5.85,123.5));
#43696=CARTESIAN_POINT('Origin',(7.7,-5.8,128.));
#43697=CARTESIAN_POINT('',(7.7,-5.75,128.4));
#43698=CARTESIAN_POINT('',(7.7,-5.85,128.5));
#43699=CARTESIAN_POINT('',(7.7,-5.75,128.4));
#43700=CARTESIAN_POINT('Origin',(7.7,-5.85,128.));
#43701=CARTESIAN_POINT('Origin',(7.7,-5.75,128.));
#43702=CARTESIAN_POINT('Origin',(7.6,-5.8,128.45));
#43703=CARTESIAN_POINT('',(6.3,-5.75,128.4));
#43704=CARTESIAN_POINT('',(6.3,-5.85,128.5));
#43705=CARTESIAN_POINT('',(6.3,-5.75,128.4));
#43706=CARTESIAN_POINT('',(7.6,-5.85,128.5));
#43707=CARTESIAN_POINT('',(7.6,-5.75,128.4));
#43708=CARTESIAN_POINT('Origin',(6.3,-5.8,128.));
#43709=CARTESIAN_POINT('',(5.89999999999999,-5.75,128.));
#43710=CARTESIAN_POINT('',(5.8,-5.85,128.));
#43711=CARTESIAN_POINT('',(5.89999999999999,-5.75,128.));
#43712=CARTESIAN_POINT('Origin',(6.3,-5.85,128.));
#43713=CARTESIAN_POINT('Origin',(6.3,-5.75,128.));
#43714=CARTESIAN_POINT('Origin',(5.85,-5.8,123.5));
#43715=CARTESIAN_POINT('',(5.9,-5.75,123.5));
#43716=CARTESIAN_POINT('',(5.8,-5.85,123.5));
#43717=CARTESIAN_POINT('',(6.075,-5.575,123.5));
#43718=CARTESIAN_POINT('',(5.8,-5.85,123.5));
#43719=CARTESIAN_POINT('',(5.9,-5.75,123.5));
#43720=CARTESIAN_POINT('Origin',(7.,-6.05,123.5));
#43721=CARTESIAN_POINT('',(6.21259921259882,-5.75,123.5));
#43722=CARTESIAN_POINT('',(8.2,-5.75,123.5));
#43723=CARTESIAN_POINT('',(5.8,-6.06752483470939,123.5));
#43724=CARTESIAN_POINT('Origin',(7.,-7.2,123.5));
#43725=CARTESIAN_POINT('',(5.8,-5.75,123.5));
#43726=CARTESIAN_POINT('Origin',(8.2,-5.75,123.5));
#43727=CARTESIAN_POINT('',(7.78740078740118,-5.75,123.5));
#43728=CARTESIAN_POINT('',(8.2,-5.75,123.5));
#43729=CARTESIAN_POINT('',(7.6,-5.75,123.5));
#43730=CARTESIAN_POINT('Origin',(5.85,-6.3,123.5));
#43731=CARTESIAN_POINT('',(5.8,-6.25,123.5));
#43732=CARTESIAN_POINT('',(5.9,-6.35,123.5));
#43733=CARTESIAN_POINT('',(6.3625,-6.8125,123.5));
#43734=CARTESIAN_POINT('',(5.9,-6.35,128.));
#43735=CARTESIAN_POINT('',(5.9,-6.35,123.5));
#43736=CARTESIAN_POINT('',(5.8,-6.25,128.));
#43737=CARTESIAN_POINT('',(5.9,-6.35,128.));
#43738=CARTESIAN_POINT('',(5.8,-6.25,123.5));
#43739=CARTESIAN_POINT('Origin',(6.3,-6.3,128.));
#43740=CARTESIAN_POINT('',(6.3,-6.35,128.4));
#43741=CARTESIAN_POINT('',(6.3,-6.25,128.5));
#43742=CARTESIAN_POINT('',(6.3,-6.35,128.4));
#43743=CARTESIAN_POINT('Origin',(6.3,-6.25,128.));
#43744=CARTESIAN_POINT('Origin',(6.3,-6.35,128.));
#43745=CARTESIAN_POINT('Origin',(6.4,-6.3,128.45));
#43746=CARTESIAN_POINT('',(7.7,-6.35,128.4));
#43747=CARTESIAN_POINT('',(7.7,-6.25,128.5));
#43748=CARTESIAN_POINT('',(7.7,-6.35,128.4));
#43749=CARTESIAN_POINT('',(6.4,-6.25,128.5));
#43750=CARTESIAN_POINT('',(6.4,-6.35,128.4));
#43751=CARTESIAN_POINT('Origin',(7.7,-6.3,128.));
#43752=CARTESIAN_POINT('',(8.10000000000001,-6.35,128.));
#43753=CARTESIAN_POINT('',(8.2,-6.25,128.));
#43754=CARTESIAN_POINT('',(8.10000000000001,-6.35,128.));
#43755=CARTESIAN_POINT('Origin',(7.7,-6.25,128.));
#43756=CARTESIAN_POINT('Origin',(7.7,-6.35,128.));
#43757=CARTESIAN_POINT('Origin',(8.15,-6.3,123.5));
#43758=CARTESIAN_POINT('',(8.1,-6.35,123.5));
#43759=CARTESIAN_POINT('',(8.2,-6.25,123.5));
#43760=CARTESIAN_POINT('',(7.6375,-6.8125,123.5));
#43761=CARTESIAN_POINT('',(8.2,-6.25,123.5));
#43762=CARTESIAN_POINT('',(8.1,-6.35,123.5));
#43763=CARTESIAN_POINT('Origin',(5.8,-6.35,123.5));
#43764=CARTESIAN_POINT('',(6.4,-6.35,123.5));
#43765=CARTESIAN_POINT('',(6.5,-6.35,127.));
#43766=CARTESIAN_POINT('Origin',(7.,-6.35,127.));
#43767=CARTESIAN_POINT('Origin',(8.15,-8.1,123.5));
#43768=CARTESIAN_POINT('',(8.2,-8.15,123.5));
#43769=CARTESIAN_POINT('',(8.1,-8.05,123.5));
#43770=CARTESIAN_POINT('',(7.63749999999999,-7.58750000000001,123.5));
#43771=CARTESIAN_POINT('',(8.1,-8.05,128.));
#43772=CARTESIAN_POINT('',(8.1,-8.05,123.5));
#43773=CARTESIAN_POINT('',(8.2,-8.15,128.));
#43774=CARTESIAN_POINT('',(8.1,-8.05,128.));
#43775=CARTESIAN_POINT('',(8.2,-8.15,123.5));
#43776=CARTESIAN_POINT('Origin',(7.7,-8.1,128.));
#43777=CARTESIAN_POINT('',(7.7,-8.05,128.4));
#43778=CARTESIAN_POINT('',(7.7,-8.15,128.5));
#43779=CARTESIAN_POINT('',(7.7,-8.05,128.4));
#43780=CARTESIAN_POINT('Origin',(7.7,-8.15,128.));
#43781=CARTESIAN_POINT('Origin',(7.7,-8.05,128.));
#43782=CARTESIAN_POINT('Origin',(7.6,-8.1,128.45));
#43783=CARTESIAN_POINT('',(6.3,-8.05,128.4));
#43784=CARTESIAN_POINT('',(6.3,-8.15,128.5));
#43785=CARTESIAN_POINT('',(6.3,-8.05,128.4));
#43786=CARTESIAN_POINT('',(7.6,-8.15,128.5));
#43787=CARTESIAN_POINT('',(7.6,-8.05,128.4));
#43788=CARTESIAN_POINT('Origin',(6.3,-8.1,128.));
#43789=CARTESIAN_POINT('',(5.89999999999999,-8.05,128.));
#43790=CARTESIAN_POINT('',(5.8,-8.15,128.));
#43791=CARTESIAN_POINT('',(5.89999999999999,-8.05,128.));
#43792=CARTESIAN_POINT('Origin',(6.3,-8.15,128.));
#43793=CARTESIAN_POINT('Origin',(6.3,-8.05,128.));
#43794=CARTESIAN_POINT('Origin',(5.85,-8.1,123.5));
#43795=CARTESIAN_POINT('',(5.9,-8.05,123.5));
#43796=CARTESIAN_POINT('',(5.8,-8.15,123.5));
#43797=CARTESIAN_POINT('',(6.3625,-7.5875,123.5));
#43798=CARTESIAN_POINT('',(5.8,-8.15,123.5));
#43799=CARTESIAN_POINT('',(5.9,-8.05,123.5));
#43800=CARTESIAN_POINT('Origin',(8.2,-8.05,123.5));
#43801=CARTESIAN_POINT('',(7.6,-8.05,123.5));
#43802=CARTESIAN_POINT('',(6.5,-8.05,127.));
#43803=CARTESIAN_POINT('Origin',(7.,-8.05,127.));
#43804=CARTESIAN_POINT('Origin',(5.85,-8.6,123.5));
#43805=CARTESIAN_POINT('',(5.8,-8.55,123.5));
#43806=CARTESIAN_POINT('',(5.9,-8.65,123.5));
#43807=CARTESIAN_POINT('',(6.075,-8.825,123.5));
#43808=CARTESIAN_POINT('',(5.9,-8.65,128.));
#43809=CARTESIAN_POINT('',(5.9,-8.65,123.5));
#43810=CARTESIAN_POINT('',(5.8,-8.55,128.));
#43811=CARTESIAN_POINT('',(5.9,-8.65,128.));
#43812=CARTESIAN_POINT('',(5.8,-8.55,123.5));
#43813=CARTESIAN_POINT('Origin',(6.3,-8.6,128.));
#43814=CARTESIAN_POINT('',(6.3,-8.65,128.4));
#43815=CARTESIAN_POINT('',(6.3,-8.55,128.5));
#43816=CARTESIAN_POINT('',(6.3,-8.65,128.4));
#43817=CARTESIAN_POINT('Origin',(6.3,-8.55,128.));
#43818=CARTESIAN_POINT('Origin',(6.3,-8.65,128.));
#43819=CARTESIAN_POINT('Origin',(6.4,-8.6,128.45));
#43820=CARTESIAN_POINT('',(7.7,-8.65,128.4));
#43821=CARTESIAN_POINT('',(7.7,-8.55,128.5));
#43822=CARTESIAN_POINT('',(7.7,-8.65,128.4));
#43823=CARTESIAN_POINT('',(6.4,-8.55,128.5));
#43824=CARTESIAN_POINT('',(6.4,-8.65,128.4));
#43825=CARTESIAN_POINT('Origin',(7.7,-8.6,128.));
#43826=CARTESIAN_POINT('',(8.10000000000001,-8.65,128.));
#43827=CARTESIAN_POINT('',(8.2,-8.55,128.));
#43828=CARTESIAN_POINT('',(8.10000000000001,-8.65,128.));
#43829=CARTESIAN_POINT('Origin',(7.7,-8.55,128.));
#43830=CARTESIAN_POINT('Origin',(7.7,-8.65,128.));
#43831=CARTESIAN_POINT('Origin',(8.15,-8.6,123.5));
#43832=CARTESIAN_POINT('',(8.1,-8.65,123.5));
#43833=CARTESIAN_POINT('',(8.2,-8.55,123.5));
#43834=CARTESIAN_POINT('',(7.925,-8.825,123.5));
#43835=CARTESIAN_POINT('',(8.2,-8.55,123.5));
#43836=CARTESIAN_POINT('',(8.1,-8.65,123.5));
#43837=CARTESIAN_POINT('Origin',(5.8,-8.05,123.5));
#43838=CARTESIAN_POINT('',(5.8,-8.33247516529063,123.5));
#43839=CARTESIAN_POINT('',(5.8,-7.625,123.5));
#43840=CARTESIAN_POINT('',(5.8,-8.05,123.5));
#43841=CARTESIAN_POINT('',(5.8,-8.2,128.));
#43842=CARTESIAN_POINT('Origin',(6.3,-8.2,128.));
#43843=CARTESIAN_POINT('',(6.3,-8.2,128.5));
#43844=CARTESIAN_POINT('Origin',(7.,-8.35,128.5));
#43845=CARTESIAN_POINT('',(7.7,-8.5,128.5));
#43846=CARTESIAN_POINT('Origin',(7.7,-8.5,128.));
#43847=CARTESIAN_POINT('',(8.2,-8.5,128.));
#43848=CARTESIAN_POINT('Origin',(8.2,-8.65,123.5));
#43849=CARTESIAN_POINT('',(8.2,-8.33247516529064,123.5));
#43850=CARTESIAN_POINT('',(8.2,-8.65,123.5));
#43851=CARTESIAN_POINT('',(8.2,-7.925,123.5));
#43852=CARTESIAN_POINT('Origin',(7.,-8.35,123.5));
#43853=CARTESIAN_POINT('',(7.78740078740121,-8.65,123.5));
#43854=CARTESIAN_POINT('',(5.8,-8.65,123.5));
#43855=CARTESIAN_POINT('Origin',(7.,-7.2,123.5));
#43856=CARTESIAN_POINT('Origin',(-8.5,0.,110.45));
#43857=CARTESIAN_POINT('',(-9.4,1.10218211923262E-16,110.5));
#43858=CARTESIAN_POINT('Origin',(-8.5,0.,110.5));
#43859=CARTESIAN_POINT('',(-9.5,-1.22464679914735E-16,110.4));
#43860=CARTESIAN_POINT('',(-9.45,-1.16341445918999E-16,110.45));
#43861=CARTESIAN_POINT('Origin',(-8.5,0.,110.4));
#43862=CARTESIAN_POINT('Origin',(-8.5,0.,110.5));
#43863=CARTESIAN_POINT('',(-9.01,-6.2456986756515E-17,110.5));
#43864=CARTESIAN_POINT('Origin',(-8.5,0.,110.5));
#43865=CARTESIAN_POINT('Origin',(-8.5,0.,109.4));
#43866=CARTESIAN_POINT('',(-9.5,-1.22464679914735E-16,109.4));
#43867=CARTESIAN_POINT('Origin',(-8.5,0.,110.45));
#43868=CARTESIAN_POINT('',(-8.91,5.02105187650415E-17,110.4));
#43869=CARTESIAN_POINT('',(-8.96,-5.63337527607782E-17,110.45));
#43870=CARTESIAN_POINT('Origin',(-8.5,0.,110.4));
#43871=CARTESIAN_POINT('Origin',(-8.5,0.,110.115));
#43872=CARTESIAN_POINT('',(-8.91,-5.02105187650415E-17,109.7));
#43873=CARTESIAN_POINT('Origin',(-8.5,0.,109.7));
#43874=CARTESIAN_POINT('',(-8.91,-5.02105187650415E-17,110.115));
#43875=CARTESIAN_POINT('Origin',(3.,-9.45,108.25));
#43876=CARTESIAN_POINT('',(3.,-9.4,107.845));
#43877=CARTESIAN_POINT('',(3.,-9.45,107.795));
#43878=CARTESIAN_POINT('Origin',(3.,-9.4,108.25));
#43879=CARTESIAN_POINT('Origin',(3.,-8.515,108.25));
#43880=CARTESIAN_POINT('',(3.,-7.5,107.845));
#43881=CARTESIAN_POINT('',(3.,-8.515,107.845));
#43882=CARTESIAN_POINT('Origin',(3.,-7.5,108.25));
#43883=CARTESIAN_POINT('Origin',(3.,-7.5,108.25));
#43884=CARTESIAN_POINT('',(3.,-7.25665144929384,108.25));
#43885=CARTESIAN_POINT('',(3.,-7.5,107.845));
#43886=CARTESIAN_POINT('Origin',(-8.5,0.,109.576823573099));
#43887=CARTESIAN_POINT('',(-8.5,0.,109.453647146199));
#43888=CARTESIAN_POINT('',(-8.705,-2.51052593825207E-17,109.576823573099));
#43889=CARTESIAN_POINT('Origin',(7.,-8.65,127.));
#43890=CARTESIAN_POINT('',(6.5,-8.65,127.));
#43891=CARTESIAN_POINT('Origin',(6.3,-5.9,128.));
#43892=CARTESIAN_POINT('',(5.8,-5.9,128.));
#43893=CARTESIAN_POINT('',(6.3,-5.9,128.5));
#43894=CARTESIAN_POINT('Origin',(7.,-6.05,128.5));
#43895=CARTESIAN_POINT('',(7.7,-6.2,128.5));
#43896=CARTESIAN_POINT('Origin',(7.7,-6.2,128.));
#43897=CARTESIAN_POINT('',(8.2,-6.2,128.));
#43898=CARTESIAN_POINT('Origin',(7.,-6.05,123.5));
#43899=CARTESIAN_POINT('',(8.2,-6.06752483470939,123.5));
#43900=CARTESIAN_POINT('',(8.2,-6.35,123.5));
#43901=CARTESIAN_POINT('Origin',(7.,-7.2,123.5));
#43902=CARTESIAN_POINT('Origin',(8.2,-6.35,123.5));
#43903=CARTESIAN_POINT('',(8.2,-6.775,123.5));
#43904=CARTESIAN_POINT('Origin',(5.8,-5.75,123.5));
#43905=CARTESIAN_POINT('',(5.8,-6.475,123.5));
#43906=CARTESIAN_POINT('Origin',(7.,-7.2,123.5));
#43907=CARTESIAN_POINT('Origin',(7.,-7.2,123.5));
#43908=CARTESIAN_POINT('Origin',(7.,-8.35,123.5));
#43909=CARTESIAN_POINT('',(6.21259921259879,-8.65,123.5));
#43910=CARTESIAN_POINT('Origin',(7.,-7.2,123.5));
#43911=CARTESIAN_POINT('',(5.8,-8.65,123.5));
#43912=CARTESIAN_POINT('Origin',(5.8,-8.65,123.5));
#43913=CARTESIAN_POINT('',(6.4,-8.65,123.5));
#43914=CARTESIAN_POINT('Origin',(7.,-7.2,123.5));
#43915=CARTESIAN_POINT('Origin',(7.,-7.2,123.5));
#43916=CARTESIAN_POINT('Origin',(7.,-7.2,123.5));
#43917=CARTESIAN_POINT('',(5.35,-7.2,123.5));
#43918=CARTESIAN_POINT('Origin',(7.,-7.2,123.5));
#43919=CARTESIAN_POINT('Origin',(7.,-7.2,123.5));
#43920=CARTESIAN_POINT('Origin',(7.,-7.2,123.5));
#43921=CARTESIAN_POINT('Origin',(7.,-7.2,123.425));
#43922=CARTESIAN_POINT('',(5.2,-7.2,123.35));
#43923=CARTESIAN_POINT('',(5.275,-7.2,123.425));
#43924=CARTESIAN_POINT('Origin',(7.,-7.2,123.35));
#43925=CARTESIAN_POINT('Origin',(7.,-7.2,109.4));
#43926=CARTESIAN_POINT('',(5.2,-7.2,109.4));
#43927=CARTESIAN_POINT('Origin',(0.,0.,129.45));
#43928=CARTESIAN_POINT('',(-2.755,-3.37390193165096E-16,129.5));
#43929=CARTESIAN_POINT('Origin',(0.,0.,129.5));
#43930=CARTESIAN_POINT('',(-2.655,3.25143725173622E-16,129.4));
#43931=CARTESIAN_POINT('',(-2.705,-3.31266959169359E-16,129.45));
#43932=CARTESIAN_POINT('Origin',(0.,0.,129.4));
#43933=CARTESIAN_POINT('Origin',(0.,0.,120.275));
#43934=CARTESIAN_POINT('',(-2.655,-3.25143725173622E-16,111.));
#43935=CARTESIAN_POINT('Origin',(0.,0.,111.));
#43936=CARTESIAN_POINT('',(-2.655,-3.25143725173622E-16,120.275));
#43937=CARTESIAN_POINT('Origin',(0.,0.,129.5));
#43938=CARTESIAN_POINT('',(-5.29999999999999,-6.49062803548096E-16,129.5));
#43939=CARTESIAN_POINT('Origin',(0.,0.,129.5));
#43940=CARTESIAN_POINT('Origin',(4.85,0.,124.9));
#43941=CARTESIAN_POINT('Origin',(0.,0.,124.9));
#43942=CARTESIAN_POINT('Origin',(5.05,0.,124.5));
#43943=CARTESIAN_POINT('Origin',(0.,0.,124.5));
#43944=CARTESIAN_POINT('Origin',(2.655,0.,111.));
#43945=CARTESIAN_POINT('Origin',(0.,0.,109.9));
#43946=CARTESIAN_POINT('',(-5.,6.12323399573677E-16,109.9));
#43947=CARTESIAN_POINT('',(5.,-6.12323399573677E-16,109.9));
#43948=CARTESIAN_POINT('Origin',(0.,0.,109.9));
#43949=CARTESIAN_POINT('Origin',(5.4,-6.61309271539571E-16,109.9));
#43950=CARTESIAN_POINT('Origin',(0.,0.,109.9));
#43951=CARTESIAN_POINT('Origin',(0.,0.,118.45));
#43952=CARTESIAN_POINT('',(-5.,-6.12323399573677E-16,127.5));
#43953=CARTESIAN_POINT('Origin',(0.,0.,127.5));
#43954=CARTESIAN_POINT('',(-5.,-6.12323399573677E-16,118.45));
#43955=CARTESIAN_POINT('Origin',(5.3,0.,127.5));
#43956=CARTESIAN_POINT('',(-5.3,-6.49062803548097E-16,127.5));
#43957=CARTESIAN_POINT('Origin',(0.,0.,127.5));
#43958=CARTESIAN_POINT('Origin',(0.,0.,127.55));
#43959=CARTESIAN_POINT('',(-5.4,-6.61309271539571E-16,127.6));
#43960=CARTESIAN_POINT('Origin',(0.,0.,127.6));
#43961=CARTESIAN_POINT('',(-5.35,-6.55186037543834E-16,127.55));
#43962=CARTESIAN_POINT('Origin',(0.,0.,128.5));
#43963=CARTESIAN_POINT('',(-5.4,-6.61309271539571E-16,129.4));
#43964=CARTESIAN_POINT('Origin',(0.,0.,129.4));
#43965=CARTESIAN_POINT('',(-5.4,-6.61309271539571E-16,128.5));
#43966=CARTESIAN_POINT('Origin',(0.,0.,129.45));
#43967=CARTESIAN_POINT('',(-5.35,-6.55186037543834E-16,129.45));
#43968=CARTESIAN_POINT('Origin',(10.45,-5.375,107.05));
#43969=CARTESIAN_POINT('',(10.4,6.,107.));
#43970=CARTESIAN_POINT('',(10.4,6.,107.));
#43971=CARTESIAN_POINT('',(10.4,-8.5,107.));
#43972=CARTESIAN_POINT('',(10.5,-8.5,107.1));
#43973=CARTESIAN_POINT('',(10.4,-5.375,107.));
#43974=CARTESIAN_POINT('Origin',(9.5,6.,107.05));
#43975=CARTESIAN_POINT('',(9.5,6.9,107.));
#43976=CARTESIAN_POINT('',(9.5,6.9,107.));
#43977=CARTESIAN_POINT('Origin',(9.5,6.,107.));
#43978=CARTESIAN_POINT('Origin',(5.25,6.95,107.05));
#43979=CARTESIAN_POINT('',(-9.5,6.9,107.));
#43980=CARTESIAN_POINT('',(-9.5,7.,107.1));
#43981=CARTESIAN_POINT('',(-9.5,6.9,107.));
#43982=CARTESIAN_POINT('',(5.25,7.,107.1));
#43983=CARTESIAN_POINT('',(5.25,6.9,107.));
#43984=CARTESIAN_POINT('Origin',(-9.5,6.,107.05));
#43985=CARTESIAN_POINT('',(-10.4,6.,107.));
#43986=CARTESIAN_POINT('',(-10.5,6.,107.1));
#43987=CARTESIAN_POINT('',(-10.4,6.,107.));
#43988=CARTESIAN_POINT('Origin',(-9.5,6.,107.1));
#43989=CARTESIAN_POINT('Origin',(-9.5,6.,107.));
#43990=CARTESIAN_POINT('Origin',(-10.45,2.875,107.05));
#43991=CARTESIAN_POINT('',(-10.4,-8.5,107.));
#43992=CARTESIAN_POINT('',(-10.5,-8.5,107.1));
#43993=CARTESIAN_POINT('',(-10.4,-8.5,107.));
#43994=CARTESIAN_POINT('',(-10.5,2.875,107.1));
#43995=CARTESIAN_POINT('',(-10.4,2.875,107.));
#43996=CARTESIAN_POINT('Origin',(-9.5,-8.5,107.05));
#43997=CARTESIAN_POINT('',(-9.5,-9.4,107.));
#43998=CARTESIAN_POINT('',(-9.5,-9.4,107.));
#43999=CARTESIAN_POINT('Origin',(-9.5,-8.5,107.1));
#44000=CARTESIAN_POINT('Origin',(-9.5,-8.5,107.));
#44001=CARTESIAN_POINT('Origin',(-5.25,-9.45,107.05));
#44002=CARTESIAN_POINT('',(9.5,-9.4,107.));
#44003=CARTESIAN_POINT('',(9.5,-9.4,107.));
#44004=CARTESIAN_POINT('',(-5.25,-9.4,107.));
#44005=CARTESIAN_POINT('Origin',(9.5,-8.5,107.05));
#44006=CARTESIAN_POINT('Origin',(9.5,-8.5,107.));
#44007=CARTESIAN_POINT('Origin',(-9.5,-8.5,107.));
#44008=CARTESIAN_POINT('',(-10.5,-8.5,107.));
#44009=CARTESIAN_POINT('Origin',(0.,-1.25,107.));
#44010=CARTESIAN_POINT('Origin',(5.25,6.85,109.35));
#44011=CARTESIAN_POINT('',(9.5,6.7,109.5));
#44012=CARTESIAN_POINT('Origin',(9.5,6.,109.35));
#44013=CARTESIAN_POINT('Origin',(-10.5,7.,107.));
#44014=CARTESIAN_POINT('',(-10.5,6.,107.));
#44015=CARTESIAN_POINT('Origin',(-9.5,6.,107.));
#44016=CARTESIAN_POINT('',(-9.5,7.,107.));
#44017=CARTESIAN_POINT('Origin',(10.5,7.,107.));
#44018=CARTESIAN_POINT('',(0.,0.,0.));
#44019=CARTESIAN_POINT('Origin',(0.,0.,131.75));
#44020=CARTESIAN_POINT('',(-1.48662474598514,6.70630482219048E-6,131.11245853209));
#44021=CARTESIAN_POINT('',(-1.4866687345303,-8.57105652977442E-7,131.06254146791));
#44022=CARTESIAN_POINT('',(-1.486725,-1.82071301246235E-16,131.75));
#44023=CARTESIAN_POINT('',(0.644080091015134,1.33993887967327,131.));
#44024=CARTESIAN_POINT('Ctrl Pts',(-1.48662474598514,6.70630482219048E-6,
131.11245853209));
#44025=CARTESIAN_POINT('Ctrl Pts',(-1.48664238717497,0.112082357541715,
131.10826015708));
#44026=CARTESIAN_POINT('Ctrl Pts',(-1.47411630956215,0.224154129411391,
131.104061782071));
#44027=CARTESIAN_POINT('Ctrl Pts',(-1.44900147170679,0.333329954091576,
131.099863407061));
#44028=CARTESIAN_POINT('Ctrl Pts',(-1.39531127956612,0.566724692212197,
131.090888172491));
#44029=CARTESIAN_POINT('Ctrl Pts',(-1.28408873642491,0.786884556765062,
131.081912937921));
#44030=CARTESIAN_POINT('Ctrl Pts',(-1.12807594748543,0.968587090660957,
131.072937703351));
#44031=CARTESIAN_POINT('Ctrl Pts',(-0.972063158545943,1.15028962455685,
131.063962468781));
#44032=CARTESIAN_POINT('Ctrl Pts',(-0.771260123808195,1.29353482779577,
131.054987234211));
#44033=CARTESIAN_POINT('Ctrl Pts',(-0.548672624156139,1.38191112458742,
131.046011999641));
#44034=CARTESIAN_POINT('Ctrl Pts',(-0.326085124504082,1.47028742137907,
131.03703676507));
#44035=CARTESIAN_POINT('Ctrl Pts',(-0.0817131599377159,1.50379481172344,
131.0280615305));
#44036=CARTESIAN_POINT('Ctrl Pts',(0.156447623458401,1.47859617596776,131.01908629593));
#44037=CARTESIAN_POINT('Ctrl Pts',(0.325267990783618,1.46073411285348,131.012724197287));
#44038=CARTESIAN_POINT('Ctrl Pts',(0.490967432775488,1.41337409773075,131.006362098643));
#44039=CARTESIAN_POINT('Ctrl Pts',(0.644080091015134,1.33993887967327,131.));
#44040=CARTESIAN_POINT('',(-0.644068464422626,1.33997277538063,131.));
#44041=CARTESIAN_POINT('Origin',(0.,0.,131.));
#44042=CARTESIAN_POINT('Ctrl Pts',(-0.644068464422466,1.33997277538071,
131.));
#44043=CARTESIAN_POINT('Ctrl Pts',(-0.859968943773443,1.23619851014301,
131.00897523457));
#44044=CARTESIAN_POINT('Ctrl Pts',(-1.05021748697928,1.07929218747651,131.01795046914));
#44045=CARTESIAN_POINT('Ctrl Pts',(-1.19311574373449,0.887131970323545,
131.02692570371));
#44046=CARTESIAN_POINT('Ctrl Pts',(-1.33601400048969,0.694971753170582,
131.03590093828));
#44047=CARTESIAN_POINT('Ctrl Pts',(-1.43156197079426,0.467557641531158,
131.044876172851));
#44048=CARTESIAN_POINT('Ctrl Pts',(-1.46877946004656,0.230978828954324,
131.053851407421));
#44049=CARTESIAN_POINT('Ctrl Pts',(-1.48079111390487,0.154624865697416,
131.056748094251));
#44050=CARTESIAN_POINT('Ctrl Pts',(-1.48672691792441,0.0773162841053159,
131.05964478108));
#44051=CARTESIAN_POINT('Ctrl Pts',(-1.4866687345303,-8.57105652977442E-7,
131.06254146791));
#44052=CARTESIAN_POINT('Origin',(0.,0.,131.75));
#44053=CARTESIAN_POINT('',(-1.48662467006137,6.54543500555605E-6,131.46245853209));
#44054=CARTESIAN_POINT('',(-1.48667651937189,2.89412199965503E-5,131.41254146791));
#44055=CARTESIAN_POINT('',(-1.486725,-1.82071301246235E-16,131.75));
#44056=CARTESIAN_POINT('Ctrl Pts',(-1.48662467006137,6.54543500555605E-6,
131.46245853209));
#44057=CARTESIAN_POINT('Ctrl Pts',(-1.48664293141312,0.111778251545966,
131.458271539825));
#44058=CARTESIAN_POINT('Ctrl Pts',(-1.47418526351766,0.22354594941412,131.454084547561));
#44059=CARTESIAN_POINT('Ctrl Pts',(-1.44920521898838,0.332441071167058,
131.449897555296));
#44060=CARTESIAN_POINT('Ctrl Pts',(-1.39565800775678,0.565868600880252,
131.440922320726));
#44061=CARTESIAN_POINT('Ctrl Pts',(-1.28457023968935,0.786096589160032,
131.431947086156));
#44062=CARTESIAN_POINT('Ctrl Pts',(-1.12866878379445,0.967894420568027,
131.422971851586));
#44063=CARTESIAN_POINT('Ctrl Pts',(-0.972767327899546,1.14969225197602,
131.413996617016));
#44064=CARTESIAN_POINT('Ctrl Pts',(-0.772052184177181,1.29305992651223,
131.405021382445));
#44065=CARTESIAN_POINT('Ctrl Pts',(-0.549518461659608,1.38157239901168,
131.396046147875));
#44066=CARTESIAN_POINT('Ctrl Pts',(-0.326984739142031,1.47008487151113,
131.387070913305));
#44067=CARTESIAN_POINT('Ctrl Pts',(-0.0826324378292454,1.50374214197381,
131.378095678735));
#44068=CARTESIAN_POINT('Ctrl Pts',(0.155544003393841,1.47868823524661,131.369120444165));
#44069=CARTESIAN_POINT('Ctrl Pts',(0.393720444616925,1.45363432851941,131.360145209595));
#44070=CARTESIAN_POINT('Ctrl Pts',(0.62572102575031,1.36986924460234,131.351169975025));
#44071=CARTESIAN_POINT('Ctrl Pts',(0.824966393821326,1.23698960503629,131.342194740455));
#44072=CARTESIAN_POINT('Ctrl Pts',(1.02421176189234,1.10410996547024,131.333219505884));
#44073=CARTESIAN_POINT('Ctrl Pts',(1.19070191690099,0.922115770255228,131.324244271314));
#44074=CARTESIAN_POINT('Ctrl Pts',(1.30536276582783,0.711857346200688,131.315269036744));
#44075=CARTESIAN_POINT('Ctrl Pts',(1.42002361475467,0.501598922146148,131.306293802174));
#44076=CARTESIAN_POINT('Ctrl Pts',(1.4828551575997,0.263076269252084,131.297318567604));
#44077=CARTESIAN_POINT('Ctrl Pts',(1.48665904299347,0.0236159482411607,
131.288343333034));
#44078=CARTESIAN_POINT('Ctrl Pts',(1.49046292838724,-0.215844372769763,
131.279368098464));
#44079=CARTESIAN_POINT('Ctrl Pts',(1.43523915632975,-0.456242361897546,
131.270392863894));
#44080=CARTESIAN_POINT('Ctrl Pts',(1.32731448618016,-0.670036610261909,
131.261417629323));
#44081=CARTESIAN_POINT('Ctrl Pts',(1.21938981603057,-0.883830858626271,
131.252442394753));
#44082=CARTESIAN_POINT('Ctrl Pts',(1.05876424778888,-1.07102136622721,131.243467160183));
#44083=CARTESIAN_POINT('Ctrl Pts',(0.863839993987138,-1.21016248254433,
131.234491925613));
#44084=CARTESIAN_POINT('Ctrl Pts',(0.668915740185388,-1.34930359886145,
131.225516691043));
#44085=CARTESIAN_POINT('Ctrl Pts',(0.439692800823575,-1.44039532389473,
131.216541456473));
#44086=CARTESIAN_POINT('Ctrl Pts',(0.202432300225987,-1.47300165684166,
131.207566221903));
#44087=CARTESIAN_POINT('Ctrl Pts',(-0.0348282003715965,-1.5056079897886,
131.198590987333));
#44088=CARTESIAN_POINT('Ctrl Pts',(-0.280126262204957,-1.47972893064917,
131.189615752763));
#44089=CARTESIAN_POINT('Ctrl Pts',(-0.505359087071109,-1.39832932086742,
131.180640518192));
#44090=CARTESIAN_POINT('Ctrl Pts',(-0.730591911937262,-1.31692971108566,
131.171665283622));
#44091=CARTESIAN_POINT('Ctrl Pts',(-0.935759499836208,-1.18000955066158,
131.162690049052));
#44092=CARTESIAN_POINT('Ctrl Pts',(-1.09735667018443,-1.00325523997758,
131.153714814482));
#44093=CARTESIAN_POINT('Ctrl Pts',(-1.25895384053266,-0.826500929293591,
131.144739579912));
#44094=CARTESIAN_POINT('Ctrl Pts',(-1.37698059333016,-0.609912468349694,
131.135764345342));
#44095=CARTESIAN_POINT('Ctrl Pts',(-1.43791504915886,-0.378303432033558,
131.126789110772));
#44096=CARTESIAN_POINT('Ctrl Pts',(-1.47034599406822,-0.255034916788333,
131.122012251211));
#44097=CARTESIAN_POINT('Ctrl Pts',(-1.48660467405586,-0.127511594203174,
131.117235391651));
#44098=CARTESIAN_POINT('Ctrl Pts',(-1.48662474598514,6.70630482219048E-6,
131.11245853209));
#44099=CARTESIAN_POINT('Ctrl Pts',(-1.4866687345303,-8.57105652977442E-7,
131.06254146791));
#44100=CARTESIAN_POINT('Ctrl Pts',(-1.48654663968209,-0.162246885628005,
131.06862001565));
#44101=CARTESIAN_POINT('Ctrl Pts',(-1.46003010793999,-0.324530606308262,
131.074698563391));
#44102=CARTESIAN_POINT('Ctrl Pts',(-1.40787558798148,-0.478109975852054,
131.080777111131));
#44103=CARTESIAN_POINT('Ctrl Pts',(-1.33086721846408,-0.704876454567354,
131.089752345701));
#44104=CARTESIAN_POINT('Ctrl Pts',(-1.19796347122924,-0.91266589848371,
131.098727580271));
#44105=CARTESIAN_POINT('Ctrl Pts',(-1.02438398444855,-1.07766566984475,
131.107702814842));
#44106=CARTESIAN_POINT('Ctrl Pts',(-0.85080449766787,-1.2426654412058,131.116678049412));
#44107=CARTESIAN_POINT('Ctrl Pts',(-0.636549271341341,-1.36487554001152,
131.125653283982));
#44108=CARTESIAN_POINT('Ctrl Pts',(-0.406167987067542,-1.43029720218641,
131.134628518552));
#44109=CARTESIAN_POINT('Ctrl Pts',(-0.175786702793742,-1.49571886436129,
131.143603753122));
#44110=CARTESIAN_POINT('Ctrl Pts',(0.0707206394273271,-1.50435208990532,
131.152578987692));
#44111=CARTESIAN_POINT('Ctrl Pts',(0.30511402383943,-1.45520632418145,131.161554222262));
#44112=CARTESIAN_POINT('Ctrl Pts',(0.539507408251534,-1.40606055845758,
131.170529456832));
#44113=CARTESIAN_POINT('Ctrl Pts',(0.761786834854671,-1.2991358014658,131.179504691402));
#44114=CARTESIAN_POINT('Ctrl Pts',(0.946485973897794,-1.14668243377515,
131.188479925973));
#44115=CARTESIAN_POINT('Ctrl Pts',(1.13118511294092,-0.994229066084504,
131.197455160543));
#44116=CARTESIAN_POINT('Ctrl Pts',(1.27830396442402,-0.796247087694984,
131.206430395113));
#44117=CARTESIAN_POINT('Ctrl Pts',(1.37098798792177,-0.57541816644418,131.215405629683));
#44118=CARTESIAN_POINT('Ctrl Pts',(1.46367201141952,-0.354589245193374,
131.224380864253));
#44119=CARTESIAN_POINT('Ctrl Pts',(1.5019212069319,-0.11091338108128,131.233356098823));
#44120=CARTESIAN_POINT('Ctrl Pts',(1.48135337845442,0.127692398802491,131.242331333393));
#44121=CARTESIAN_POINT('Ctrl Pts',(1.46078554997695,0.366298178686261,131.251306567963));
#44122=CARTESIAN_POINT('Ctrl Pts',(1.38140069750961,0.599833874341709,131.260281802533));
#44123=CARTESIAN_POINT('Ctrl Pts',(1.25229366895348,0.801544328040148,131.269257037104));
#44124=CARTESIAN_POINT('Ctrl Pts',(1.12318664039736,1.00325478173859,131.278232271674));
#44125=CARTESIAN_POINT('Ctrl Pts',(0.944357435752443,1.17313999348001,131.287207506244));
#44126=CARTESIAN_POINT('Ctrl Pts',(0.736293752205015,1.29173689729788,131.296182740814));
#44127=CARTESIAN_POINT('Ctrl Pts',(0.528230068657587,1.41033380111575,131.305157975384));
#44128=CARTESIAN_POINT('Ctrl Pts',(0.290931906207645,1.47764239701006,131.314133209954));
#44129=CARTESIAN_POINT('Ctrl Pts',(0.0515855500820499,1.48595143028722,
131.323108444524));
#44130=CARTESIAN_POINT('Ctrl Pts',(-0.187760806043545,1.49426046356437,
131.332083679094));
#44131=CARTESIAN_POINT('Ctrl Pts',(-0.429155355844794,1.44356993422436,
131.341058913665));
#44132=CARTESIAN_POINT('Ctrl Pts',(-0.64494252417023,1.33968724516187,131.350034148235));
#44133=CARTESIAN_POINT('Ctrl Pts',(-0.860729692495666,1.23580455609938,
131.359009382805));
#44134=CARTESIAN_POINT('Ctrl Pts',(-1.05090947934529,1.07872970731441,131.367984617375));
#44135=CARTESIAN_POINT('Ctrl Pts',(-1.1936937662667,0.8864581217929,131.376959851945));
#44136=CARTESIAN_POINT('Ctrl Pts',(-1.33647805318811,0.694186536271395,
131.385935086515));
#44137=CARTESIAN_POINT('Ctrl Pts',(-1.4318668401813,0.466718214013358,131.394910321085));
#44138=CARTESIAN_POINT('Ctrl Pts',(-1.46893182730532,0.230113265328173,
131.403885555655));
#44139=CARTESIAN_POINT('Ctrl Pts',(-1.48084725502128,0.154050938532649,
131.40677085974));
#44140=CARTESIAN_POINT('Ctrl Pts',(-1.48673518054972,0.0770443825219525,
131.409656163825));
#44141=CARTESIAN_POINT('Ctrl Pts',(-1.48667651937189,2.89412199965503E-5,
131.41254146791));
#44142=CARTESIAN_POINT('Origin',(0.,0.,131.75));
#44143=CARTESIAN_POINT('',(-1.48662482583238,6.78982369262116E-6,131.81245853209));
#44144=CARTESIAN_POINT('',(-1.48667723510369,2.90658880924576E-5,131.76254146791));
#44145=CARTESIAN_POINT('',(-1.486725,-1.82071301246235E-16,131.75));
#44146=CARTESIAN_POINT('Ctrl Pts',(-1.48662482583238,6.78982369262116E-6,
131.81245853209));
#44147=CARTESIAN_POINT('Ctrl Pts',(-1.48664372040861,0.111474600180848,
131.80828292257));
#44148=CARTESIAN_POINT('Ctrl Pts',(-1.47425429712656,0.222938274562959,
131.80410731305));
#44149=CARTESIAN_POINT('Ctrl Pts',(-1.44940874218647,0.331552605768891,
131.799931703531));
#44150=CARTESIAN_POINT('Ctrl Pts',(-1.39600463853288,0.565012917521814,
131.790956468961));
#44151=CARTESIAN_POINT('Ctrl Pts',(-1.28505189717003,0.785308964263988,
131.78198123439));
#44152=CARTESIAN_POINT('Ctrl Pts',(-1.12926191763864,0.967202333379871,
131.77300599982));
#44153=CARTESIAN_POINT('Ctrl Pts',(-0.973471938107258,1.14909570249575,
131.76403076525));
#44154=CARTESIAN_POINT('Ctrl Pts',(-0.772844720407338,1.29258639398535,
131.75505553068));
#44155=CARTESIAN_POINT('Ctrl Pts',(-0.550365300254005,1.38123526909931,
131.74608029611));
#44156=CARTESIAN_POINT('Ctrl Pts',(-0.327885880100671,1.46988414421327,
131.73710506154));
#44157=CARTESIAN_POINT('Ctrl Pts',(-0.0835542574939237,1.5036912029516,
131.72812982697));
#44158=CARTESIAN_POINT('Ctrl Pts',(0.15463749781462,1.47878330954827,131.7191545924));
#44159=CARTESIAN_POINT('Ctrl Pts',(0.392829253123164,1.45387541614494,131.710179357829));
#44160=CARTESIAN_POINT('Ctrl Pts',(0.624881141133504,1.37025257059994,131.701204123259));
#44161=CARTESIAN_POINT('Ctrl Pts',(0.824207930814637,1.23749509862122,131.692228888689));
#44162=CARTESIAN_POINT('Ctrl Pts',(1.02353472049577,1.1047376266425,131.683253654119));
#44163=CARTESIAN_POINT('Ctrl Pts',(1.1901364118477,0.922845528230054,131.674278419549));
#44164=CARTESIAN_POINT('Ctrl Pts',(1.30492613385756,0.712657433487139,131.665303184979));
#44165=CARTESIAN_POINT('Ctrl Pts',(1.41971585586741,0.502469338744224,131.656327950409));
#44166=CARTESIAN_POINT('Ctrl Pts',(1.4826936085352,0.263985247670841,131.647352715839));
#44167=CARTESIAN_POINT('Ctrl Pts',(1.48664428958854,0.0245273023653047,
131.638377481268));
#44168=CARTESIAN_POINT('Ctrl Pts',(1.49059497064187,-0.214930642940232,
131.629402246698));
#44169=CARTESIAN_POINT('Ctrl Pts',(1.43551858008075,-0.455362442477921,
131.620427012128));
#44170=CARTESIAN_POINT('Ctrl Pts',(1.32772499359706,-0.669222813196063,
131.611451777558));
#44171=CARTESIAN_POINT('Ctrl Pts',(1.21993140711338,-0.883083183914204,
131.602476542988));
#44172=CARTESIAN_POINT('Ctrl Pts',(1.05942062470712,-1.0703721258128,131.593501308418));
#44173=CARTESIAN_POINT('Ctrl Pts',(0.864581706987901,-1.20963271461242,
131.584526073848));
#44174=CARTESIAN_POINT('Ctrl Pts',(0.669742789268677,-1.34889330341204,
131.575550839278));
#44175=CARTESIAN_POINT('Ctrl Pts',(0.440575736236482,-1.44012553911268,
131.566575604708));
#44176=CARTESIAN_POINT('Ctrl Pts',(0.203335275236014,-1.47287731945189,
131.557600370137));
#44177=CARTESIAN_POINT('Ctrl Pts',(-0.033905185764455,-1.50562909979111,
131.548625135567));
#44178=CARTESIAN_POINT('Ctrl Pts',(-0.279219054733197,-1.47990042476888,
131.539649900997));
#44179=CARTESIAN_POINT('Ctrl Pts',(-0.504501729990859,-1.39863892293247,
131.530674666427));
#44180=CARTESIAN_POINT('Ctrl Pts',(-0.72978440524852,-1.31737742109606,
131.521699431857));
#44181=CARTESIAN_POINT('Ctrl Pts',(-0.9350358867951,-1.18058309244548,131.512724197287));
#44182=CARTESIAN_POINT('Ctrl Pts',(-1.09674135601336,-1.00392790096093,
131.503748962717));
#44183=CARTESIAN_POINT('Ctrl Pts',(-1.25844682523162,-0.827272709476379,
131.494773728147));
#44184=CARTESIAN_POINT('Ctrl Pts',(-1.37660628212157,-0.610756655157868,
131.485798493576));
#44185=CARTESIAN_POINT('Ctrl Pts',(-1.43768268336866,-0.379185092425305,
131.476823259006));
#44186=CARTESIAN_POINT('Ctrl Pts',(-1.4702666349111,-0.255642833473939,
131.472035016701));
#44187=CARTESIAN_POINT('Ctrl Pts',(-1.48660378638844,-0.127815522989732,
131.467246774395));
#44188=CARTESIAN_POINT('Ctrl Pts',(-1.48662467006137,6.54543500555605E-6,
131.46245853209));
#44189=CARTESIAN_POINT('Ctrl Pts',(-1.48667651937189,2.89412199965503E-5,
131.41254146791));
#44190=CARTESIAN_POINT('Ctrl Pts',(-1.48655270486754,-0.162525392751979,
131.418631398395));
#44191=CARTESIAN_POINT('Ctrl Pts',(-1.45993722594017,-0.325119310129694,
131.424721328881));
#44192=CARTESIAN_POINT('Ctrl Pts',(-1.40759092349875,-0.478957857091241,
131.430811259366));
#44193=CARTESIAN_POINT('Ctrl Pts',(-1.33044384531333,-0.705682455713139,
131.439786493936));
#44194=CARTESIAN_POINT('Ctrl Pts',(-1.19740850168767,-0.913390077844603,
131.448761728506));
#44195=CARTESIAN_POINT('Ctrl Pts',(-1.02372620542085,-1.07828451499433,
131.457736963076));
#44196=CARTESIAN_POINT('Ctrl Pts',(-0.850043909154037,-1.24317895214406,
131.466712197646));
#44197=CARTESIAN_POINT('Ctrl Pts',(-0.63571466024607,-1.36526020431205,
131.475687432216));
#44198=CARTESIAN_POINT('Ctrl Pts',(-0.405293279741281,-1.43054192405704,
131.484662666787));
#44199=CARTESIAN_POINT('Ctrl Pts',(-0.174871899236492,-1.49582364380202,
131.493637901357));
#44200=CARTESIAN_POINT('Ctrl Pts',(0.0716416128651196,-1.50430583112399,
131.502613135927));
#44201=CARTESIAN_POINT('Ctrl Pts',(0.306005216640002,-1.45501671668872,
131.511588370497));
#44202=CARTESIAN_POINT('Ctrl Pts',(0.540368820414884,-1.40572760225345,
131.520563605067));
#44203=CARTESIAN_POINT('Ctrl Pts',(0.762582515863036,-1.29866718606095,
131.529538839637));
#44204=CARTESIAN_POINT('Ctrl Pts',(0.947188193250521,-1.14610093991915,
131.538514074207));
#44205=CARTESIAN_POINT('Ctrl Pts',(1.13179387063801,-0.993534693777357,
131.547489308777));
#44206=CARTESIAN_POINT('Ctrl Pts',(1.27879152996482,-0.795462617686266,
131.556464543347));
#44207=CARTESIAN_POINT('Ctrl Pts',(1.37134025357767,-0.574577015287615,
131.565439777918));
#44208=CARTESIAN_POINT('Ctrl Pts',(1.46388897719051,-0.353691412888964,
131.574415012488));
#44209=CARTESIAN_POINT('Ctrl Pts',(1.50198876508937,-0.109992284182755,
131.583390247058));
#44210=CARTESIAN_POINT('Ctrl Pts',(1.48127468117422,0.128600763314322,131.592365481628));
#44211=CARTESIAN_POINT('Ctrl Pts',(1.46056059725906,0.367193810811399,131.601340716198));
#44212=CARTESIAN_POINT('Ctrl Pts',(1.38103264152987,0.600680777099344,131.610315950768));
#44213=CARTESIAN_POINT('Ctrl Pts',(1.25180200499627,0.802312020128169,131.619291185338));
#44214=CARTESIAN_POINT('Ctrl Pts',(1.12257136846268,1.00394326315699,131.628266419908));
#44215=CARTESIAN_POINT('Ctrl Pts',(0.943638051124673,1.1737187829267,131.637241654478));
#44216=CARTESIAN_POINT('Ctrl Pts',(0.73550170769923,1.29218809594964,131.646216889049));
#44217=CARTESIAN_POINT('Ctrl Pts',(0.527365364273789,1.41065740897258,131.655192123619));
#44218=CARTESIAN_POINT('Ctrl Pts',(0.29002599476091,1.47782051524875,131.664167358189));
#44219=CARTESIAN_POINT('Ctrl Pts',(0.0506745952140745,1.48598281374583,
131.673142592759));
#44220=CARTESIAN_POINT('Ctrl Pts',(-0.188676804332765,1.4941451122429,131.682117827329));
#44221=CARTESIAN_POINT('Ctrl Pts',(-0.430040233913561,1.44330660296088,
131.691093061899));
#44222=CARTESIAN_POINT('Ctrl Pts',(-0.645763677451843,1.3392916449525,131.700068296469));
#44223=CARTESIAN_POINT('Ctrl Pts',(-0.861487120990125,1.23527668694413,
131.709043531039));
#44224=CARTESIAN_POINT('Ctrl Pts',(-1.05157057848589,1.07808528020941,131.71801876561));
#44225=CARTESIAN_POINT('Ctrl Pts',(-1.19423696949397,0.885726198130794,
131.72699400018));
#44226=CARTESIAN_POINT('Ctrl Pts',(-1.33690336050205,0.693367116052179,
131.73596923475));
#44227=CARTESIAN_POINT('Ctrl Pts',(-1.43215268502245,0.465840358629668,
131.74494446932));
#44228=CARTESIAN_POINT('Ctrl Pts',(-1.46907261943811,0.22921273128206,131.75391970389));
#44229=CARTESIAN_POINT('Ctrl Pts',(-1.48089459317689,0.153443214335519,
131.75679362523));
#44230=CARTESIAN_POINT('Ctrl Pts',(-1.4867359556546,0.0767405697656338,
131.75966754657));
#44231=CARTESIAN_POINT('Ctrl Pts',(-1.48667723510369,2.90658880924576E-5,
131.76254146791));
#44232=CARTESIAN_POINT('Origin',(0.,0.,131.75));
#44233=CARTESIAN_POINT('',(-1.48662495810528,7.0294833549589E-6,132.16245853209));
#44234=CARTESIAN_POINT('',(-1.48667795283619,2.91850407830213E-5,132.11254146791));
#44235=CARTESIAN_POINT('',(-1.486725,-1.82071301246235E-16,131.75));
#44236=CARTESIAN_POINT('Ctrl Pts',(-1.48662495810528,7.0294833549589E-6,
132.16245853209));
#44237=CARTESIAN_POINT('Ctrl Pts',(-1.48664448474531,0.111170943043426,
132.158294305315));
#44238=CARTESIAN_POINT('Ctrl Pts',(-1.47432311674833,0.222330594316862,
132.15413007854));
#44239=CARTESIAN_POINT('Ctrl Pts',(-1.44961170010174,0.330664011192151,
132.149965851765));
#44240=CARTESIAN_POINT('Ctrl Pts',(-1.3963507292296,0.564157017408393,132.140990617195));
#44241=CARTESIAN_POINT('Ctrl Pts',(-1.28553305875945,0.784521041741841,
132.132015382625));
#44242=CARTESIAN_POINT('Ctrl Pts',(-1.12985461636972,0.966509881058128,
132.123040148055));
#44243=CARTESIAN_POINT('Ctrl Pts',(-0.974176173979993,1.14849872037442,
132.114064913485));
#44244=CARTESIAN_POINT('Ctrl Pts',(-0.773636959670693,1.29211237467355,
132.105089678915));
#44245=CARTESIAN_POINT('Ctrl Pts',(-0.551211926840969,1.38089761924403,
132.096114444345));
#44246=CARTESIAN_POINT('Ctrl Pts',(-0.328786894011251,1.46968286381452,
132.087139209774));
#44247=CARTESIAN_POINT('Ctrl Pts',(-0.0844760426611109,1.50363969865637,
132.078163975204));
#44248=CARTESIAN_POINT('Ctrl Pts',(0.153730936532854,1.47887782825435,132.069188740634));
#44249=CARTESIAN_POINT('Ctrl Pts',(0.391937915726826,1.45411595785233,132.060213506064));
#44250=CARTESIAN_POINT('Ctrl Pts',(0.624041022764623,1.37063538220644,132.051238271494));
#44251=CARTESIAN_POINT('Ctrl Pts',(0.823449158655619,1.23800012803382,132.042263036924));
#44252=CARTESIAN_POINT('Ctrl Pts',(1.02285729454661,1.1053648738612,132.033287802354));
#44253=CARTESIAN_POINT('Ctrl Pts',(1.1895704592908,0.92357494116184,132.024312567784));
#44254=CARTESIAN_POINT('Ctrl Pts',(1.30448901068812,0.713457255231484,132.015337333214));
#44255=CARTESIAN_POINT('Ctrl Pts',(1.41940756208544,0.503339569301124,132.006362098643));
#44256=CARTESIAN_POINT('Ctrl Pts',(1.48253150013589,0.264894130139772,131.997386864073));
#44257=CARTESIAN_POINT('Ctrl Pts',(1.48662897469899,0.025438651714869,131.988411629503));
#44258=CARTESIAN_POINT('Ctrl Pts',(1.49072644926209,-0.214016826710032,
131.979436394933));
#44259=CARTESIAN_POINT('Ctrl Pts',(1.43579746033784,-0.454482344398475,
131.970461160363));
#44260=CARTESIAN_POINT('Ctrl Pts',(1.32813499638598,-0.668408755368728,
131.961485925793));
#44261=CARTESIAN_POINT('Ctrl Pts',(1.22047253243412,-0.882335166338984,
131.952510691223));
#44262=CARTESIAN_POINT('Ctrl Pts',(1.06007659345464,-1.06972247059105,131.943535456653));
#44263=CARTESIAN_POINT('Ctrl Pts',(0.865323082913764,-1.20910247486244,
131.934560222082));
#44264=CARTESIAN_POINT('Ctrl Pts',(0.670569572372892,-1.34848247913384,
131.925584987512));
#44265=CARTESIAN_POINT('Ctrl Pts',(0.441458490270625,-1.43985518342455,
131.916609752942));
#44266=CARTESIAN_POINT('Ctrl Pts',(0.20423815158461,-1.4727523925674,131.907634518372));
#44267=CARTESIAN_POINT('Ctrl Pts',(-0.0329821871014054,-1.50564960171024,
131.898659283802));
#44268=CARTESIAN_POINT('Ctrl Pts',(-0.27831178237117,-1.4800713157052,131.889684049232));
#44269=CARTESIAN_POINT('Ctrl Pts',(-0.50364423084838,-1.39894793364549,
131.880708814662));
#44270=CARTESIAN_POINT('Ctrl Pts',(-0.728976679325591,-1.31782455158578,
131.871733580092));
#44271=CARTESIAN_POINT('Ctrl Pts',(-0.934311981010247,-1.18115607347139,
131.862758345521));
#44272=CARTESIAN_POINT('Ctrl Pts',(-1.09612571435821,-1.0046000451066,131.853783110951));
#44273=CARTESIAN_POINT('Ctrl Pts',(-1.25793944770617,-0.828044016741798,
131.844807876381));
#44274=CARTESIAN_POINT('Ctrl Pts',(-1.37623161271745,-0.611600438126588,
131.835832641811));
#44275=CARTESIAN_POINT('Ctrl Pts',(-1.43744996225092,-0.380066360437146,
131.826857407241));
#44276=CARTESIAN_POINT('Ctrl Pts',(-1.47018728200171,-0.256250458958468,
131.822057782191));
#44277=CARTESIAN_POINT('Ctrl Pts',(-1.48660310759437,-0.12811910230264,
131.81725815714));
#44278=CARTESIAN_POINT('Ctrl Pts',(-1.48662482583238,6.78982369262116E-6,
131.81245853209));
#44279=CARTESIAN_POINT('Ctrl Pts',(-1.48667723510369,2.90658880924576E-5,
131.76254146791));
#44280=CARTESIAN_POINT('Ctrl Pts',(-1.48655257181903,-0.162828875630418,
131.76864278114));
#44281=CARTESIAN_POINT('Ctrl Pts',(-1.45983566302084,-0.325726746906379,
131.77474409437));
#44282=CARTESIAN_POINT('Ctrl Pts',(-1.4072970457122,-0.479820656595399,
131.7808454076));
#44283=CARTESIAN_POINT('Ctrl Pts',(-1.3300109932597,-0.706497919852542,
131.789820642171));
#44284=CARTESIAN_POINT('Ctrl Pts',(-1.19684834404377,-0.914123949094121,
131.798795876741));
#44285=CARTESIAN_POINT('Ctrl Pts',(-1.02306499546073,-1.07891188353324,
131.807771111311));
#44286=CARTESIAN_POINT('Ctrl Pts',(-0.849281646877681,-1.24369981797236,
131.816746345881));
#44287=CARTESIAN_POINT('Ctrl Pts',(-0.634877598927511,-1.36564965760903,
131.825721580451));
#44288=CARTESIAN_POINT('Ctrl Pts',(-0.404416242141579,-1.43079011055361,
131.834696815021));
#44289=CARTESIAN_POINT('Ctrl Pts',(-0.173954885355643,-1.49593056349819,
131.843672049591));
#44290=CARTESIAN_POINT('Ctrl Pts',(0.072563780266055,-1.50426162975068,
131.852647284161));
#44291=CARTESIAN_POINT('Ctrl Pts',(0.306897124442854,-1.4548288532928,131.861622518732));
#44292=CARTESIAN_POINT('Ctrl Pts',(0.54123046861965,-1.40539607683492,131.870597753302));
#44293=CARTESIAN_POINT('Ctrl Pts',(0.763378491351546,-1.29819945766667,
131.879572987872));
#44294=CARTESIAN_POINT('Ctrl Pts',(0.947890606745602,-1.14552007184721,
131.888548222442));
#44295=CARTESIAN_POINT('Ctrl Pts',(1.13240272213966,-0.992840686027748,
131.897523457012));
#44296=CARTESIAN_POINT('Ctrl Pts',(1.27927893019587,-0.794678533557074,
131.906498691582));
#44297=CARTESIAN_POINT('Ctrl Pts',(1.37169222744692,-0.573736237758631,
131.915473926152));
#44298=CARTESIAN_POINT('Ctrl Pts',(1.46410552469796,-0.352793941960185,
131.924449160722));
#44299=CARTESIAN_POINT('Ctrl Pts',(1.50205591114383,-0.109071502833969,
131.933424395292));
#44300=CARTESIAN_POINT('Ctrl Pts',(1.48119556699242,0.129508801515888,131.942399629863));
#44301=CARTESIAN_POINT('Ctrl Pts',(1.46033522284101,0.368089105865746,131.951374864433));
#44302=CARTESIAN_POINT('Ctrl Pts',(1.38066414809232,0.601527275439246,131.960350099003));
#44303=CARTESIAN_POINT('Ctrl Pts',(1.25130993031637,0.803079258625255,131.969325333573));
#44304=CARTESIAN_POINT('Ctrl Pts',(1.12195571254041,1.00463124181126,131.978300568143));
#44305=CARTESIAN_POINT('Ctrl Pts',(0.942918351737199,1.17429703860978,131.987275802713));
#44306=CARTESIAN_POINT('Ctrl Pts',(0.734709422453624,1.29263873604062,131.996251037283));
#44307=CARTESIAN_POINT('Ctrl Pts',(0.526500493170048,1.41098043347147,132.005226271853));
#44308=CARTESIAN_POINT('Ctrl Pts',(0.289119995406113,1.47799803153465,132.014201506424));
#44309=CARTESIAN_POINT('Ctrl Pts',(0.0497636371096859,1.48601359947829,
132.023176740994));
#44310=CARTESIAN_POINT('Ctrl Pts',(-0.189592721186742,1.49402916742193,
132.032151975564));
#44311=CARTESIAN_POINT('Ctrl Pts',(-0.430924940015661,1.44304270524602,
132.041127210134));
#44312=CARTESIAN_POINT('Ctrl Pts',(-0.646584578996447,1.33889552235537,
132.050102444704));
#44313=CARTESIAN_POINT('Ctrl Pts',(-0.862244217977232,1.23474833946472,
132.059077679274));
#44314=CARTESIAN_POINT('Ctrl Pts',(-1.05223127710988,1.07744043585933,132.068052913844));
#44315=CARTESIAN_POINT('Ctrl Pts',(-1.1947797199153,0.88499393150229,132.077028148414));
#44316=CARTESIAN_POINT('Ctrl Pts',(-1.33732816272071,0.692547427145254,
132.086003382984));
#44317=CARTESIAN_POINT('Ctrl Pts',(-1.43243798919889,0.46496232203658,132.094978617555));
#44318=CARTESIAN_POINT('Ctrl Pts',(-1.46921285748553,0.228312106235572,
132.103953852125));
#44319=CARTESIAN_POINT('Ctrl Pts',(-1.48094174088988,0.152835485432742,
132.10681639072));
#44320=CARTESIAN_POINT('Ctrl Pts',(-1.48673672765572,0.0764367515174225,
132.109678929315));
#44321=CARTESIAN_POINT('Ctrl Pts',(-1.48667795283619,2.91850407830213E-5,
132.11254146791));
#44322=CARTESIAN_POINT('Origin',(0.,0.,131.75));
#44323=CARTESIAN_POINT('',(-1.486725,-1.82071301246235E-16,132.5));
#44324=CARTESIAN_POINT('',(-1.48668131839924,3.04819389219259E-5,132.46254146791));
#44325=CARTESIAN_POINT('',(-1.486725,-1.82071301246235E-16,131.75));
#44326=CARTESIAN_POINT('',(-1.44969557651742,0.329748329868144,132.5));
#44327=CARTESIAN_POINT('Origin',(0.,0.,132.5));
#44328=CARTESIAN_POINT('Ctrl Pts',(-1.44969557651734,0.329748329868494,
132.5));
#44329=CARTESIAN_POINT('Ctrl Pts',(-1.39656552507766,0.563327679862336,
132.49102476543));
#44330=CARTESIAN_POINT('Ctrl Pts',(-1.28592745851384,0.783721236611964,
132.48204953086));
#44331=CARTESIAN_POINT('Ctrl Pts',(-1.1303829541632,0.965796406696618,132.47307429629));
#44332=CARTESIAN_POINT('Ctrl Pts',(-0.974838449812451,1.1478715767814,132.46409906172));
#44333=CARTESIAN_POINT('Ctrl Pts',(-0.774387507674821,1.29162836020115,
132.455123827149));
#44334=CARTESIAN_POINT('Ctrl Pts',(-0.552021890034789,1.38055646740327,
132.446148592579));
#44335=CARTESIAN_POINT('Ctrl Pts',(-0.329656272394756,1.46948457460539,
132.437173358009));
#44336=CARTESIAN_POINT('Ctrl Pts',(-0.0853759792523218,1.50358400558988,
132.428198123439));
#44337=CARTESIAN_POINT('Ctrl Pts',(0.152840964869851,1.47896668523315,132.419222888869));
#44338=CARTESIAN_POINT('Ctrl Pts',(0.39105790899202,1.45434936487643,132.410247654299));
#44339=CARTESIAN_POINT('Ctrl Pts',(0.623211504093927,1.3710152931785,132.401272419729));
#44340=CARTESIAN_POINT('Ctrl Pts',(0.82269945647758,1.23850370981599,132.392297185159));
#44341=CARTESIAN_POINT('Ctrl Pts',(1.02218740886124,1.10599212645348,132.383321950588));
#44342=CARTESIAN_POINT('Ctrl Pts',(1.18900971852664,0.924303031426379,132.374346716018));
#44343=CARTESIAN_POINT('Ctrl Pts',(1.3040557817562,0.714255576485402,132.365371481448));
#44344=CARTESIAN_POINT('Ctrl Pts',(1.41910184498576,0.504208121544427,132.356396246878));
#44345=CARTESIAN_POINT('Ctrl Pts',(1.48237166177948,0.265802306689577,132.347421012308));
#44346=CARTESIAN_POINT('Ctrl Pts',(1.48661551803772,0.0263496923375517,
132.338445777738));
#44347=CARTESIAN_POINT('Ctrl Pts',(1.49085937429597,-0.21310292201447,132.329470543168));
#44348=CARTESIAN_POINT('Ctrl Pts',(1.43607727001874,-0.453602335863666,
132.320495308598));
#44349=CARTESIAN_POINT('Ctrl Pts',(1.32854565172172,-0.667594747419045,
132.311520074027));
#44350=CARTESIAN_POINT('Ctrl Pts',(1.2210140334247,-0.881587158974429,132.302544839457));
#44351=CARTESIAN_POINT('Ctrl Pts',(1.06073290110789,-1.069072568236,132.293569604887));
#44352=CARTESIAN_POINT('Ctrl Pts',(0.866064757738101,-1.20857186741508,
132.284594370317));
#44353=CARTESIAN_POINT('Ctrl Pts',(0.671396614368315,-1.34807116659416,
132.275619135747));
#44354=CARTESIAN_POINT('Ctrl Pts',(0.442341459945558,-1.43958435569076,
132.266643901177));
#44355=CARTESIAN_POINT('Ctrl Pts',(0.20514125304273,-1.47262698657398,132.257668666607));
#44356=CARTESIAN_POINT('Ctrl Pts',(-0.0320589538600982,-1.5056696174572,
132.248693432037));
#44357=CARTESIAN_POINT('Ctrl Pts',(-0.277404213242995,-1.48024169012703,
132.239718197467));
#44358=CARTESIAN_POINT('Ctrl Pts',(-0.50278638102289,-1.399256442972,132.230742962896));
#44359=CARTESIAN_POINT('Ctrl Pts',(-0.728168548802785,-1.31827119581697,
132.221767728326));
#44360=CARTESIAN_POINT('Ctrl Pts',(-0.933587624979677,-1.18172862883706,
132.212792493756));
#44361=CARTESIAN_POINT('Ctrl Pts',(-1.09550958179572,-1.00527183024128,
132.203817259186));
#44362=CARTESIAN_POINT('Ctrl Pts',(-1.25743153861176,-0.828815031645493,
132.194842024616));
#44363=CARTESIAN_POINT('Ctrl Pts',(-1.37585637606696,-0.612444001433831,
132.185866790046));
#44364=CARTESIAN_POINT('Ctrl Pts',(-1.43721665915749,-0.38094749227848,
132.176891555476));
#44365=CARTESIAN_POINT('Ctrl Pts',(-1.47010769927003,-0.256858088106286,
132.172080547681));
#44366=CARTESIAN_POINT('Ctrl Pts',(-1.48660239861885,-0.128422684745344,
132.167269539885));
#44367=CARTESIAN_POINT('Ctrl Pts',(-1.48662495810528,7.0294833549589E-6,
132.16245853209));
#44368=CARTESIAN_POINT('Ctrl Pts',(-1.48667795283619,2.91850407830213E-5,
132.11254146791));
#44369=CARTESIAN_POINT('Ctrl Pts',(-1.48655244444886,-0.163132361450183,
132.118654163885));
#44370=CARTESIAN_POINT('Ctrl Pts',(-1.4597339032395,-0.326334184239694,
132.12476685986));
#44371=CARTESIAN_POINT('Ctrl Pts',(-1.40700263865445,-0.480683278165215,
132.130879555835));
#44372=CARTESIAN_POINT('Ctrl Pts',(-1.32957764144165,-0.707313120271662,
132.139854790405));
#44373=CARTESIAN_POINT('Ctrl Pts',(-1.19628773692095,-0.914857477991214,
132.148830024975));
#44374=CARTESIAN_POINT('Ctrl Pts',(-1.02240340176009,-1.07953884738407,
132.157805259545));
#44375=CARTESIAN_POINT('Ctrl Pts',(-0.848519066599234,-1.24422021677693,
132.166780494116));
#44376=CARTESIAN_POINT('Ctrl Pts',(-0.634040300798227,-1.3660385978431,
132.175755728686));
#44377=CARTESIAN_POINT('Ctrl Pts',(-0.403539054962874,-1.43103775907736,
132.184730963256));
#44378=CARTESIAN_POINT('Ctrl Pts',(-0.173037809127522,-1.49603692031162,
132.193706197826));
#44379=CARTESIAN_POINT('Ctrl Pts',(0.0734859167421764,-1.50421686171398,
132.202681432396));
#44380=CARTESIAN_POINT('Ctrl Pts',(0.307788911951766,-1.45464044142533,
132.211656666966));
#44381=CARTESIAN_POINT('Ctrl Pts',(0.542091907161356,-1.40506402113668,
132.220631901536));
#44382=CARTESIAN_POINT('Ctrl Pts',(0.764174171710838,-1.29773123915701,
132.229607136106));
#44383=CARTESIAN_POINT('Ctrl Pts',(0.948592653714135,-1.14493876981965,
132.238582370677));
#44384=CARTESIAN_POINT('Ctrl Pts',(1.13301113571743,-0.992146300482294,
132.247557605247));
#44385=CARTESIAN_POINT('Ctrl Pts',(1.27976583517455,-0.793894143787234,
132.256532839817));
#44386=CARTESIAN_POINT('Ctrl Pts',(1.37204366629816,-0.572895236586572,
132.265508074387));
#44387=CARTESIAN_POINT('Ctrl Pts',(1.46432149742177,-0.35189632938591,132.274483308957));
#44388=CARTESIAN_POINT('Ctrl Pts',(1.50212246021187,-0.108150671679646,
132.283458543527));
#44389=CARTESIAN_POINT('Ctrl Pts',(1.4811158560996,0.130416804746358,132.292433778097));
#44390=CARTESIAN_POINT('Ctrl Pts',(1.46010925198732,0.368984281172361,132.301409012667));
#44391=CARTESIAN_POINT('Ctrl Pts',(1.38029508097267,0.602373576318102,132.310384247238));
#44392=CARTESIAN_POINT('Ctrl Pts',(1.25081731064699,0.803846227062567,132.319359481808));
#44393=CARTESIAN_POINT('Ctrl Pts',(1.12133954032132,1.00531887780703,132.328334716378));
#44394=CARTESIAN_POINT('Ctrl Pts',(0.942198170684623,1.17487488415022,132.337309950948));
#44395=CARTESIAN_POINT('Ctrl Pts',(0.733916706066377,1.29308894190268,132.346285185518));
#44396=CARTESIAN_POINT('Ctrl Pts',(0.525635241448134,1.41130299965514,132.355260420088));
#44397=CARTESIAN_POINT('Ctrl Pts',(0.288213681848343,1.47817510881686,132.364235654658));
#44398=CARTESIAN_POINT('Ctrl Pts',(0.0488523752928705,1.48604395157025,
132.373210889228));
#44399=CARTESIAN_POINT('Ctrl Pts',(-0.190508931262602,1.49391279432363,
132.382186123798));
#44400=CARTESIAN_POINT('Ctrl Pts',(-0.431809984773757,1.44277837066867,
132.391161358369));
#44401=CARTESIAN_POINT('Ctrl Pts',(-0.647405838147634,1.33849908854363,
132.400136592939));
#44402=CARTESIAN_POINT('Ctrl Pts',(-0.863001691521512,1.23421980641859,
132.409111827509));
#44403=CARTESIAN_POINT('Ctrl Pts',(-1.05289234475811,1.07679566582346,132.418087062079));
#44404=CARTESIAN_POINT('Ctrl Pts',(-1.19532310554678,0.884261825513106,
132.427062296649));
#44405=CARTESIAN_POINT('Ctrl Pts',(-1.33775386633544,0.691727985202751,
132.436037531219));
#44406=CARTESIAN_POINT('Ctrl Pts',(-1.43272473467618,0.46408444517717,132.445012765789));
#44407=CARTESIAN_POINT('Ctrl Pts',(-1.46935487513581,0.227412102571081,
132.453988000359));
#44408=CARTESIAN_POINT('Ctrl Pts',(-1.48099114363096,0.152228581858804,
132.45683915621));
#44409=CARTESIAN_POINT('Ctrl Pts',(-1.48674003111915,0.0761339309162625,
132.45969031206));
#44410=CARTESIAN_POINT('Ctrl Pts',(-1.48668131839924,3.04819389219259E-5,
132.46254146791));
#44411=CARTESIAN_POINT('Origin',(0.,0.,130.353000754712));
#44412=CARTESIAN_POINT('',(-1.28651342453934,6.08325872239859E-6,132.278000754712));
#44413=CARTESIAN_POINT('',(-1.28656219828984,2.63788275486898E-5,132.346999245288));
#44414=CARTESIAN_POINT('',(-1.2866,7.40115670650129E-15,130.353000754712));
#44415=CARTESIAN_POINT('',(0.855148668267089,0.961251009262055,132.5));
#44416=CARTESIAN_POINT('Ctrl Pts',(-1.28651342453934,6.08325872233223E-6,
132.278000754712));
#44417=CARTESIAN_POINT('Ctrl Pts',(-1.28649390173904,-0.11113597080406,
132.282811762507));
#44418=CARTESIAN_POINT('Ctrl Pts',(-1.24558977217514,-0.429634554413405,
132.296598004872));
#44419=CARTESIAN_POINT('Ctrl Pts',(-0.98568734749738,-0.904495711840062,
132.319359481808));
#44420=CARTESIAN_POINT('Ctrl Pts',(-0.452383239321647,-1.25898426892294,
132.346285185518));
#44421=CARTESIAN_POINT('Ctrl Pts',(0.184576273813673,-1.32499964763048,
132.373210889228));
#44422=CARTESIAN_POINT('Ctrl Pts',(0.779243804823753,-1.08741528786317,
132.400136592939));
#44423=CARTESIAN_POINT('Ctrl Pts',(1.19536185928334,-0.600670138176585,
132.427062296649));
#44424=CARTESIAN_POINT('Ctrl Pts',(1.33758585234813,0.0237087063139161,
132.453988000359));
#44425=CARTESIAN_POINT('Ctrl Pts',(1.18926763353383,0.582583816218694,132.478300568143));
#44426=CARTESIAN_POINT('Ctrl Pts',(0.964859291222552,0.863480253952869,
132.493637901357));
#44427=CARTESIAN_POINT('Ctrl Pts',(0.855148668267089,0.961251009262055,
132.5));
#44428=CARTESIAN_POINT('',(1.18756226708949,-0.495010526943903,132.5));
#44429=CARTESIAN_POINT('Origin',(0.,0.,132.5));
#44430=CARTESIAN_POINT('Ctrl Pts',(-1.28656219828984,2.63788275487037E-5,
132.346999245288));
#44431=CARTESIAN_POINT('Ctrl Pts',(-1.28645306307448,-0.141434727128406,
132.353123324008));
#44432=CARTESIAN_POINT('Ctrl Pts',(-1.22901431635415,-0.490302866316248,
132.368222637298));
#44433=CARTESIAN_POINT('Ctrl Pts',(-0.919323220327711,-0.971881421552252,
132.392297185159));
#44434=CARTESIAN_POINT('Ctrl Pts',(-0.362304579342239,-1.28779095308542,
132.419222888869));
#44435=CARTESIAN_POINT('Ctrl Pts',(0.277699363289323,-1.30864921194912,
132.446148592579));
#44436=CARTESIAN_POINT('Ctrl Pts',(0.85410155756253,-1.02958919072608,132.47307429629));
#44437=CARTESIAN_POINT('Ctrl Pts',(1.10780466901396,-0.686354162750902,
132.49102476543));
#44438=CARTESIAN_POINT('Ctrl Pts',(1.18756226708949,-0.495010526943894,
132.5));
#44439=CARTESIAN_POINT('Origin',(0.,0.,130.353000754712));
#44440=CARTESIAN_POINT('',(-1.28651331007142,5.8758598133296E-6,131.928000754712));
#44441=CARTESIAN_POINT('',(-1.28655928575833,2.52565028640017E-5,131.996999245288));
#44442=CARTESIAN_POINT('',(-1.2866,7.40115670650129E-15,130.353000754712));
#44443=CARTESIAN_POINT('Ctrl Pts',(-1.28651331007142,5.87585981328548E-6,
131.928000754712));
#44444=CARTESIAN_POINT('Ctrl Pts',(-1.28649451528088,-0.110873252970274,
131.932800379762));
#44445=CARTESIAN_POINT('Ctrl Pts',(-1.24572312673905,-0.429108439932022,
131.946575239382));
#44446=CARTESIAN_POINT('Ctrl Pts',(-0.986241701669955,-0.903891264481546,
131.969325333573));
#44447=CARTESIAN_POINT('Ctrl Pts',(-0.453155086833697,-1.25870670904991,
131.996251037283));
#44448=CARTESIAN_POINT('Ctrl Pts',(0.183763759504555,-1.32511244536446,
132.023176740994));
#44449=CARTESIAN_POINT('Ctrl Pts',(0.778576488622803,-1.08789280890088,
132.050102444704));
#44450=CARTESIAN_POINT('Ctrl Pts',(1.1949926014029,-0.601402357101034,132.077028148414));
#44451=CARTESIAN_POINT('Ctrl Pts',(1.3375979328864,0.02288848698503,132.103953852125));
#44452=CARTESIAN_POINT('Ctrl Pts',(1.17371706985718,0.641934851359759,132.130879555835));
#44453=CARTESIAN_POINT('Ctrl Pts',(0.740900326155663,1.11389354058136,132.157805259545));
#44454=CARTESIAN_POINT('Ctrl Pts',(0.138319773232647,1.3306238208134,132.184730963256));
#44455=CARTESIAN_POINT('Ctrl Pts',(-0.495954234429353,1.24246589576165,
132.211656666966));
#44456=CARTESIAN_POINT('Ctrl Pts',(-1.01658936156519,0.869619550362351,
132.238582370677));
#44457=CARTESIAN_POINT('Ctrl Pts',(-1.25288574974687,0.399737600901963,
132.260697066592));
#44458=CARTESIAN_POINT('Ctrl Pts',(-1.28653032273847,0.0962064506343579,
132.273836527937));
#44459=CARTESIAN_POINT('Ctrl Pts',(-1.28651342453934,6.08325872233223E-6,
132.278000754712));
#44460=CARTESIAN_POINT('Ctrl Pts',(-1.28655928575833,2.52565028640434E-5,
131.996999245288));
#44461=CARTESIAN_POINT('Ctrl Pts',(-1.28645067179739,-0.14117344918617,
132.003111941263));
#44462=CARTESIAN_POINT('Ctrl Pts',(-1.22916514203553,-0.489779393246562,
132.018199871809));
#44463=CARTESIAN_POINT('Ctrl Pts',(-0.919909876517952,-0.971317628899406,
132.042263036924));
#44464=CARTESIAN_POINT('Ctrl Pts',(-0.363085218132085,-1.28757960555225,
132.069188740634));
#44465=CARTESIAN_POINT('Ctrl Pts',(0.276933801600455,-1.30881617440312,
132.096114444345));
#44466=CARTESIAN_POINT('Ctrl Pts',(0.853498482162152,-1.0301613647476,132.123040148055));
#44467=CARTESIAN_POINT('Ctrl Pts',(1.23449953411498,-0.51546384206413,132.149965851765));
#44468=CARTESIAN_POINT('Ctrl Pts',(1.33263749249817,0.117342823334407,132.176891555476));
#44469=CARTESIAN_POINT('Ctrl Pts',(1.125425844559,0.72326254715928,132.203817259186));
#44470=CARTESIAN_POINT('Ctrl Pts',(0.660343291616316,1.16345980844394,132.230742962896));
#44471=CARTESIAN_POINT('Ctrl Pts',(0.0439550989490249,1.33707158395214,
132.257668666607));
#44472=CARTESIAN_POINT('Ctrl Pts',(-0.582504943319958,1.20431761235457,
132.284594370317));
#44473=CARTESIAN_POINT('Ctrl Pts',(-1.07549453007113,0.795616811689296,
132.311520074027));
#44474=CARTESIAN_POINT('Ctrl Pts',(-1.2659768915234,0.339033863349242,132.332321699018));
#44475=CARTESIAN_POINT('Ctrl Pts',(-1.28661300781106,0.065885698778665,
132.344148089438));
#44476=CARTESIAN_POINT('Ctrl Pts',(-1.28656219828984,2.63788275487037E-5,
132.346999245288));
#44477=CARTESIAN_POINT('Origin',(0.,0.,130.353000754712));
#44478=CARTESIAN_POINT('',(-1.28651317526843,5.66436777652892E-6,131.578000754712));
#44479=CARTESIAN_POINT('',(-1.28655866463832,2.51533884142174E-5,131.646999245288));
#44480=CARTESIAN_POINT('',(-1.2866,7.40115670650129E-15,130.353000754712));
#44481=CARTESIAN_POINT('Ctrl Pts',(-1.28651317526843,5.66436777649226E-6,
131.578000754712));
#44482=CARTESIAN_POINT('Ctrl Pts',(-1.28649510270387,-0.110610537845435,
131.582788997017));
#44483=CARTESIAN_POINT('Ctrl Pts',(-1.24585626516315,-0.428582328169219,
131.596552473893));
#44484=CARTESIAN_POINT('Ctrl Pts',(-0.986795626701916,-0.903286501201301,
131.619291185338));
#44485=CARTESIAN_POINT('Ctrl Pts',(-0.453926623709776,-1.25842867593135,
131.646216889049));
#44486=CARTESIAN_POINT('Ctrl Pts',(0.182951394380693,-1.3252248486269,131.673142592759));
#44487=CARTESIAN_POINT('Ctrl Pts',(0.777909433892818,-1.08836989336796,
131.700068296469));
#44488=CARTESIAN_POINT('Ctrl Pts',(1.19462370043953,-0.602134807565142,
131.72699400018));
#44489=CARTESIAN_POINT('Ctrl Pts',(1.33761171253848,0.0220684982618089,
131.75391970389));
#44490=CARTESIAN_POINT('Ctrl Pts',(1.17411037251451,0.641215209809031,131.7808454076));
#44491=CARTESIAN_POINT('Ctrl Pts',(0.741583033376361,1.11343913921922,131.807771111311));
#44492=CARTESIAN_POINT('Ctrl Pts',(0.139135454071305,1.33053877717148,131.834696815021));
#44493=CARTESIAN_POINT('Ctrl Pts',(-0.495192479431881,1.24276969726887,
131.861622518732));
#44494=CARTESIAN_POINT('Ctrl Pts',(-1.01605607887236,0.870242584984128,
131.888548222442));
#44495=CARTESIAN_POINT('Ctrl Pts',(-1.25276225187591,0.400263803823439,
131.910674301102));
#44496=CARTESIAN_POINT('Ctrl Pts',(-1.28652966128751,0.0964692331083593,
131.923825145192));
#44497=CARTESIAN_POINT('Ctrl Pts',(-1.28651331007142,5.87585981328548E-6,
131.928000754712));
#44498=CARTESIAN_POINT('Ctrl Pts',(-1.28655866463832,2.51533884142105E-5,
131.646999245288));
#44499=CARTESIAN_POINT('Ctrl Pts',(-1.28645078202246,-0.140910814969984,
131.653100558519));
#44500=CARTESIAN_POINT('Ctrl Pts',(-1.22931900951945,-0.489253663809912,
131.668177106319));
#44501=CARTESIAN_POINT('Ctrl Pts',(-0.920505147196365,-0.970753516707333,
131.692228888689));
#44502=CARTESIAN_POINT('Ctrl Pts',(-0.363874469513489,-1.2873567829668,
131.7191545924));
#44503=CARTESIAN_POINT('Ctrl Pts',(0.276131412923829,-1.30898569855063,
131.74608029611));
#44504=CARTESIAN_POINT('Ctrl Pts',(0.852866813310974,-1.03068439153984,
131.77300599982));
#44505=CARTESIAN_POINT('Ctrl Pts',(1.23418332299191,-0.516220535677922,
131.799931703531));
#44506=CARTESIAN_POINT('Ctrl Pts',(1.33270921150778,0.116525850196642,131.826857407241));
#44507=CARTESIAN_POINT('Ctrl Pts',(1.12586906668276,0.722572460645641,131.853783110951));
#44508=CARTESIAN_POINT('Ctrl Pts',(0.661056538993872,1.16305475729291,131.880708814662));
#44509=CARTESIAN_POINT('Ctrl Pts',(0.0447749500858785,1.33704424761847,
131.907634518372));
#44510=CARTESIAN_POINT('Ctrl Pts',(-0.581766002838075,1.20467441008527,
131.934560222082));
#44511=CARTESIAN_POINT('Ctrl Pts',(-1.07500587627816,0.796275381121529,
131.961485925793));
#44512=CARTESIAN_POINT('Ctrl Pts',(-1.26587133036338,0.339559855102084,
131.982298933528));
#44513=CARTESIAN_POINT('Ctrl Pts',(-1.28661014902004,0.0661477573208332,
131.994136706693));
#44514=CARTESIAN_POINT('Ctrl Pts',(-1.28655928575833,2.52565028640434E-5,
131.996999245288));
#44515=CARTESIAN_POINT('Origin',(0.,0.,130.353000754712));
#44516=CARTESIAN_POINT('',(-1.28651324097226,5.80358258384201E-6,131.228000754712));
#44517=CARTESIAN_POINT('',(-1.28655804524971,2.50455016348461E-5,131.296999245288));
#44518=CARTESIAN_POINT('',(-1.2866,7.40115670650129E-15,130.353000754712));
#44519=CARTESIAN_POINT('Ctrl Pts',(-1.28651324097226,5.80358258382013E-6,
131.228000754712));
#44520=CARTESIAN_POINT('Ctrl Pts',(-1.28649587088415,-0.110347520289303,
131.232777614272));
#44521=CARTESIAN_POINT('Ctrl Pts',(-1.24598938676408,-0.428056057830857,
131.246529708403));
#44522=CARTESIAN_POINT('Ctrl Pts',(-0.98734923478118,-0.902681268882645,
131.269257037104));
#44523=CARTESIAN_POINT('Ctrl Pts',(-0.454698034476922,-1.2581501250631,
131.296182740814));
#44524=CARTESIAN_POINT('Ctrl Pts',(0.182138945505527,-1.32533672141841,
131.323108444524));
#44525=CARTESIAN_POINT('Ctrl Pts',(0.777242075774215,-1.08884655660415,
131.350034148235));
#44526=CARTESIAN_POINT('Ctrl Pts',(1.19425434657027,-0.602867023578126,
131.376959851945));
#44527=CARTESIAN_POINT('Ctrl Pts',(1.33762498699637,0.0212485044686996,
131.403885555655));
#44528=CARTESIAN_POINT('Ctrl Pts',(1.17450323342847,0.640495329295421,131.430811259366));
#44529=CARTESIAN_POINT('Ctrl Pts',(0.742265462285602,1.11298431999035,131.457736963076));
#44530=CARTESIAN_POINT('Ctrl Pts',(0.139951084671291,1.3304532338131,131.484662666786));
#44531=CARTESIAN_POINT('Ctrl Pts',(-0.494430534395506,1.24307303066064,
131.511588370497));
#44532=CARTESIAN_POINT('Ctrl Pts',(-1.01552240527922,0.870865292057418,
131.538514074207));
#44533=CARTESIAN_POINT('Ctrl Pts',(-1.25263856527262,0.400790001029229,
131.560651535612));
#44534=CARTESIAN_POINT('Ctrl Pts',(-1.28652897849709,0.0967320105866091,
131.573813762447));
#44535=CARTESIAN_POINT('Ctrl Pts',(-1.28651317526843,5.66436777649226E-6,
131.578000754712));
#44536=CARTESIAN_POINT('Ctrl Pts',(-1.28655804524971,2.50455016348322E-5,
131.296999245288));
#44537=CARTESIAN_POINT('Ctrl Pts',(-1.28645089716158,-0.14064818329876,
131.303089175774));
#44538=CARTESIAN_POINT('Ctrl Pts',(-1.22947269431557,-0.488727931596862,
131.318154340829));
#44539=CARTESIAN_POINT('Ctrl Pts',(-0.92110007241593,-0.970189040198561,
131.342194740455));
#44540=CARTESIAN_POINT('Ctrl Pts',(-0.364663586223146,-1.28713347653886,
131.369120444165));
#44541=CARTESIAN_POINT('Ctrl Pts',(0.275328916768196,-1.30915472904038,
131.396046147875));
#44542=CARTESIAN_POINT('Ctrl Pts',(0.852234815095578,-1.03120702894802,
131.422971851586));
#44543=CARTESIAN_POINT('Ctrl Pts',(1.23386663366973,-0.516977027235267,
131.449897555296));
#44544=CARTESIAN_POINT('Ctrl Pts',(1.332780394676,0.115708840682625,131.476823259006));
#44545=CARTESIAN_POINT('Ctrl Pts',(1.1263118120373,0.721882135998308,131.503748962717));
#44546=CARTESIAN_POINT('Ctrl Pts',(0.661769399512303,1.16264929280748,131.530674666427));
#44547=CARTESIAN_POINT('Ctrl Pts',(0.0455945867891589,1.33701654808655,
131.557600370137));
#44548=CARTESIAN_POINT('Ctrl Pts',(-0.581027394744716,1.20503082232908,
131.584526073848));
#44549=CARTESIAN_POINT('Ctrl Pts',(-1.07451753531689,0.796934239763604,
131.611451777558));
#44550=CARTESIAN_POINT('Ctrl Pts',(-1.26576747112306,0.340086089182502,
131.632276168038));
#44551=CARTESIAN_POINT('Ctrl Pts',(-1.28660948093643,0.0664106792179535,
131.644125323948));
#44552=CARTESIAN_POINT('Ctrl Pts',(-1.28655866463832,2.51533884142105E-5,
131.646999245288));
#44553=CARTESIAN_POINT('Origin',(1.88724897194442,-1.29707028255787,134.));
#44554=CARTESIAN_POINT('',(1.8802655232717,-1.2357595081551,132.6));
#44555=CARTESIAN_POINT('',(1.8802655232717,-1.23575950815512,133.85));
#44556=CARTESIAN_POINT('',(1.8802655232717,-1.23575950815512,133.225));
#44557=CARTESIAN_POINT('',(1.86195461813654,-1.075,132.6));
#44558=CARTESIAN_POINT('',(1.88724897194442,-1.29707028255787,132.6));
#44559=CARTESIAN_POINT('',(1.86195461813654,-1.075,133.95));
#44560=CARTESIAN_POINT('',(1.86195461813654,-1.075,134.));
#44561=CARTESIAN_POINT('Ctrl Pts',(1.8802655232717,-1.23575950815514,133.85));
#44562=CARTESIAN_POINT('Ctrl Pts',(1.87090199223673,-1.15355294148538,133.902974875989));
#44563=CARTESIAN_POINT('Ctrl Pts',(1.86195461813654,-1.075,133.95));
#44564=CARTESIAN_POINT('Origin',(1.86195461813654,-1.075,134.));
#44565=CARTESIAN_POINT('',(2.01033188866635,-1.01047795493577,133.85));
#44566=CARTESIAN_POINT('Ctrl Pts',(1.86195461813654,-1.075,133.95));
#44567=CARTESIAN_POINT('Ctrl Pts',(1.93445714805536,-1.04347218252507,133.902974875989));
#44568=CARTESIAN_POINT('Ctrl Pts',(2.01033188866637,-1.01047795493577,133.85));
#44569=CARTESIAN_POINT('',(2.01033188866633,-1.01047795493578,132.6));
#44570=CARTESIAN_POINT('',(1.86195461813654,-1.075,132.6));
#44571=CARTESIAN_POINT('',(2.01033188866635,-1.01047795493577,133.225));
#44572=CARTESIAN_POINT('Origin',(1.96443745964886,-1.14147034712443,132.6));
#44573=CARTESIAN_POINT('Origin',(0.,0.,132.6));
#44574=CARTESIAN_POINT('Origin',(0.985870411690995,-2.06692030116118,134.));
#44575=CARTESIAN_POINT('',(1.01047795493578,-2.01033188866633,132.6));
#44576=CARTESIAN_POINT('',(1.01047795493577,-2.01033188866635,133.85));
#44577=CARTESIAN_POINT('',(1.01047795493577,-2.01033188866635,133.225));
#44578=CARTESIAN_POINT('',(1.075,-1.86195461813654,132.6));
#44579=CARTESIAN_POINT('',(0.985870411690995,-2.06692030116118,132.6));
#44580=CARTESIAN_POINT('',(1.075,-1.86195461813654,133.95));
#44581=CARTESIAN_POINT('',(1.075,-1.86195461813654,134.));
#44582=CARTESIAN_POINT('Ctrl Pts',(1.01047795493577,-2.01033188866637,133.85));
#44583=CARTESIAN_POINT('Ctrl Pts',(1.04347218252507,-1.93445714805537,133.902974875989));
#44584=CARTESIAN_POINT('Ctrl Pts',(1.075,-1.86195461813654,133.95));
#44585=CARTESIAN_POINT('Origin',(1.075,-1.86195461813654,134.));
#44586=CARTESIAN_POINT('',(1.23575950815512,-1.8802655232717,133.85));
#44587=CARTESIAN_POINT('Ctrl Pts',(1.075,-1.86195461813654,133.95));
#44588=CARTESIAN_POINT('Ctrl Pts',(1.1535529414858,-1.87090199223678,133.902974875989));
#44589=CARTESIAN_POINT('Ctrl Pts',(1.23575950815514,-1.88026552327171,133.85));
#44590=CARTESIAN_POINT('',(1.2357595081551,-1.8802655232717,132.6));
#44591=CARTESIAN_POINT('',(1.075,-1.86195461813654,132.6));
#44592=CARTESIAN_POINT('',(1.23575950815512,-1.8802655232717,133.225));
#44593=CARTESIAN_POINT('Origin',(1.14147034712443,-1.96443745964886,132.6));
#44594=CARTESIAN_POINT('Origin',(0.,0.,132.6));
#44595=CARTESIAN_POINT('Origin',(-0.179671329216764,-2.28294069424886,134.));
#44596=CARTESIAN_POINT('',(-0.13006636539463,-2.24623746309088,132.6));
#44597=CARTESIAN_POINT('',(-0.130066365394647,-2.2462374630909,133.85));
#44598=CARTESIAN_POINT('',(-0.130066365394647,-2.2462374630909,133.225));
#44599=CARTESIAN_POINT('',(-3.94948592725021E-16,-2.15,132.6));
#44600=CARTESIAN_POINT('',(-0.179671329216764,-2.28294069424886,132.6));
#44601=CARTESIAN_POINT('',(-3.94948592725021E-16,-2.15,133.95));
#44602=CARTESIAN_POINT('',(-3.94948592725021E-16,-2.15,134.));
#44603=CARTESIAN_POINT('Ctrl Pts',(-0.130066365394665,-2.24623746309091,
133.85));
#44604=CARTESIAN_POINT('Ctrl Pts',(-0.0635551558182033,-2.19702512401059,
133.902974875989));
#44605=CARTESIAN_POINT('Ctrl Pts',(-3.94948592725021E-16,-2.15,133.95));
#44606=CARTESIAN_POINT('Origin',(-3.94948592725021E-16,-2.15,134.));
#44607=CARTESIAN_POINT('',(0.130066365394648,-2.2462374630909,133.85));
#44608=CARTESIAN_POINT('Ctrl Pts',(-3.94948592725021E-16,-2.15,133.95));
#44609=CARTESIAN_POINT('Ctrl Pts',(0.0635551558186,-2.19702512401089,133.902974875989));
#44610=CARTESIAN_POINT('Ctrl Pts',(0.130066365394665,-2.24623746309091,
133.85));
#44611=CARTESIAN_POINT('',(0.13006636539463,-2.24623746309088,132.6));
#44612=CARTESIAN_POINT('',(-3.94948592725021E-16,-2.15,132.6));
#44613=CARTESIAN_POINT('',(0.130066365394648,-2.2462374630909,133.225));
#44614=CARTESIAN_POINT('Origin',(6.10622663543836E-16,-2.21647034712443,
132.6));
#44615=CARTESIAN_POINT('Origin',(0.,0.,132.6));
#44616=CARTESIAN_POINT('Origin',(-1.29707028255787,-1.88724897194442,134.));
#44617=CARTESIAN_POINT('',(-1.2357595081551,-1.8802655232717,132.6));
#44618=CARTESIAN_POINT('',(-1.23575950815512,-1.8802655232717,133.85));
#44619=CARTESIAN_POINT('',(-1.23575950815512,-1.8802655232717,133.225));
#44620=CARTESIAN_POINT('',(-1.075,-1.86195461813654,132.6));
#44621=CARTESIAN_POINT('',(-1.29707028255787,-1.88724897194442,132.6));
#44622=CARTESIAN_POINT('',(-1.075,-1.86195461813654,133.95));
#44623=CARTESIAN_POINT('',(-1.075,-1.86195461813654,134.));
#44624=CARTESIAN_POINT('Ctrl Pts',(-1.23575950815514,-1.8802655232717,133.85));
#44625=CARTESIAN_POINT('Ctrl Pts',(-1.15355294148538,-1.87090199223673,
133.902974875989));
#44626=CARTESIAN_POINT('Ctrl Pts',(-1.075,-1.86195461813654,133.95));
#44627=CARTESIAN_POINT('Origin',(-1.075,-1.86195461813654,134.));
#44628=CARTESIAN_POINT('',(-1.01047795493577,-2.01033188866635,133.85));
#44629=CARTESIAN_POINT('Ctrl Pts',(-1.075,-1.86195461813654,133.95));
#44630=CARTESIAN_POINT('Ctrl Pts',(-1.04347218252507,-1.93445714805536,
133.902974875989));
#44631=CARTESIAN_POINT('Ctrl Pts',(-1.01047795493577,-2.01033188866637,
133.85));
#44632=CARTESIAN_POINT('',(-1.01047795493578,-2.01033188866633,132.6));
#44633=CARTESIAN_POINT('',(-1.075,-1.86195461813654,132.6));
#44634=CARTESIAN_POINT('',(-1.01047795493577,-2.01033188866635,133.225));
#44635=CARTESIAN_POINT('Origin',(-1.14147034712443,-1.96443745964886,132.6));
#44636=CARTESIAN_POINT('Origin',(0.,0.,132.6));
#44637=CARTESIAN_POINT('Origin',(-2.06692030116118,-0.985870411690996,134.));
#44638=CARTESIAN_POINT('',(-2.01033188866633,-1.01047795493578,132.6));
#44639=CARTESIAN_POINT('',(-2.01033188866635,-1.01047795493577,133.85));
#44640=CARTESIAN_POINT('',(-2.01033188866635,-1.01047795493577,133.225));
#44641=CARTESIAN_POINT('',(-1.86195461813654,-1.075,132.6));
#44642=CARTESIAN_POINT('',(-2.06692030116118,-0.985870411690996,132.6));
#44643=CARTESIAN_POINT('',(-1.86195461813654,-1.075,133.95));
#44644=CARTESIAN_POINT('',(-1.86195461813654,-1.075,134.));
#44645=CARTESIAN_POINT('Ctrl Pts',(-2.01033188866637,-1.01047795493577,
133.85));
#44646=CARTESIAN_POINT('Ctrl Pts',(-1.93445714805536,-1.04347218252507,
133.902974875989));
#44647=CARTESIAN_POINT('Ctrl Pts',(-1.86195461813654,-1.075,133.95));
#44648=CARTESIAN_POINT('Origin',(-1.86195461813654,-1.075,134.));
#44649=CARTESIAN_POINT('',(-1.8802655232717,-1.23575950815512,133.85));
#44650=CARTESIAN_POINT('Ctrl Pts',(-1.86195461813654,-1.075,133.95));
#44651=CARTESIAN_POINT('Ctrl Pts',(-1.87090199223678,-1.15355294148581,
133.902974875989));
#44652=CARTESIAN_POINT('Ctrl Pts',(-1.88026552327171,-1.23575950815514,
133.85));
#44653=CARTESIAN_POINT('',(-1.8802655232717,-1.2357595081551,132.6));
#44654=CARTESIAN_POINT('',(-1.86195461813654,-1.075,132.6));
#44655=CARTESIAN_POINT('',(-1.8802655232717,-1.23575950815512,133.225));
#44656=CARTESIAN_POINT('Origin',(-1.96443745964886,-1.14147034712443,132.6));
#44657=CARTESIAN_POINT('Origin',(0.,0.,132.6));
#44658=CARTESIAN_POINT('Origin',(-2.28294069424886,0.179671329216765,134.));
#44659=CARTESIAN_POINT('',(-2.24623746309088,0.13006636539463,132.6));
#44660=CARTESIAN_POINT('',(-2.2462374630909,0.130066365394648,133.85));
#44661=CARTESIAN_POINT('',(-2.2462374630909,0.130066365394648,133.225));
#44662=CARTESIAN_POINT('',(-2.15,2.63299061816681E-16,132.6));
#44663=CARTESIAN_POINT('',(-2.28294069424886,0.179671329216765,132.6));
#44664=CARTESIAN_POINT('',(-2.15,2.63299061816681E-16,133.95));
#44665=CARTESIAN_POINT('',(-2.15,2.63299061816681E-16,134.));
#44666=CARTESIAN_POINT('Ctrl Pts',(-2.24623746309091,0.130066365394665,
133.85));
#44667=CARTESIAN_POINT('Ctrl Pts',(-2.19702512401088,0.0635551558185912,
133.902974875989));
#44668=CARTESIAN_POINT('Ctrl Pts',(-2.15,2.63299061816681E-16,133.95));
#44669=CARTESIAN_POINT('Origin',(-2.15,2.63299061816681E-16,134.));
#44670=CARTESIAN_POINT('',(-2.2462374630909,-0.130066365394647,133.85));
#44671=CARTESIAN_POINT('Ctrl Pts',(-2.15,2.63299061816681E-16,133.95));
#44672=CARTESIAN_POINT('Ctrl Pts',(-2.19702512401089,-0.0635551558186091,
133.902974875989));
#44673=CARTESIAN_POINT('Ctrl Pts',(-2.24623746309091,-0.130066365394664,
133.85));
#44674=CARTESIAN_POINT('',(-2.24623746309088,-0.13006636539463,132.6));
#44675=CARTESIAN_POINT('',(-2.15,2.63299061816681E-16,132.6));
#44676=CARTESIAN_POINT('',(-2.2462374630909,-0.130066365394647,133.225));
#44677=CARTESIAN_POINT('Origin',(-2.21647034712443,2.77555756156289E-16,
132.6));
#44678=CARTESIAN_POINT('',(-2.24999999999999,-2.75545529808154E-16,132.6));
#44679=CARTESIAN_POINT('Origin',(0.,0.,132.6));
#44680=CARTESIAN_POINT('Origin',(0.,0.,132.6));
#44681=CARTESIAN_POINT('Origin',(-2.15864901460109,0.764417707645336,134.));
#44682=CARTESIAN_POINT('',(-2.13603512508613,0.707003496736915,132.6));
#44683=CARTESIAN_POINT('',(-2.13603512508614,0.707003496736936,133.85));
#44684=CARTESIAN_POINT('',(-2.13603512508614,0.707003496736936,133.225));
#44685=CARTESIAN_POINT('',(-2.0767405265215,0.55646094697042,132.6));
#44686=CARTESIAN_POINT('',(-2.15864901460109,0.764417707645336,132.6));
#44687=CARTESIAN_POINT('',(-2.0767405265215,0.55646094697042,133.95));
#44688=CARTESIAN_POINT('',(-2.0767405265215,0.55646094697042,134.));
#44689=CARTESIAN_POINT('Ctrl Pts',(-2.13603512508614,0.707003496736955,
133.85));
#44690=CARTESIAN_POINT('Ctrl Pts',(-2.10571402354774,0.63002151106175,133.902974875989));
#44691=CARTESIAN_POINT('Ctrl Pts',(-2.0767405265215,0.55646094697042,133.95));
#44692=CARTESIAN_POINT('Origin',(-2.0767405265215,0.55646094697042,134.));
#44693=CARTESIAN_POINT('',(-2.20336243006893,0.455734573804454,133.85));
#44694=CARTESIAN_POINT('Ctrl Pts',(-2.0767405265215,0.55646094697042,133.95));
#44695=CARTESIAN_POINT('Ctrl Pts',(-2.13861259302839,0.50724237826372,133.902974875989));
#44696=CARTESIAN_POINT('Ctrl Pts',(-2.20336243006895,0.455734573804441,
133.85));
#44697=CARTESIAN_POINT('',(-2.20336243006892,0.455734573804468,132.6));
#44698=CARTESIAN_POINT('',(-2.0767405265215,0.55646094697042,132.6));
#44699=CARTESIAN_POINT('',(-2.20336243006893,0.455734573804454,133.225));
#44700=CARTESIAN_POINT('Origin',(-2.16419713242148,0.590868530511177,132.6));
#44701=CARTESIAN_POINT('Origin',(0.,0.,132.6));
#44702=CARTESIAN_POINT('Origin',(-1.48723603067612,1.74132966122407,134.));
#44703=CARTESIAN_POINT('',(-1.496358933332,1.68030055128166,132.6));
#44704=CARTESIAN_POINT('',(-1.496358933332,1.68030055128168,133.85));
#44705=CARTESIAN_POINT('',(-1.496358933332,1.68030055128168,133.225));
#44706=CARTESIAN_POINT('',(-1.52027957955108,1.52027957955108,132.6));
#44707=CARTESIAN_POINT('',(-1.48723603067612,1.74132966122407,132.6));
#44708=CARTESIAN_POINT('',(-1.52027957955108,1.52027957955108,133.95));
#44709=CARTESIAN_POINT('',(-1.52027957955108,1.52027957955108,134.));
#44710=CARTESIAN_POINT('Ctrl Pts',(-1.49635893333199,1.6803005512817,133.85));
#44711=CARTESIAN_POINT('Ctrl Pts',(-1.50859108196662,1.598471645284,133.902974875989));
#44712=CARTESIAN_POINT('Ctrl Pts',(-1.52027957955108,1.52027957955108,133.95));
#44713=CARTESIAN_POINT('Origin',(-1.52027957955108,1.52027957955108,134.));
#44714=CARTESIAN_POINT('',(-1.68030055128168,1.496358933332,133.85));
#44715=CARTESIAN_POINT('Ctrl Pts',(-1.52027957955108,1.52027957955108,133.95));
#44716=CARTESIAN_POINT('Ctrl Pts',(-1.59847164528371,1.50859108196666,133.902974875989));
#44717=CARTESIAN_POINT('Ctrl Pts',(-1.6803005512817,1.49635893333199,133.85));
#44718=CARTESIAN_POINT('',(-1.68030055128166,1.496358933332,132.6));
#44719=CARTESIAN_POINT('',(-1.52027957955108,1.52027957955108,132.6));
#44720=CARTESIAN_POINT('',(-1.68030055128168,1.496358933332,133.225));
#44721=CARTESIAN_POINT('Origin',(-1.6142828459501,1.6142828459501,132.6));
#44722=CARTESIAN_POINT('Origin',(0.,0.,132.6));
#44723=CARTESIAN_POINT('Origin',(-0.417319353377018,2.25165373832146,134.));
#44724=CARTESIAN_POINT('',(-0.455734573804468,2.20336243006892,132.6));
#44725=CARTESIAN_POINT('',(-0.455734573804454,2.20336243006893,133.85));
#44726=CARTESIAN_POINT('',(-0.455734573804454,2.20336243006893,133.225));
#44727=CARTESIAN_POINT('',(-0.55646094697042,2.0767405265215,132.6));
#44728=CARTESIAN_POINT('',(-0.417319353377018,2.25165373832146,132.6));
#44729=CARTESIAN_POINT('',(-0.55646094697042,2.0767405265215,133.95));
#44730=CARTESIAN_POINT('',(-0.55646094697042,2.0767405265215,134.));
#44731=CARTESIAN_POINT('Ctrl Pts',(-0.455734573804441,2.20336243006895,
133.85));
#44732=CARTESIAN_POINT('Ctrl Pts',(-0.507242378263725,2.13861259302838,
133.902974875989));
#44733=CARTESIAN_POINT('Ctrl Pts',(-0.55646094697042,2.0767405265215,133.95));
#44734=CARTESIAN_POINT('Origin',(-0.55646094697042,2.0767405265215,134.));
#44735=CARTESIAN_POINT('',(-0.707003496736936,2.13603512508614,133.85));
#44736=CARTESIAN_POINT('Ctrl Pts',(-0.55646094697042,2.0767405265215,133.95));
#44737=CARTESIAN_POINT('Ctrl Pts',(-0.630021511061762,2.10571402354775,
133.902974875989));
#44738=CARTESIAN_POINT('Ctrl Pts',(-0.707003496736956,2.13603512508614,
133.85));
#44739=CARTESIAN_POINT('',(-0.707003496736916,2.13603512508613,132.6));
#44740=CARTESIAN_POINT('',(-0.55646094697042,2.0767405265215,132.6));
#44741=CARTESIAN_POINT('',(-0.707003496736936,2.13603512508614,133.225));
#44742=CARTESIAN_POINT('Origin',(-0.590868530511177,2.16419713242148,132.6));
#44743=CARTESIAN_POINT('Origin',(0.,0.,132.6));
#44744=CARTESIAN_POINT('Origin',(0.764417707645335,2.15864901460109,134.));
#44745=CARTESIAN_POINT('',(0.707003496736915,2.13603512508613,132.6));
#44746=CARTESIAN_POINT('',(0.707003496736935,2.13603512508614,133.85));
#44747=CARTESIAN_POINT('',(0.707003496736935,2.13603512508614,133.225));
#44748=CARTESIAN_POINT('',(0.55646094697042,2.0767405265215,132.6));
#44749=CARTESIAN_POINT('',(0.764417707645335,2.15864901460109,132.6));
#44750=CARTESIAN_POINT('',(0.55646094697042,2.0767405265215,133.95));
#44751=CARTESIAN_POINT('',(0.55646094697042,2.0767405265215,134.));
#44752=CARTESIAN_POINT('Ctrl Pts',(0.707003496736955,2.13603512508614,133.85));
#44753=CARTESIAN_POINT('Ctrl Pts',(0.630021511061745,2.10571402354774,133.902974875989));
#44754=CARTESIAN_POINT('Ctrl Pts',(0.55646094697042,2.0767405265215,133.95));
#44755=CARTESIAN_POINT('Origin',(0.55646094697042,2.0767405265215,134.));
#44756=CARTESIAN_POINT('',(0.455734573804454,2.20336243006893,133.85));
#44757=CARTESIAN_POINT('Ctrl Pts',(0.55646094697042,2.0767405265215,133.95));
#44758=CARTESIAN_POINT('Ctrl Pts',(0.507242378263745,2.13861259302836,133.902974875989));
#44759=CARTESIAN_POINT('Ctrl Pts',(0.45573457380444,2.20336243006895,133.85));
#44760=CARTESIAN_POINT('',(0.455734573804467,2.20336243006892,132.6));
#44761=CARTESIAN_POINT('',(0.55646094697042,2.0767405265215,132.6));
#44762=CARTESIAN_POINT('',(0.455734573804454,2.20336243006893,133.225));
#44763=CARTESIAN_POINT('Origin',(0.590868530511176,2.16419713242148,132.6));
#44764=CARTESIAN_POINT('Origin',(0.,0.,132.6));
#44765=CARTESIAN_POINT('Origin',(1.74132966122407,1.48723603067612,134.));
#44766=CARTESIAN_POINT('',(1.68030055128166,1.496358933332,132.6));
#44767=CARTESIAN_POINT('',(1.68030055128168,1.496358933332,133.85));
#44768=CARTESIAN_POINT('',(1.68030055128168,1.496358933332,133.225));
#44769=CARTESIAN_POINT('',(1.52027957955108,1.52027957955108,132.6));
#44770=CARTESIAN_POINT('',(1.74132966122407,1.48723603067612,132.6));
#44771=CARTESIAN_POINT('',(1.52027957955108,1.52027957955108,133.95));
#44772=CARTESIAN_POINT('',(1.52027957955108,1.52027957955108,134.));
#44773=CARTESIAN_POINT('Ctrl Pts',(1.6803005512817,1.49635893333199,133.85));
#44774=CARTESIAN_POINT('Ctrl Pts',(1.59847164528401,1.50859108196661,133.902974875989));
#44775=CARTESIAN_POINT('Ctrl Pts',(1.52027957955108,1.52027957955108,133.95));
#44776=CARTESIAN_POINT('Origin',(1.52027957955108,1.52027957955108,134.));
#44777=CARTESIAN_POINT('',(1.496358933332,1.68030055128168,133.85));
#44778=CARTESIAN_POINT('Ctrl Pts',(1.52027957955108,1.52027957955108,133.95));
#44779=CARTESIAN_POINT('Ctrl Pts',(1.50859108196669,1.59847164528354,133.902974875989));
#44780=CARTESIAN_POINT('Ctrl Pts',(1.49635893333199,1.6803005512817,133.85));
#44781=CARTESIAN_POINT('',(1.496358933332,1.68030055128166,132.6));
#44782=CARTESIAN_POINT('',(1.52027957955108,1.52027957955108,132.6));
#44783=CARTESIAN_POINT('',(1.496358933332,1.68030055128168,133.225));
#44784=CARTESIAN_POINT('Origin',(1.6142828459501,1.6142828459501,132.6));
#44785=CARTESIAN_POINT('Origin',(0.,0.,132.6));
#44786=CARTESIAN_POINT('Origin',(2.25165373832146,0.417319353377018,134.));
#44787=CARTESIAN_POINT('',(2.20336243006892,0.455734573804467,132.6));
#44788=CARTESIAN_POINT('',(2.20336243006893,0.455734573804454,133.85));
#44789=CARTESIAN_POINT('',(2.20336243006893,0.455734573804454,133.225));
#44790=CARTESIAN_POINT('',(2.0767405265215,0.55646094697042,132.6));
#44791=CARTESIAN_POINT('',(2.25165373832146,0.417319353377018,132.6));
#44792=CARTESIAN_POINT('',(2.0767405265215,0.55646094697042,133.95));
#44793=CARTESIAN_POINT('',(2.0767405265215,0.55646094697042,134.));
#44794=CARTESIAN_POINT('Ctrl Pts',(2.20336243006895,0.45573457380444,133.85));
#44795=CARTESIAN_POINT('Ctrl Pts',(2.13861259302836,0.507242378263746,133.902974875989));
#44796=CARTESIAN_POINT('Ctrl Pts',(2.0767405265215,0.55646094697042,133.95));
#44797=CARTESIAN_POINT('Origin',(2.0767405265215,0.55646094697042,134.));
#44798=CARTESIAN_POINT('',(2.13603512508614,0.707003496736936,133.85));
#44799=CARTESIAN_POINT('Ctrl Pts',(2.0767405265215,0.55646094697042,133.95));
#44800=CARTESIAN_POINT('Ctrl Pts',(2.10571402354757,0.630021511061296,133.902974875989));
#44801=CARTESIAN_POINT('Ctrl Pts',(2.13603512508614,0.707003496736956,133.85));
#44802=CARTESIAN_POINT('',(2.13603512508613,0.707003496736915,132.6));
#44803=CARTESIAN_POINT('',(2.0767405265215,0.55646094697042,132.6));
#44804=CARTESIAN_POINT('',(2.13603512508614,0.707003496736936,133.225));
#44805=CARTESIAN_POINT('Origin',(2.16419713242148,0.590868530511176,132.6));
#44806=CARTESIAN_POINT('Origin',(0.,0.,132.6));
#44807=CARTESIAN_POINT('Origin',(2.06692030116118,0.985870411690996,134.));
#44808=CARTESIAN_POINT('',(2.01033188866633,1.01047795493578,132.6));
#44809=CARTESIAN_POINT('',(2.01033188866635,1.01047795493577,133.85));
#44810=CARTESIAN_POINT('',(2.01033188866635,1.01047795493577,133.225));
#44811=CARTESIAN_POINT('',(1.86195461813654,1.075,132.6));
#44812=CARTESIAN_POINT('',(2.06692030116118,0.985870411690996,132.6));
#44813=CARTESIAN_POINT('',(1.86195461813654,1.075,133.95));
#44814=CARTESIAN_POINT('',(1.86195461813654,1.075,134.));
#44815=CARTESIAN_POINT('Ctrl Pts',(2.01033188866637,1.01047795493577,133.85));
#44816=CARTESIAN_POINT('Ctrl Pts',(1.93445714805535,1.04347218252507,133.902974875989));
#44817=CARTESIAN_POINT('Ctrl Pts',(1.86195461813654,1.075,133.95));
#44818=CARTESIAN_POINT('Origin',(1.86195461813654,1.075,134.));
#44819=CARTESIAN_POINT('',(1.8802655232717,1.23575950815512,133.85));
#44820=CARTESIAN_POINT('Ctrl Pts',(1.86195461813654,1.075,133.95));
#44821=CARTESIAN_POINT('Ctrl Pts',(1.87090199223678,1.15355294148582,133.902974875989));
#44822=CARTESIAN_POINT('Ctrl Pts',(1.88026552327171,1.23575950815514,133.85));
#44823=CARTESIAN_POINT('',(1.8802655232717,1.2357595081551,132.6));
#44824=CARTESIAN_POINT('',(1.86195461813654,1.075,132.6));
#44825=CARTESIAN_POINT('',(1.8802655232717,1.23575950815512,133.225));
#44826=CARTESIAN_POINT('Origin',(1.96443745964886,1.14147034712443,132.6));
#44827=CARTESIAN_POINT('Origin',(0.,0.,132.6));
#44828=CARTESIAN_POINT('Origin',(1.29707028255787,1.88724897194442,134.));
#44829=CARTESIAN_POINT('',(1.2357595081551,1.8802655232717,132.6));
#44830=CARTESIAN_POINT('',(1.23575950815512,1.8802655232717,133.85));
#44831=CARTESIAN_POINT('',(1.23575950815512,1.8802655232717,133.225));
#44832=CARTESIAN_POINT('',(1.075,1.86195461813654,132.6));
#44833=CARTESIAN_POINT('',(1.29707028255787,1.88724897194442,132.6));
#44834=CARTESIAN_POINT('',(1.075,1.86195461813654,133.95));
#44835=CARTESIAN_POINT('',(1.075,1.86195461813654,134.));
#44836=CARTESIAN_POINT('Ctrl Pts',(1.23575950815514,1.88026552327171,133.85));
#44837=CARTESIAN_POINT('Ctrl Pts',(1.15355294148583,1.87090199223679,133.902974875989));
#44838=CARTESIAN_POINT('Ctrl Pts',(1.075,1.86195461813654,133.95));
#44839=CARTESIAN_POINT('Origin',(1.075,1.86195461813654,134.));
#44840=CARTESIAN_POINT('',(1.01047795493577,2.01033188866635,133.85));
#44841=CARTESIAN_POINT('Ctrl Pts',(1.075,1.86195461813654,133.95));
#44842=CARTESIAN_POINT('Ctrl Pts',(1.04347218252507,1.93445714805536,133.902974875989));
#44843=CARTESIAN_POINT('Ctrl Pts',(1.01047795493577,2.01033188866637,133.85));
#44844=CARTESIAN_POINT('',(1.01047795493578,2.01033188866633,132.6));
#44845=CARTESIAN_POINT('',(1.075,1.86195461813654,132.6));
#44846=CARTESIAN_POINT('',(1.01047795493577,2.01033188866635,133.225));
#44847=CARTESIAN_POINT('Origin',(1.14147034712443,1.96443745964886,132.6));
#44848=CARTESIAN_POINT('Origin',(0.,0.,132.6));
#44849=CARTESIAN_POINT('Origin',(0.179671329216765,2.28294069424886,134.));
#44850=CARTESIAN_POINT('',(0.13006636539463,2.24623746309088,132.6));
#44851=CARTESIAN_POINT('',(0.130066365394648,2.2462374630909,133.85));
#44852=CARTESIAN_POINT('',(0.130066365394648,2.2462374630909,133.225));
#44853=CARTESIAN_POINT('',(1.3164953090834E-16,2.15,132.6));
#44854=CARTESIAN_POINT('',(0.179671329216765,2.28294069424886,132.6));
#44855=CARTESIAN_POINT('',(1.3164953090834E-16,2.15,133.95));
#44856=CARTESIAN_POINT('',(1.3164953090834E-16,2.15,134.));
#44857=CARTESIAN_POINT('Ctrl Pts',(0.130066365394665,2.24623746309091,133.85));
#44858=CARTESIAN_POINT('Ctrl Pts',(0.0635551558186174,2.1970251240109,133.902974875989));
#44859=CARTESIAN_POINT('Ctrl Pts',(1.3164953090834E-16,2.15,133.95));
#44860=CARTESIAN_POINT('Origin',(1.3164953090834E-16,2.15,134.));
#44861=CARTESIAN_POINT('',(-0.130066365394647,2.2462374630909,133.85));
#44862=CARTESIAN_POINT('Ctrl Pts',(1.3164953090834E-16,2.15,133.95));
#44863=CARTESIAN_POINT('Ctrl Pts',(-0.0635551558186092,2.19702512401089,
133.902974875989));
#44864=CARTESIAN_POINT('Ctrl Pts',(-0.130066365394664,2.24623746309091,
133.85));
#44865=CARTESIAN_POINT('',(-0.13006636539463,2.24623746309088,132.6));
#44866=CARTESIAN_POINT('',(1.3164953090834E-16,2.15,132.6));
#44867=CARTESIAN_POINT('',(-0.130066365394647,2.2462374630909,133.225));
#44868=CARTESIAN_POINT('Origin',(1.38777878078145E-16,2.21647034712443,
132.6));
#44869=CARTESIAN_POINT('Origin',(0.,0.,132.6));
#44870=CARTESIAN_POINT('Origin',(-0.985870411690995,2.06692030116118,134.));
#44871=CARTESIAN_POINT('',(-1.01047795493578,2.01033188866633,132.6));
#44872=CARTESIAN_POINT('',(-1.01047795493577,2.01033188866635,133.85));
#44873=CARTESIAN_POINT('',(-1.01047795493577,2.01033188866635,133.225));
#44874=CARTESIAN_POINT('',(-1.075,1.86195461813654,132.6));
#44875=CARTESIAN_POINT('',(-0.985870411690995,2.06692030116118,132.6));
#44876=CARTESIAN_POINT('',(-1.075,1.86195461813654,133.95));
#44877=CARTESIAN_POINT('',(-1.075,1.86195461813654,134.));
#44878=CARTESIAN_POINT('Ctrl Pts',(-1.01047795493577,2.01033188866637,133.85));
#44879=CARTESIAN_POINT('Ctrl Pts',(-1.04347218252506,1.93445714805537,133.902974875989));
#44880=CARTESIAN_POINT('Ctrl Pts',(-1.075,1.86195461813654,133.95));
#44881=CARTESIAN_POINT('Origin',(-1.075,1.86195461813654,134.));
#44882=CARTESIAN_POINT('',(-1.23575950815512,1.8802655232717,133.85));
#44883=CARTESIAN_POINT('Ctrl Pts',(-1.075,1.86195461813654,133.95));
#44884=CARTESIAN_POINT('Ctrl Pts',(-1.15355294148585,1.87090199223679,133.902974875989));
#44885=CARTESIAN_POINT('Ctrl Pts',(-1.23575950815514,1.88026552327171,133.85));
#44886=CARTESIAN_POINT('',(-1.2357595081551,1.8802655232717,132.6));
#44887=CARTESIAN_POINT('',(-1.075,1.86195461813654,132.6));
#44888=CARTESIAN_POINT('',(-1.23575950815512,1.8802655232717,133.225));
#44889=CARTESIAN_POINT('Origin',(-1.14147034712443,1.96443745964886,132.6));
#44890=CARTESIAN_POINT('Origin',(0.,0.,132.6));
#44891=CARTESIAN_POINT('Origin',(-1.88724897194442,1.29707028255787,134.));
#44892=CARTESIAN_POINT('',(-1.8802655232717,1.2357595081551,132.6));
#44893=CARTESIAN_POINT('',(-1.8802655232717,1.23575950815512,133.85));
#44894=CARTESIAN_POINT('',(-1.8802655232717,1.23575950815512,133.225));
#44895=CARTESIAN_POINT('',(-1.86195461813654,1.075,132.6));
#44896=CARTESIAN_POINT('',(-1.88724897194442,1.29707028255787,132.6));
#44897=CARTESIAN_POINT('',(-1.86195461813654,1.075,133.95));
#44898=CARTESIAN_POINT('',(-1.86195461813654,1.075,134.));
#44899=CARTESIAN_POINT('Ctrl Pts',(-1.88026552327171,1.23575950815514,133.85));
#44900=CARTESIAN_POINT('Ctrl Pts',(-1.87090199223678,1.1535529414858,133.902974875989));
#44901=CARTESIAN_POINT('Ctrl Pts',(-1.86195461813654,1.075,133.95));
#44902=CARTESIAN_POINT('Origin',(-1.86195461813654,1.075,134.));
#44903=CARTESIAN_POINT('',(-2.01033188866635,1.01047795493577,133.85));
#44904=CARTESIAN_POINT('Ctrl Pts',(-1.86195461813654,1.075,133.95));
#44905=CARTESIAN_POINT('Ctrl Pts',(-1.93445714805534,1.04347218252508,133.902974875989));
#44906=CARTESIAN_POINT('Ctrl Pts',(-2.01033188866637,1.01047795493577,133.85));
#44907=CARTESIAN_POINT('',(-2.01033188866633,1.01047795493578,132.6));
#44908=CARTESIAN_POINT('',(-1.86195461813654,1.075,132.6));
#44909=CARTESIAN_POINT('',(-2.01033188866635,1.01047795493577,133.225));
#44910=CARTESIAN_POINT('Origin',(-1.96443745964886,1.14147034712443,132.6));
#44911=CARTESIAN_POINT('Origin',(0.,0.,132.6));
#44912=CARTESIAN_POINT('Origin',(2.28294069424886,-0.179671329216765,134.));
#44913=CARTESIAN_POINT('',(2.24623746309088,-0.13006636539463,132.6));
#44914=CARTESIAN_POINT('',(2.2462374630909,-0.130066365394648,133.85));
#44915=CARTESIAN_POINT('',(2.2462374630909,-0.130066365394648,133.225));
#44916=CARTESIAN_POINT('',(2.15,0.,132.6));
#44917=CARTESIAN_POINT('',(2.28294069424886,-0.179671329216765,132.6));
#44918=CARTESIAN_POINT('',(2.15,0.,133.95));
#44919=CARTESIAN_POINT('',(2.15,0.,134.));
#44920=CARTESIAN_POINT('Ctrl Pts',(2.24623746309091,-0.130066365394665,
133.85));
#44921=CARTESIAN_POINT('Ctrl Pts',(2.19702512401089,-0.06355515581861,133.902974875989));
#44922=CARTESIAN_POINT('Ctrl Pts',(2.15,0.,133.95));
#44923=CARTESIAN_POINT('Origin',(2.15,0.,134.));
#44924=CARTESIAN_POINT('',(2.2462374630909,0.130066365394648,133.85));
#44925=CARTESIAN_POINT('Ctrl Pts',(2.15,0.,133.95));
#44926=CARTESIAN_POINT('Ctrl Pts',(2.19702512401088,0.0635551558185882,
133.902974875989));
#44927=CARTESIAN_POINT('Ctrl Pts',(2.24623746309091,0.130066365394665,133.85));
#44928=CARTESIAN_POINT('',(2.24623746309088,0.13006636539463,132.6));
#44929=CARTESIAN_POINT('',(2.15,0.,132.6));
#44930=CARTESIAN_POINT('',(2.2462374630909,0.130066365394648,133.225));
#44931=CARTESIAN_POINT('Origin',(2.21647034712443,0.,132.6));
#44932=CARTESIAN_POINT('Origin',(0.,0.,132.6));
#44933=CARTESIAN_POINT('Origin',(-2.25165373832146,-0.417319353377018,134.));
#44934=CARTESIAN_POINT('',(-2.20336243006892,-0.455734573804467,132.6));
#44935=CARTESIAN_POINT('',(-2.20336243006893,-0.455734573804454,133.85));
#44936=CARTESIAN_POINT('',(-2.20336243006893,-0.455734573804454,133.225));
#44937=CARTESIAN_POINT('',(-2.0767405265215,-0.55646094697042,132.6));
#44938=CARTESIAN_POINT('',(-2.25165373832146,-0.417319353377018,132.6));
#44939=CARTESIAN_POINT('',(-2.0767405265215,-0.55646094697042,133.95));
#44940=CARTESIAN_POINT('',(-2.0767405265215,-0.55646094697042,134.));
#44941=CARTESIAN_POINT('Ctrl Pts',(-2.20336243006895,-0.455734573804441,
133.85));
#44942=CARTESIAN_POINT('Ctrl Pts',(-2.13861259302836,-0.50724237826374,
133.902974875989));
#44943=CARTESIAN_POINT('Ctrl Pts',(-2.0767405265215,-0.55646094697042,133.95));
#44944=CARTESIAN_POINT('Origin',(-2.0767405265215,-0.55646094697042,134.));
#44945=CARTESIAN_POINT('',(-2.13603512508614,-0.707003496736936,133.85));
#44946=CARTESIAN_POINT('Ctrl Pts',(-2.0767405265215,-0.55646094697042,133.95));
#44947=CARTESIAN_POINT('Ctrl Pts',(-2.10571402354757,-0.630021511061296,
133.902974875989));
#44948=CARTESIAN_POINT('Ctrl Pts',(-2.13603512508614,-0.707003496736956,
133.85));
#44949=CARTESIAN_POINT('',(-2.13603512508613,-0.707003496736915,132.6));
#44950=CARTESIAN_POINT('',(-2.0767405265215,-0.55646094697042,132.6));
#44951=CARTESIAN_POINT('',(-2.13603512508614,-0.707003496736936,133.225));
#44952=CARTESIAN_POINT('Origin',(-2.16419713242148,-0.590868530511177,132.6));
#44953=CARTESIAN_POINT('Origin',(0.,0.,132.6));
#44954=CARTESIAN_POINT('Origin',(-1.74132966122407,-1.48723603067612,134.));
#44955=CARTESIAN_POINT('',(-1.68030055128166,-1.496358933332,132.6));
#44956=CARTESIAN_POINT('',(-1.68030055128168,-1.496358933332,133.85));
#44957=CARTESIAN_POINT('',(-1.68030055128168,-1.496358933332,133.225));
#44958=CARTESIAN_POINT('',(-1.52027957955108,-1.52027957955108,132.6));
#44959=CARTESIAN_POINT('',(-1.74132966122407,-1.48723603067612,132.6));
#44960=CARTESIAN_POINT('',(-1.52027957955108,-1.52027957955108,133.95));
#44961=CARTESIAN_POINT('',(-1.52027957955108,-1.52027957955108,134.));
#44962=CARTESIAN_POINT('Ctrl Pts',(-1.6803005512817,-1.49635893333199,133.85));
#44963=CARTESIAN_POINT('Ctrl Pts',(-1.598471645284,-1.50859108196662,133.902974875989));
#44964=CARTESIAN_POINT('Ctrl Pts',(-1.52027957955108,-1.52027957955108,
133.95));
#44965=CARTESIAN_POINT('Origin',(-1.52027957955108,-1.52027957955108,134.));
#44966=CARTESIAN_POINT('',(-1.496358933332,-1.68030055128168,133.85));
#44967=CARTESIAN_POINT('Ctrl Pts',(-1.52027957955108,-1.52027957955108,
133.95));
#44968=CARTESIAN_POINT('Ctrl Pts',(-1.50859108196661,-1.59847164528404,
133.902974875989));
#44969=CARTESIAN_POINT('Ctrl Pts',(-1.49635893333199,-1.6803005512817,133.85));
#44970=CARTESIAN_POINT('',(-1.496358933332,-1.68030055128166,132.6));
#44971=CARTESIAN_POINT('',(-1.52027957955108,-1.52027957955108,132.6));
#44972=CARTESIAN_POINT('',(-1.496358933332,-1.68030055128168,133.225));
#44973=CARTESIAN_POINT('Origin',(-1.6142828459501,-1.6142828459501,132.6));
#44974=CARTESIAN_POINT('Origin',(0.,0.,132.6));
#44975=CARTESIAN_POINT('Origin',(-0.764417707645336,-2.15864901460109,134.));
#44976=CARTESIAN_POINT('',(-0.707003496736916,-2.13603512508613,132.6));
#44977=CARTESIAN_POINT('',(-0.707003496736936,-2.13603512508614,133.85));
#44978=CARTESIAN_POINT('',(-0.707003496736936,-2.13603512508614,133.225));
#44979=CARTESIAN_POINT('',(-0.556460946970419,-2.0767405265215,132.6));
#44980=CARTESIAN_POINT('',(-0.764417707645336,-2.15864901460109,132.6));
#44981=CARTESIAN_POINT('',(-0.556460946970419,-2.0767405265215,133.95));
#44982=CARTESIAN_POINT('',(-0.556460946970419,-2.0767405265215,134.));
#44983=CARTESIAN_POINT('Ctrl Pts',(-0.707003496736956,-2.13603512508614,
133.85));
#44984=CARTESIAN_POINT('Ctrl Pts',(-0.630021511061715,-2.10571402354773,
133.902974875989));
#44985=CARTESIAN_POINT('Ctrl Pts',(-0.556460946970419,-2.0767405265215,
133.95));
#44986=CARTESIAN_POINT('Origin',(-0.556460946970419,-2.0767405265215,134.));
#44987=CARTESIAN_POINT('',(-0.455734573804454,-2.20336243006893,133.85));
#44988=CARTESIAN_POINT('Ctrl Pts',(-0.556460946970419,-2.0767405265215,
133.95));
#44989=CARTESIAN_POINT('Ctrl Pts',(-0.507242378263734,-2.13861259302837,
133.902974875989));
#44990=CARTESIAN_POINT('Ctrl Pts',(-0.455734573804441,-2.20336243006895,
133.85));
#44991=CARTESIAN_POINT('',(-0.455734573804468,-2.20336243006892,132.6));
#44992=CARTESIAN_POINT('',(-0.556460946970419,-2.0767405265215,132.6));
#44993=CARTESIAN_POINT('',(-0.455734573804454,-2.20336243006893,133.225));
#44994=CARTESIAN_POINT('Origin',(-0.590868530511177,-2.16419713242148,132.6));
#44995=CARTESIAN_POINT('Origin',(0.,0.,132.6));
#44996=CARTESIAN_POINT('Origin',(0.417319353377018,-2.25165373832146,134.));
#44997=CARTESIAN_POINT('',(0.455734573804467,-2.20336243006892,132.6));
#44998=CARTESIAN_POINT('',(0.455734573804453,-2.20336243006893,133.85));
#44999=CARTESIAN_POINT('',(0.455734573804453,-2.20336243006893,133.225));
#45000=CARTESIAN_POINT('',(0.556460946970419,-2.0767405265215,132.6));
#45001=CARTESIAN_POINT('',(0.417319353377018,-2.25165373832146,132.6));
#45002=CARTESIAN_POINT('',(0.556460946970419,-2.0767405265215,133.95));
#45003=CARTESIAN_POINT('',(0.556460946970419,-2.0767405265215,134.));
#45004=CARTESIAN_POINT('Ctrl Pts',(0.45573457380444,-2.20336243006895,133.85));
#45005=CARTESIAN_POINT('Ctrl Pts',(0.507242378263739,-2.13861259302836,
133.902974875989));
#45006=CARTESIAN_POINT('Ctrl Pts',(0.556460946970419,-2.0767405265215,133.95));
#45007=CARTESIAN_POINT('Origin',(0.556460946970419,-2.0767405265215,134.));
#45008=CARTESIAN_POINT('',(0.707003496736935,-2.13603512508614,133.85));
#45009=CARTESIAN_POINT('Ctrl Pts',(0.556460946970419,-2.0767405265215,133.95));
#45010=CARTESIAN_POINT('Ctrl Pts',(0.630021511061762,-2.10571402354775,
133.902974875989));
#45011=CARTESIAN_POINT('Ctrl Pts',(0.707003496736956,-2.13603512508614,
133.85));
#45012=CARTESIAN_POINT('',(0.707003496736915,-2.13603512508613,132.6));
#45013=CARTESIAN_POINT('',(0.556460946970419,-2.0767405265215,132.6));
#45014=CARTESIAN_POINT('',(0.707003496736935,-2.13603512508614,133.225));
#45015=CARTESIAN_POINT('Origin',(0.590868530511176,-2.16419713242148,132.6));
#45016=CARTESIAN_POINT('Origin',(0.,0.,132.6));
#45017=CARTESIAN_POINT('Origin',(1.48723603067612,-1.74132966122407,134.));
#45018=CARTESIAN_POINT('',(1.496358933332,-1.68030055128166,132.6));
#45019=CARTESIAN_POINT('',(1.496358933332,-1.68030055128168,133.85));
#45020=CARTESIAN_POINT('',(1.496358933332,-1.68030055128168,133.225));
#45021=CARTESIAN_POINT('',(1.52027957955108,-1.52027957955108,132.6));
#45022=CARTESIAN_POINT('',(1.48723603067612,-1.74132966122407,132.6));
#45023=CARTESIAN_POINT('',(1.52027957955108,-1.52027957955108,133.95));
#45024=CARTESIAN_POINT('',(1.52027957955108,-1.52027957955108,134.));
#45025=CARTESIAN_POINT('Ctrl Pts',(1.49635893333199,-1.6803005512817,133.85));
#45026=CARTESIAN_POINT('Ctrl Pts',(1.50859108196662,-1.59847164528399,133.902974875989));
#45027=CARTESIAN_POINT('Ctrl Pts',(1.52027957955108,-1.52027957955108,133.95));
#45028=CARTESIAN_POINT('Origin',(1.52027957955108,-1.52027957955108,134.));
#45029=CARTESIAN_POINT('',(1.68030055128168,-1.496358933332,133.85));
#45030=CARTESIAN_POINT('Ctrl Pts',(1.52027957955108,-1.52027957955108,133.95));
#45031=CARTESIAN_POINT('Ctrl Pts',(1.59847164528402,-1.50859108196661,133.902974875989));
#45032=CARTESIAN_POINT('Ctrl Pts',(1.6803005512817,-1.49635893333199,133.85));
#45033=CARTESIAN_POINT('',(1.68030055128166,-1.496358933332,132.6));
#45034=CARTESIAN_POINT('',(1.52027957955108,-1.52027957955108,132.6));
#45035=CARTESIAN_POINT('',(1.68030055128168,-1.496358933332,133.225));
#45036=CARTESIAN_POINT('Origin',(1.6142828459501,-1.6142828459501,132.6));
#45037=CARTESIAN_POINT('Origin',(0.,0.,132.6));
#45038=CARTESIAN_POINT('Origin',(2.15864901460109,-0.764417707645336,134.));
#45039=CARTESIAN_POINT('',(2.13603512508613,-0.707003496736916,132.6));
#45040=CARTESIAN_POINT('',(2.13603512508614,-0.707003496736936,133.85));
#45041=CARTESIAN_POINT('',(2.13603512508614,-0.707003496736936,133.225));
#45042=CARTESIAN_POINT('',(2.0767405265215,-0.556460946970419,132.6));
#45043=CARTESIAN_POINT('',(2.15864901460109,-0.764417707645336,132.6));
#45044=CARTESIAN_POINT('',(2.0767405265215,-0.556460946970419,133.95));
#45045=CARTESIAN_POINT('',(2.0767405265215,-0.556460946970419,134.));
#45046=CARTESIAN_POINT('Ctrl Pts',(2.13603512508614,-0.707003496736956,
133.85));
#45047=CARTESIAN_POINT('Ctrl Pts',(2.10571402354774,-0.630021511061738,
133.902974875989));
#45048=CARTESIAN_POINT('Ctrl Pts',(2.0767405265215,-0.556460946970419,133.95));
#45049=CARTESIAN_POINT('Origin',(2.0767405265215,-0.556460946970419,134.));
#45050=CARTESIAN_POINT('',(2.20336243006893,-0.455734573804454,133.85));
#45051=CARTESIAN_POINT('Ctrl Pts',(2.0767405265215,-0.556460946970419,133.95));
#45052=CARTESIAN_POINT('Ctrl Pts',(2.13861259302834,-0.507242378263754,
133.902974875989));
#45053=CARTESIAN_POINT('Ctrl Pts',(2.20336243006895,-0.455734573804441,
133.85));
#45054=CARTESIAN_POINT('',(2.20336243006892,-0.455734573804468,132.6));
#45055=CARTESIAN_POINT('',(2.0767405265215,-0.556460946970419,132.6));
#45056=CARTESIAN_POINT('',(2.20336243006893,-0.455734573804454,133.225));
#45057=CARTESIAN_POINT('Origin',(2.16419713242148,-0.590868530511177,132.6));
#45058=CARTESIAN_POINT('Origin',(0.,0.,132.6));
#45059=CARTESIAN_POINT('Origin',(0.,0.,133.925));
#45060=CARTESIAN_POINT('',(-2.10000000000001,-2.57175827820945E-16,134.));
#45061=CARTESIAN_POINT('Origin',(0.,0.,134.));
#45062=CARTESIAN_POINT('',(-2.175,-2.66360678814549E-16,133.925));
#45063=CARTESIAN_POINT('Origin',(0.,0.,133.85));
#45064=CARTESIAN_POINT('Origin',(0.,0.,133.85));
#45065=CARTESIAN_POINT('Origin',(0.,0.,133.85));
#45066=CARTESIAN_POINT('Origin',(0.,0.,133.85));
#45067=CARTESIAN_POINT('Origin',(0.,0.,133.85));
#45068=CARTESIAN_POINT('Origin',(0.,0.,133.85));
#45069=CARTESIAN_POINT('Origin',(0.,0.,133.85));
#45070=CARTESIAN_POINT('Origin',(0.,0.,133.85));
#45071=CARTESIAN_POINT('Origin',(0.,0.,133.85));
#45072=CARTESIAN_POINT('Origin',(0.,0.,133.85));
#45073=CARTESIAN_POINT('Origin',(0.,0.,133.85));
#45074=CARTESIAN_POINT('Origin',(0.,0.,133.85));
#45075=CARTESIAN_POINT('Origin',(0.,0.,133.85));
#45076=CARTESIAN_POINT('Origin',(0.,0.,133.85));
#45077=CARTESIAN_POINT('Origin',(0.,0.,133.85));
#45078=CARTESIAN_POINT('Origin',(0.,0.,133.85));
#45079=CARTESIAN_POINT('Origin',(0.,0.,133.85));
#45080=CARTESIAN_POINT('Origin',(0.,0.,133.85));
#45081=CARTESIAN_POINT('Origin',(0.,0.,133.85));
#45082=CARTESIAN_POINT('Origin',(0.,0.,133.85));
#45083=CARTESIAN_POINT('Origin',(0.,0.,133.85));
#45084=CARTESIAN_POINT('Origin',(0.,0.,133.85));
#45085=CARTESIAN_POINT('Origin',(0.,0.,133.85));
#45086=CARTESIAN_POINT('Origin',(0.,0.,133.85));
#45087=CARTESIAN_POINT('Origin',(0.,0.,133.225));
#45088=CARTESIAN_POINT('Origin',(0.,0.,132.6));
#45089=CARTESIAN_POINT('Origin',(0.,0.,133.225));
#45090=CARTESIAN_POINT('Origin',(0.,0.,132.6));
#45091=CARTESIAN_POINT('Origin',(0.,0.,133.225));
#45092=CARTESIAN_POINT('Origin',(0.,0.,132.6));
#45093=CARTESIAN_POINT('Origin',(0.,0.,133.225));
#45094=CARTESIAN_POINT('Origin',(0.,0.,132.6));
#45095=CARTESIAN_POINT('Origin',(0.,0.,133.225));
#45096=CARTESIAN_POINT('Origin',(0.,0.,132.6));
#45097=CARTESIAN_POINT('Origin',(0.,0.,133.225));
#45098=CARTESIAN_POINT('Origin',(0.,0.,132.6));
#45099=CARTESIAN_POINT('Origin',(0.,0.,133.225));
#45100=CARTESIAN_POINT('Origin',(0.,0.,132.6));
#45101=CARTESIAN_POINT('Origin',(0.,0.,133.225));
#45102=CARTESIAN_POINT('Origin',(0.,0.,132.6));
#45103=CARTESIAN_POINT('Origin',(0.,0.,133.225));
#45104=CARTESIAN_POINT('Origin',(0.,0.,132.6));
#45105=CARTESIAN_POINT('Origin',(0.,0.,133.225));
#45106=CARTESIAN_POINT('Origin',(0.,0.,132.6));
#45107=CARTESIAN_POINT('Origin',(0.,0.,133.225));
#45108=CARTESIAN_POINT('Origin',(0.,0.,132.6));
#45109=CARTESIAN_POINT('Origin',(0.,0.,133.225));
#45110=CARTESIAN_POINT('Origin',(0.,0.,132.6));
#45111=CARTESIAN_POINT('Origin',(0.,0.,133.225));
#45112=CARTESIAN_POINT('Origin',(0.,0.,132.6));
#45113=CARTESIAN_POINT('Origin',(0.,0.,133.225));
#45114=CARTESIAN_POINT('Origin',(0.,0.,132.6));
#45115=CARTESIAN_POINT('Origin',(0.,0.,133.225));
#45116=CARTESIAN_POINT('Origin',(0.,0.,132.6));
#45117=CARTESIAN_POINT('Origin',(0.,0.,133.225));
#45118=CARTESIAN_POINT('Origin',(0.,0.,132.6));
#45119=CARTESIAN_POINT('Origin',(0.,0.,133.225));
#45120=CARTESIAN_POINT('Origin',(0.,0.,132.6));
#45121=CARTESIAN_POINT('Origin',(0.,0.,133.225));
#45122=CARTESIAN_POINT('Origin',(0.,0.,132.6));
#45123=CARTESIAN_POINT('Origin',(0.,0.,133.225));
#45124=CARTESIAN_POINT('Origin',(0.,0.,132.6));
#45125=CARTESIAN_POINT('Origin',(0.,0.,133.225));
#45126=CARTESIAN_POINT('Origin',(0.,0.,132.6));
#45127=CARTESIAN_POINT('Origin',(0.,0.,133.225));
#45128=CARTESIAN_POINT('Origin',(0.,0.,132.6));
#45129=CARTESIAN_POINT('Origin',(0.,0.,133.225));
#45130=CARTESIAN_POINT('Origin',(0.,0.,132.6));
#45131=CARTESIAN_POINT('Origin',(0.,0.,133.225));
#45132=CARTESIAN_POINT('Origin',(0.,0.,132.6));
#45133=CARTESIAN_POINT('Ctrl Pts',(-0.557371730700663,1.15960179105404,
130.884457777378));
#45134=CARTESIAN_POINT('Ctrl Pts',(-0.744210289770409,1.06979636661117,
130.893433011949));
#45135=CARTESIAN_POINT('Ctrl Pts',(-1.07348944454164,0.798225397208331,
130.911383481089));
#45136=CARTESIAN_POINT('Ctrl Pts',(-1.32154880708789,0.207818302348253,
130.938309184799));
#45137=CARTESIAN_POINT('Ctrl Pts',(-1.2667357611315,-0.430175148668094,
130.96523488851));
#45138=CARTESIAN_POINT('Ctrl Pts',(-0.921694221117689,-0.969633149057105,
130.99216059222));
#45139=CARTESIAN_POINT('Ctrl Pts',(-0.365449910586059,-1.28691209396646,
131.01908629593));
#45140=CARTESIAN_POINT('Ctrl Pts',(0.274526574308514,-1.30932546829921,
131.046011999641));
#45141=CARTESIAN_POINT('Ctrl Pts',(0.851603122293372,-1.03172996338952,
131.072937703351));
#45142=CARTESIAN_POINT('Ctrl Pts',(1.23354957705434,-0.517733871181562,
131.099863407061));
#45143=CARTESIAN_POINT('Ctrl Pts',(1.3328512265448,0.114891597751729,131.126789110772));
#45144=CARTESIAN_POINT('Ctrl Pts',(1.12675416518279,0.721191403089574,131.153714814482));
#45145=CARTESIAN_POINT('Ctrl Pts',(0.662482047549443,1.16224333958056,131.180640518192));
#45146=CARTESIAN_POINT('Ctrl Pts',(0.0464142156206867,1.33698831153762,
131.207566221903));
#45147=CARTESIAN_POINT('Ctrl Pts',(-0.580288559487598,1.20538676777764,
131.234491925613));
#45148=CARTESIAN_POINT('Ctrl Pts',(-1.07402878803166,0.797592790182427,
131.261417629323));
#45149=CARTESIAN_POINT('Ctrl Pts',(-1.32167488266001,0.207044955006741,
131.288343333034));
#45150=CARTESIAN_POINT('Ctrl Pts',(-1.26648325984221,-0.430943463576776,
131.315269036744));
#45151=CARTESIAN_POINT('Ctrl Pts',(-0.92110007241593,-0.970189040198561,
131.342194740455));
#45152=CARTESIAN_POINT('Ctrl Pts',(-0.364663586223146,-1.28713347653886,
131.369120444165));
#45153=CARTESIAN_POINT('Ctrl Pts',(0.275328916768196,-1.30915472904038,
131.396046147875));
#45154=CARTESIAN_POINT('Ctrl Pts',(0.852234815095578,-1.03120702894802,
131.422971851586));
#45155=CARTESIAN_POINT('Ctrl Pts',(1.23386663366973,-0.516977027235267,
131.449897555296));
#45156=CARTESIAN_POINT('Ctrl Pts',(1.332780394676,0.115708840682625,131.476823259006));
#45157=CARTESIAN_POINT('Ctrl Pts',(1.1263118120373,0.721882135998308,131.503748962717));
#45158=CARTESIAN_POINT('Ctrl Pts',(0.661769399512303,1.16264929280748,131.530674666427));
#45159=CARTESIAN_POINT('Ctrl Pts',(0.0455945867891589,1.33701654808655,
131.557600370137));
#45160=CARTESIAN_POINT('Ctrl Pts',(-0.581027394744716,1.20503082232908,
131.584526073848));
#45161=CARTESIAN_POINT('Ctrl Pts',(-1.07451753531689,0.796934239763604,
131.611451777558));
#45162=CARTESIAN_POINT('Ctrl Pts',(-1.32180156079828,0.206234696607059,
131.638377481268));
#45163=CARTESIAN_POINT('Ctrl Pts',(-1.26621884236099,-0.431719769601012,
131.665303184979));
#45164=CARTESIAN_POINT('Ctrl Pts',(-0.920505147196365,-0.970753516707333,
131.692228888689));
#45165=CARTESIAN_POINT('Ctrl Pts',(-0.363874469513489,-1.2873567829668,
131.7191545924));
#45166=CARTESIAN_POINT('Ctrl Pts',(0.276131412923829,-1.30898569855063,
131.74608029611));
#45167=CARTESIAN_POINT('Ctrl Pts',(0.852866813310974,-1.03068439153984,
131.77300599982));
#45168=CARTESIAN_POINT('Ctrl Pts',(1.23418332299191,-0.516220535677922,
131.799931703531));
#45169=CARTESIAN_POINT('Ctrl Pts',(1.33270921150778,0.116525850196642,131.826857407241));
#45170=CARTESIAN_POINT('Ctrl Pts',(1.12586906668276,0.722572460645641,131.853783110951));
#45171=CARTESIAN_POINT('Ctrl Pts',(0.661056538993872,1.16305475729291,131.880708814662));
#45172=CARTESIAN_POINT('Ctrl Pts',(0.0447749500858785,1.33704424761847,
131.907634518372));
#45173=CARTESIAN_POINT('Ctrl Pts',(-0.581766002838075,1.20467441008527,
131.934560222082));
#45174=CARTESIAN_POINT('Ctrl Pts',(-1.07500587627816,0.796275381121529,
131.961485925793));
#45175=CARTESIAN_POINT('Ctrl Pts',(-1.32192774026812,0.205424357093238,
131.988411629503));
#45176=CARTESIAN_POINT('Ctrl Pts',(-1.26595394887095,-0.432495915451445,
132.015337333214));
#45177=CARTESIAN_POINT('Ctrl Pts',(-0.919909876517952,-0.971317628899406,
132.042263036924));
#45178=CARTESIAN_POINT('Ctrl Pts',(-0.363085218132085,-1.28757960555225,
132.069188740634));
#45179=CARTESIAN_POINT('Ctrl Pts',(0.276933801600455,-1.30881617440312,
132.096114444345));
#45180=CARTESIAN_POINT('Ctrl Pts',(0.853498482162152,-1.0301613647476,132.123040148055));
#45181=CARTESIAN_POINT('Ctrl Pts',(1.23449953411498,-0.51546384206413,132.149965851765));
#45182=CARTESIAN_POINT('Ctrl Pts',(1.33263749249817,0.117342823334407,132.176891555476));
#45183=CARTESIAN_POINT('Ctrl Pts',(1.125425844559,0.72326254715928,132.203817259186));
#45184=CARTESIAN_POINT('Ctrl Pts',(0.660343291616316,1.16345980844394,132.230742962896));
#45185=CARTESIAN_POINT('Ctrl Pts',(0.0439550989490249,1.33707158395214,
132.257668666607));
#45186=CARTESIAN_POINT('Ctrl Pts',(-0.582504943319958,1.20431761235457,
132.284594370317));
#45187=CARTESIAN_POINT('Ctrl Pts',(-1.07549453007113,0.795616811689296,
132.311520074027));
#45188=CARTESIAN_POINT('Ctrl Pts',(-1.32205563425755,0.204614080322882,
132.338445777738));
#45189=CARTESIAN_POINT('Ctrl Pts',(-1.2656911247959,-0.43326937505133,132.365371481448));
#45190=CARTESIAN_POINT('Ctrl Pts',(-0.919323220327711,-0.971881421552252,
132.392297185159));
#45191=CARTESIAN_POINT('Ctrl Pts',(-0.362304579342239,-1.28779095308542,
132.419222888869));
#45192=CARTESIAN_POINT('Ctrl Pts',(0.277699363289323,-1.30864921194912,
132.446148592579));
#45193=CARTESIAN_POINT('Ctrl Pts',(0.85410155756253,-1.02958919072608,132.47307429629));
#45194=CARTESIAN_POINT('Ctrl Pts',(1.10780466901396,-0.686354162750902,
132.49102476543));
#45195=CARTESIAN_POINT('Ctrl Pts',(1.18756226708949,-0.495010526943894,
132.5));
#45196=CARTESIAN_POINT('Ctrl Pts',(-0.586270641941264,1.21972545249627,
130.922971851586));
#45197=CARTESIAN_POINT('Ctrl Pts',(-0.78279650777142,1.12526374778845,130.931947086156));
#45198=CARTESIAN_POINT('Ctrl Pts',(-1.1291483064228,0.839612219742223,130.949897555296));
#45199=CARTESIAN_POINT('Ctrl Pts',(-1.39006918509154,0.21859337819608,130.976823259006));
#45200=CARTESIAN_POINT('Ctrl Pts',(-1.33241416265397,-0.452479102662395,
131.003748962717));
#45201=CARTESIAN_POINT('Ctrl Pts',(-0.969482722076592,-1.01990721350476,
131.030674666427));
#45202=CARTESIAN_POINT('Ctrl Pts',(-0.384397955395643,-1.35363660891672,
131.057600370137));
#45203=CARTESIAN_POINT('Ctrl Pts',(0.288760376755141,-1.37721208401592,
131.084526073848));
#45204=CARTESIAN_POINT('Ctrl Pts',(0.89575750201485,-1.08522365708435,131.111451777558));
#45205=CARTESIAN_POINT('Ctrl Pts',(1.29750732333861,-0.544577617222861,
131.138377481268));
#45206=CARTESIAN_POINT('Ctrl Pts',(1.40195761851129,0.120848559511423,131.165303184979));
#45207=CARTESIAN_POINT('Ctrl Pts',(1.18517472513595,0.758584125392103,131.192228888689));
#45208=CARTESIAN_POINT('Ctrl Pts',(0.696830775402138,1.22250396146085,131.2191545924));
#45209=CARTESIAN_POINT('Ctrl Pts',(0.0488207249996935,1.40630920532654,
131.24608029611));
#45210=CARTESIAN_POINT('Ctrl Pts',(-0.610375674873748,1.26788431347988,
131.27300599982));
#45211=CARTESIAN_POINT('Ctrl Pts',(-1.12971561408608,0.838946812964761,
131.299931703531));
#45212=CARTESIAN_POINT('Ctrl Pts',(-1.39020179749817,0.217779933922935,
131.326857407241));
#45213=CARTESIAN_POINT('Ctrl Pts',(-1.33214856954114,-0.453287253578409,
131.353783110951));
#45214=CARTESIAN_POINT('Ctrl Pts',(-0.968857767631288,-1.02049192679106,
131.380708814662));
#45215=CARTESIAN_POINT('Ctrl Pts',(-0.383570861261465,-1.35386946985259,
131.407634518372));
#45216=CARTESIAN_POINT('Ctrl Pts',(0.28960431950104,-1.37703249217557,131.434560222082));
#45217=CARTESIAN_POINT('Ctrl Pts',(0.896421947167448,-1.08467360925483,
131.461485925793));
#45218=CARTESIAN_POINT('Ctrl Pts',(1.29784081887703,-0.543781532021902,
131.488411629503));
#45219=CARTESIAN_POINT('Ctrl Pts',(1.40188311411341,0.121708175296234,131.515337333214));
#45220=CARTESIAN_POINT('Ctrl Pts',(1.1847094366251,0.759310671794635,131.542263036924));
#45221=CARTESIAN_POINT('Ctrl Pts',(0.696081177603758,1.22293096277045,131.569188740634));
#45222=CARTESIAN_POINT('Ctrl Pts',(0.047958599608781,1.40633890589934,131.596114444345));
#45223=CARTESIAN_POINT('Ctrl Pts',(-0.611152817661263,1.26750991277901,
131.623040148055));
#45224=CARTESIAN_POINT('Ctrl Pts',(-1.13022970220514,0.838254117667301,
131.649965851765));
#45225=CARTESIAN_POINT('Ctrl Pts',(-1.39033504371314,0.216927664807091,
131.676891555476));
#45226=CARTESIAN_POINT('Ctrl Pts',(-1.3318704423992,-0.454103809937662,
131.703817259186));
#45227=CARTESIAN_POINT('Ctrl Pts',(-0.968231996406861,-1.02108567058346,
131.730742962896));
#45228=CARTESIAN_POINT('Ctrl Pts',(-0.382740830001438,-1.3541043543931,
131.757668666607));
#45229=CARTESIAN_POINT('Ctrl Pts',(0.290448423911803,-1.37685469770148,
131.784594370317));
#45230=CARTESIAN_POINT('Ctrl Pts',(0.897086713568465,-1.08412387385937,
131.811520074027));
#45231=CARTESIAN_POINT('Ctrl Pts',(1.29817392807863,-0.542985817480746,
131.838445777738));
#45232=CARTESIAN_POINT('Ctrl Pts',(1.40180824020176,0.122567545561843,131.865371481448));
#45233=CARTESIAN_POINT('Ctrl Pts',(1.18424373556972,0.760036788768008,131.892297185159));
#45234=CARTESIAN_POINT('Ctrl Pts',(0.695331356307243,1.22335744999804,131.919222888869));
#45235=CARTESIAN_POINT('Ctrl Pts',(0.0470964659379791,1.40636804161159,
131.946148592579));
#45236=CARTESIAN_POINT('Ctrl Pts',(-0.611929721506911,1.26713502108022,
131.97307429629));
#45237=CARTESIAN_POINT('Ctrl Pts',(-1.13074336293295,0.837561098165661,
132.));
#45238=CARTESIAN_POINT('Ctrl Pts',(-1.39046776540444,0.216075310371461,
132.02692570371));
#45239=CARTESIAN_POINT('Ctrl Pts',(-1.33159181456808,-0.454920197818335,
132.053851407421));
#45240=CARTESIAN_POINT('Ctrl Pts',(-0.967605861812048,-1.02167903116986,
132.080777111131));
#45241=CARTESIAN_POINT('Ctrl Pts',(-0.38191065708713,-1.35433873000459,
132.107702814841));
#45242=CARTESIAN_POINT('Ctrl Pts',(0.291292415270928,-1.37667638397419,
132.134628518552));
#45243=CARTESIAN_POINT('Ctrl Pts',(0.897751133528208,-1.08357372889085,
132.161554222262));
#45244=CARTESIAN_POINT('Ctrl Pts',(1.29850653428721,-0.542189890406811,
132.188479925973));
#45245=CARTESIAN_POINT('Ctrl Pts',(1.40173280266611,0.123426877565145,132.215405629683));
#45246=CARTESIAN_POINT('Ctrl Pts',(1.18377753302534,0.760762655260802,132.242331333393));
#45247=CARTESIAN_POINT('Ctrl Pts',(0.69458112809352,1.22378350246043,132.269257037104));
#45248=CARTESIAN_POINT('Ctrl Pts',(0.046234106715534,1.40639679529429,132.296182740814));
#45249=CARTESIAN_POINT('Ctrl Pts',(-0.612706974974943,1.26675972390762,
132.323108444524));
#45250=CARTESIAN_POINT('Ctrl Pts',(-1.13125735271232,0.836868382868973,
132.350034148235));
#45251=CARTESIAN_POINT('Ctrl Pts',(-1.39060229051067,0.215223021932451,
132.376959851945));
#45252=CARTESIAN_POINT('Ctrl Pts',(-1.33131536344811,-0.455733760170286,
132.403885555655));
#45253=CARTESIAN_POINT('Ctrl Pts',(-0.966988788354056,-1.02227205564939,
132.430811259366));
#45254=CARTESIAN_POINT('Ctrl Pts',(-0.381089543314689,-1.35456103559908,
132.457736963076));
#45255=CARTESIAN_POINT('Ctrl Pts',(0.292097670216696,-1.37650076476049,
132.484662666786));
#45256=CARTESIAN_POINT('Ctrl Pts',(0.898385477508435,-1.0829718884809,132.511588370497));
#45257=CARTESIAN_POINT('Ctrl Pts',(1.16524272523097,-0.721940624956333,
132.529538839637));
#45258=CARTESIAN_POINT('Ctrl Pts',(1.24913563843031,-0.520676100731304,
132.538514074207));
#45259=CARTESIAN_POINT('Ctrl Pts',(-0.615169553181865,1.27984911393849,
130.961485925793));
#45260=CARTESIAN_POINT('Ctrl Pts',(-0.821382725772432,1.18073112896573,
130.970461160363));
#45261=CARTESIAN_POINT('Ctrl Pts',(-1.18480716830396,0.880999042276115,
130.988411629503));
#45262=CARTESIAN_POINT('Ctrl Pts',(-1.45858956309518,0.229368454043907,
131.015337333214));
#45263=CARTESIAN_POINT('Ctrl Pts',(-1.39809256417645,-0.474783056656697,
131.042263036924));
#45264=CARTESIAN_POINT('Ctrl Pts',(-1.0172712230355,-1.07018127795241,131.069188740634));
#45265=CARTESIAN_POINT('Ctrl Pts',(-0.403346000205227,-1.42036112386699,
131.096114444345));
#45266=CARTESIAN_POINT('Ctrl Pts',(0.30299417920177,-1.44509869973264,131.123040148055));
#45267=CARTESIAN_POINT('Ctrl Pts',(0.939911881736328,-1.13871735077919,
131.149965851765));
#45268=CARTESIAN_POINT('Ctrl Pts',(1.36146506962287,-0.571421363264162,
131.176891555476));
#45269=CARTESIAN_POINT('Ctrl Pts',(1.47106401047779,0.126805521271117,131.203817259186));
#45270=CARTESIAN_POINT('Ctrl Pts',(1.24359528508911,0.795976847694632,131.230742962896));
#45271=CARTESIAN_POINT('Ctrl Pts',(0.731179503254833,1.28276458334115,131.257668666607));
#45272=CARTESIAN_POINT('Ctrl Pts',(0.0512272343786986,1.47563009911546,
131.284594370317));
#45273=CARTESIAN_POINT('Ctrl Pts',(-0.640462790259896,1.33038185918212,
131.311520074028));
#45274=CARTESIAN_POINT('Ctrl Pts',(-1.18540244014049,0.880300835747097,
131.338445777738));
#45275=CARTESIAN_POINT('Ctrl Pts',(-1.45872871233634,0.228514912839127,
131.365371481448));
#45276=CARTESIAN_POINT('Ctrl Pts',(-1.39781387924007,-0.475631043580043,
131.392297185159));
#45277=CARTESIAN_POINT('Ctrl Pts',(-1.01661546284665,-1.07079481338356,
131.419222888869));
#45278=CARTESIAN_POINT('Ctrl Pts',(-0.402478136299785,-1.42060546316632,
131.446148592579));
#45279=CARTESIAN_POINT('Ctrl Pts',(0.303879722233887,-1.44491025531076,
131.47307429629));
#45280=CARTESIAN_POINT('Ctrl Pts',(0.940609079239318,-1.13814018956164,
131.5));
#45281=CARTESIAN_POINT('Ctrl Pts',(1.36181500408434,-0.570586036808538,
131.52692570371));
#45282=CARTESIAN_POINT('Ctrl Pts',(1.47098583355083,0.127707509909844,131.553851407421));
#45283=CARTESIAN_POINT('Ctrl Pts',(1.24310706121289,0.796739207590962,131.580777111131));
#45284=CARTESIAN_POINT('Ctrl Pts',(0.730392955695213,1.28321263273343,131.607702814841));
#45285=CARTESIAN_POINT('Ctrl Pts',(0.0503226124284044,1.47566126371214,
131.634628518552));
#45286=CARTESIAN_POINT('Ctrl Pts',(-0.64127824057781,1.32998900322893,131.661554222262));
#45287=CARTESIAN_POINT('Ctrl Pts',(-1.1859418690934,0.879573995570998,131.688479925972));
#45288=CARTESIAN_POINT('Ctrl Pts',(-1.45886852662799,0.227620633007125,
131.715405629683));
#45289=CARTESIAN_POINT('Ctrl Pts',(-1.39752204243741,-0.476487850274313,
131.742331333393));
#45290=CARTESIAN_POINT('Ctrl Pts',(-1.01595884561736,-1.07141782445958,
131.769257037104));
#45291=CARTESIAN_POINT('Ctrl Pts',(-0.401607190489387,-1.4208519258194,
131.796182740814));
#45292=CARTESIAN_POINT('Ctrl Pts',(0.304765434899777,-1.44472369685233,
131.823108444524));
#45293=CARTESIAN_POINT('Ctrl Pts',(0.941306613825954,-1.13756335617889,
131.850034148235));
#45294=CARTESIAN_POINT('Ctrl Pts',(1.36216453316536,-0.569751099283571,
131.876959851945));
#45295=CARTESIAN_POINT('Ctrl Pts',(1.47090726889573,0.128609240927045,131.903885555655));
#45296=CARTESIAN_POINT('Ctrl Pts',(1.24261840445668,0.797501116890374,131.930811259366));
#45297=CARTESIAN_POINT('Ctrl Pts',(0.729606173620613,1.28366014270317,131.957736963076));
#45298=CARTESIAN_POINT('Ctrl Pts',(0.0494179817900777,1.47569183560471,
131.984662666786));
#45299=CARTESIAN_POINT('Ctrl Pts',(-0.642093440175745,1.32959563207517,
132.011588370497));
#45300=CARTESIAN_POINT('Ctrl Pts',(-1.18648084958774,0.878846815209795,
132.038514074207));
#45301=CARTESIAN_POINT('Ctrl Pts',(-1.45900779054075,0.226726263649683,
132.065439777918));
#45302=CARTESIAN_POINT('Ctrl Pts',(-1.39722968026521,-0.477344480185226,
132.092365481628));
#45303=CARTESIAN_POINT('Ctrl Pts',(-1.01530184710615,-1.07204043344031,
132.119291185338));
#45304=CARTESIAN_POINT('Ctrl Pts',(-0.400736096042175,-1.42109785445693,
132.146216889049));
#45305=CARTESIAN_POINT('Ctrl Pts',(0.305651028941402,-1.44453659354527,
132.173142592759));
#45306=CARTESIAN_POINT('Ctrl Pts',(0.942003784894263,-1.1369860930341,132.200068296469));
#45307=CARTESIAN_POINT('Ctrl Pts',(1.36251353445943,-0.568915938749493,
132.22699400018));
#45308=CARTESIAN_POINT('Ctrl Pts',(1.47082811283404,0.129510931795882,132.25391970389));
#45309=CARTESIAN_POINT('Ctrl Pts',(1.24212922149168,0.798262763362323,132.2808454076));
#45310=CARTESIAN_POINT('Ctrl Pts',(0.728818964570724,1.28410719647692,132.307771111311));
#45311=CARTESIAN_POINT('Ctrl Pts',(0.0485131144820429,1.47572200663644,
132.334696815021));
#45312=CARTESIAN_POINT('Ctrl Pts',(-0.642909006629927,1.32920183546066,
132.361622518731));
#45313=CARTESIAN_POINT('Ctrl Pts',(-1.18702017535352,0.87811995404865,132.388548222442));
#45314=CARTESIAN_POINT('Ctrl Pts',(-1.45914894676379,0.22583196354202,132.415473926152));
#45315=CARTESIAN_POINT('Ctrl Pts',(-1.39693960210031,-0.478198145289243,
132.442399629863));
#45316=CARTESIAN_POINT('Ctrl Pts',(-1.0146543563804,-1.07266268974653,132.469325333573));
#45317=CARTESIAN_POINT('Ctrl Pts',(-0.39987450728714,-1.42133111811274,
132.496251037283));
#45318=CARTESIAN_POINT('Ctrl Pts',(0.306495977144071,-1.44435231757185,
132.523176740994));
#45319=CARTESIAN_POINT('Ctrl Pts',(0.942669397454339,-1.13635458623572,
132.550102444704));
#45320=CARTESIAN_POINT('Ctrl Pts',(1.22268078144798,-0.757527087161765,
132.568052913844));
#45321=CARTESIAN_POINT('Ctrl Pts',(1.31070900977112,-0.546341674518714,
132.577028148414));
#45322=CARTESIAN_POINT('Ctrl Pts',(-0.644068464422466,1.33997277538071,
131.));
#45323=CARTESIAN_POINT('Ctrl Pts',(-0.859968943773443,1.23619851014301,
131.00897523457));
#45324=CARTESIAN_POINT('Ctrl Pts',(-1.24046603018512,0.922385864810007,
131.02692570371));
#45325=CARTESIAN_POINT('Ctrl Pts',(-1.52710994109882,0.240143529891734,
131.053851407421));
#45326=CARTESIAN_POINT('Ctrl Pts',(-1.46377096569892,-0.497087010650998,
131.080777111131));
#45327=CARTESIAN_POINT('Ctrl Pts',(-1.0650597239944,-1.12045534240007,131.107702814842));
#45328=CARTESIAN_POINT('Ctrl Pts',(-0.422294045014812,-1.48708563881725,
131.134628518552));
#45329=CARTESIAN_POINT('Ctrl Pts',(0.317227981648397,-1.51298531544935,
131.161554222262));
#45330=CARTESIAN_POINT('Ctrl Pts',(0.984066261457807,-1.19221104447402,
131.188479925973));
#45331=CARTESIAN_POINT('Ctrl Pts',(1.42542281590713,-0.598265109305461,
131.215405629683));
#45332=CARTESIAN_POINT('Ctrl Pts',(1.54017040244428,0.132762483030811,131.242331333393));
#45333=CARTESIAN_POINT('Ctrl Pts',(1.30201584504227,0.833369569997161,131.269257037104));
#45334=CARTESIAN_POINT('Ctrl Pts',(0.765528231107528,1.34302520522144,131.296182740814));
#45335=CARTESIAN_POINT('Ctrl Pts',(0.0536337437577054,1.54495099290438,
131.323108444524));
#45336=CARTESIAN_POINT('Ctrl Pts',(-0.670549905646045,1.39287940488435,
131.350034148235));
#45337=CARTESIAN_POINT('Ctrl Pts',(-1.24108926619491,0.921654858529432,
131.376959851945));
#45338=CARTESIAN_POINT('Ctrl Pts',(-1.5272556271745,0.23924989175532,131.403885555655));
#45339=CARTESIAN_POINT('Ctrl Pts',(-1.46347918893899,-0.497974833581676,
131.430811259366));
#45340=CARTESIAN_POINT('Ctrl Pts',(-1.064373158062,-1.12109769997607,131.457736963076));
#45341=CARTESIAN_POINT('Ctrl Pts',(-0.421385411338104,-1.48734145648005,
131.484662666786));
#45342=CARTESIAN_POINT('Ctrl Pts',(0.318155124966732,-1.51278801844595,
131.511588370497));
#45343=CARTESIAN_POINT('Ctrl Pts',(0.984796211311188,-1.19160676986845,
131.538514074207));
#45344=CARTESIAN_POINT('Ctrl Pts',(1.42578918929164,-0.597390541595174,
131.565439777918));
#45345=CARTESIAN_POINT('Ctrl Pts',(1.54008855298824,0.133706844523454,131.592365481628));
#45346=CARTESIAN_POINT('Ctrl Pts',(1.30150468580068,0.834167743387289,131.619291185338));
#45347=CARTESIAN_POINT('Ctrl Pts',(0.764704733786668,1.34349430269641,131.646216889049));
#45348=CARTESIAN_POINT('Ctrl Pts',(0.0526866252480262,1.54498362152493,
131.673142592759));
#45349=CARTESIAN_POINT('Ctrl Pts',(-0.671403663494357,1.39246809367885,
131.700068296469));
#45350=CARTESIAN_POINT('Ctrl Pts',(-1.24165403598166,0.920893873474695,
131.72699400018));
#45351=CARTESIAN_POINT('Ctrl Pts',(-1.52740200954285,0.238313601207157,
131.75391970389));
#45352=CARTESIAN_POINT('Ctrl Pts',(-1.46317364247562,-0.498871890610963,
131.7808454076));
#45353=CARTESIAN_POINT('Ctrl Pts',(-1.06368569482785,-1.1217499783357,131.807771111311));
#45354=CARTESIAN_POINT('Ctrl Pts',(-0.420473550977336,-1.4875994972457,
131.834696815021));
#45355=CARTESIAN_POINT('Ctrl Pts',(0.319082445887751,-1.51259269600317,
131.861622518732));
#45356=CARTESIAN_POINT('Ctrl Pts',(0.985526514083445,-1.19100283849842,
131.888548222442));
#45357=CARTESIAN_POINT('Ctrl Pts',(1.42615513825209,-0.596516381086395,
131.915473926152));
#45358=CARTESIAN_POINT('Ctrl Pts',(1.5400062975897,0.134650936292246,131.942399629863));
#45359=CARTESIAN_POINT('Ctrl Pts',(1.30099307334363,0.834965445012741,131.969325333573));
#45360=CARTESIAN_POINT('Ctrl Pts',(0.763880990933983,1.34396283540829,131.996251037283));
#45361=CARTESIAN_POINT('Ctrl Pts',(0.0517394976421782,1.54501562959783,
132.023176740994));
#45362=CARTESIAN_POINT('Ctrl Pts',(-0.672257158844581,1.39205624307012,
132.050102444704));
#45363=CARTESIAN_POINT('Ctrl Pts',(-1.24221833624253,0.920132532253928,
132.077028148414));
#45364=CARTESIAN_POINT('Ctrl Pts',(-1.52754781567707,0.237377216927905,
132.103953852125));
#45365=CARTESIAN_POINT('Ctrl Pts',(-1.46286754596235,-0.499768762552115,
132.130879555835));
#45366=CARTESIAN_POINT('Ctrl Pts',(-1.06299783240024,-1.12240183571076,
132.157805259545));
#45367=CARTESIAN_POINT('Ctrl Pts',(-0.41956153499722,-1.48785697890927,
132.184730963256));
#45368=CARTESIAN_POINT('Ctrl Pts',(0.320009642611874,-1.51239680311634,
132.211656666966));
#45369=CARTESIAN_POINT('Ctrl Pts',(0.986256436260319,-1.19039845717735,
132.238582370677));
#45370=CARTESIAN_POINT('Ctrl Pts',(1.42652053463166,-0.595641987092175,
132.265508074387));
#45371=CARTESIAN_POINT('Ctrl Pts',(1.53992342300198,0.135594986026619,132.292433778097));
#45372=CARTESIAN_POINT('Ctrl Pts',(1.30048090995801,0.835762871463845,132.319359481808));
#45373=CARTESIAN_POINT('Ctrl Pts',(0.763056801047929,1.34443089049341,132.346285185518));
#45374=CARTESIAN_POINT('Ctrl Pts',(0.0507921222485523,1.54504721797859,
132.373210889228));
#45375=CARTESIAN_POINT('Ctrl Pts',(-0.673111038284911,1.39164394701371,
132.400136592939));
#45376=CARTESIAN_POINT('Ctrl Pts',(-1.24278299799471,0.919371525228328,
132.427062296649));
#45377=CARTESIAN_POINT('Ctrl Pts',(-1.52769560301691,0.23644090515159,132.453988000359));
#45378=CARTESIAN_POINT('Ctrl Pts',(-1.46256384075252,-0.5006625304082,132.48091370407));
#45379=CARTESIAN_POINT('Ctrl Pts',(-1.06231992440674,-1.12305332384367,
132.50783940778));
#45380=CARTESIAN_POINT('Ctrl Pts',(-0.41865947125959,-1.4881012006264,132.53476511149));
#45381=CARTESIAN_POINT('Ctrl Pts',(0.320894284071444,-1.51220387038322,
132.561690815201));
#45382=CARTESIAN_POINT('Ctrl Pts',(0.986953317400244,-1.18973728399054,
132.588616518911));
#45383=CARTESIAN_POINT('Ctrl Pts',(1.28011883766499,-0.793113549367196,
132.606566988051));
#45384=CARTESIAN_POINT('Ctrl Pts',(1.37228238111194,-0.572007248306124,
132.615542222622));
#45385=CARTESIAN_POINT('',(-1.16302251498203,-0.926096109379588,132.5));
#45386=CARTESIAN_POINT('Ctrl Pts',(-1.16302251498205,-0.926096109379563,
132.5));
#45387=CARTESIAN_POINT('Ctrl Pts',(-1.12343887327884,-0.969761157109709,
132.5));
#45388=CARTESIAN_POINT('Ctrl Pts',(-1.08135544679353,-1.01098477954329,
132.5));
#45389=CARTESIAN_POINT('Ctrl Pts',(-1.03694177510552,-1.0495028422266,132.5));
#45390=CARTESIAN_POINT('Ctrl Pts',(-1.02884469989658,-1.05652508647247,
132.5));
#45391=CARTESIAN_POINT('Ctrl Pts',(-1.02067008828795,-1.06345729579591,
132.5));
#45392=CARTESIAN_POINT('Ctrl Pts',(-1.012418858982,-1.07029771551359,132.5));
#45393=CARTESIAN_POINT('Ctrl Pts',(-0.98167242007177,-1.0957870746347,132.5));
#45394=CARTESIAN_POINT('Ctrl Pts',(-0.94986244225381,-1.12000269225618,
132.5));
#45395=CARTESIAN_POINT('Ctrl Pts',(-0.91707717529942,-1.14289362846388,
132.5));
#45396=CARTESIAN_POINT('Ctrl Pts',(-0.901607681935602,-1.15369455274029,
132.5));
#45397=CARTESIAN_POINT('Ctrl Pts',(-0.885920995232433,-1.16420041056655,
132.5));
#45398=CARTESIAN_POINT('Ctrl Pts',(-0.870026136517583,-1.1744050442284,
132.5));
#45399=CARTESIAN_POINT('Ctrl Pts',(-0.859196579215699,-1.18135771156369,
132.5));
#45400=CARTESIAN_POINT('Ctrl Pts',(-0.848277795189246,-1.18816574517481,
132.5));
#45401=CARTESIAN_POINT('Ctrl Pts',(-0.837276000207708,-1.19482592504528,
132.5));
#45402=CARTESIAN_POINT('Ctrl Pts',(-0.7873206039329,-1.22506752882437,132.5));
#45403=CARTESIAN_POINT('Ctrl Pts',(-0.735635042660107,-1.25227756773128,
132.5));
#45404=CARTESIAN_POINT('Ctrl Pts',(-0.682504096094913,-1.27630821846757,
132.5));
#45405=CARTESIAN_POINT('Ctrl Pts',(-0.656532974943956,-1.28805472369579,
132.5));
#45406=CARTESIAN_POINT('Ctrl Pts',(-0.630216202837425,-1.29904081955767,
132.5));
#45407=CARTESIAN_POINT('Ctrl Pts',(-0.603585928569541,-1.30924482499605,
132.5));
#45408=CARTESIAN_POINT('Ctrl Pts',(-0.581793012479383,-1.31759528477973,
132.5));
#45409=CARTESIAN_POINT('Ctrl Pts',(-0.559790126733421,-1.32542192801966,
132.5));
#45410=CARTESIAN_POINT('Ctrl Pts',(-0.537594787919088,-1.33271132314286,
132.5));
#45411=CARTESIAN_POINT('Ctrl Pts',(-0.526294525446042,-1.33642255633695,
132.5));
#45412=CARTESIAN_POINT('Ctrl Pts',(-0.514943176335056,-1.33999474630347,
132.5));
#45413=CARTESIAN_POINT('Ctrl Pts',(-0.503559980499219,-1.34342124510912,
132.5));
#45414=CARTESIAN_POINT('Ctrl Pts',(-0.46487623766045,-1.35506558476089,
132.5));
#45415=CARTESIAN_POINT('Ctrl Pts',(-0.425780872220429,-1.36504338933051,
132.5));
#45416=CARTESIAN_POINT('Ctrl Pts',(-0.386368127474387,-1.37330780015286,
132.5));
#45417=CARTESIAN_POINT('Ctrl Pts',(-0.330299401943935,-1.38506478346002,
132.5));
#45418=CARTESIAN_POINT('Ctrl Pts',(-0.273587986529516,-1.39335645759698,
132.5));
#45419=CARTESIAN_POINT('Ctrl Pts',(-0.216553461875847,-1.39819529077566,
132.5));
#45420=CARTESIAN_POINT('Ctrl Pts',(-0.174416968678751,-1.40177016866855,
132.5));
#45421=CARTESIAN_POINT('Ctrl Pts',(-0.132103871869953,-1.40345934657106,
132.5));
#45422=CARTESIAN_POINT('Ctrl Pts',(-0.0897455132278829,-1.40324976814038,
132.5));
#45423=CARTESIAN_POINT('Ctrl Pts',(-0.0705591202545961,-1.40315483872719,
132.5));
#45424=CARTESIAN_POINT('Ctrl Pts',(-0.0513634969174188,-1.40267014032031,
132.5));
#45425=CARTESIAN_POINT('Ctrl Pts',(-0.0321712203893606,-1.40179344447432,
132.5));
#45426=CARTESIAN_POINT('Ctrl Pts',(-0.0192679054651587,-1.4012040259873,
132.5));
#45427=CARTESIAN_POINT('Ctrl Pts',(-0.00636610869756403,-1.40043740709029,
132.5));
#45428=CARTESIAN_POINT('Ctrl Pts',(0.00653026688444481,-1.39949275165764,
132.5));
#45429=CARTESIAN_POINT('Ctrl Pts',(0.017391646899733,-1.39869715900665,
132.5));
#45430=CARTESIAN_POINT('Ctrl Pts',(0.0282504431870717,-1.39777505085674,
132.5));
#45431=CARTESIAN_POINT('Ctrl Pts',(0.039086617545718,-1.39672789082918,
132.5));
#45432=CARTESIAN_POINT('Ctrl Pts',(0.0949958078773393,-1.3913250736217,
132.5));
#45433=CARTESIAN_POINT('Ctrl Pts',(0.150411388764911,-1.38259070029328,
132.5));
#45434=CARTESIAN_POINT('Ctrl Pts',(0.205031962417632,-1.3705335380372,132.5));
#45435=CARTESIAN_POINT('Ctrl Pts',(0.232388170204765,-1.36449482013398,
132.5));
#45436=CARTESIAN_POINT('Ctrl Pts',(0.259544834917365,-1.3576218081049,132.5));
#45437=CARTESIAN_POINT('Ctrl Pts',(0.286462690387675,-1.34991087227367,
132.5));
#45438=CARTESIAN_POINT('Ctrl Pts',(0.339060168306143,-1.3348437070026,132.5));
#45439=CARTESIAN_POINT('Ctrl Pts',(0.390747678696571,-1.31657948059088,
132.5));
#45440=CARTESIAN_POINT('Ctrl Pts',(0.44125190511673,-1.29524246473403,132.5));
#45441=CARTESIAN_POINT('Ctrl Pts',(0.461191169585947,-1.28681852811902,
132.5));
#45442=CARTESIAN_POINT('Ctrl Pts',(0.480945683432762,-1.2779152214623,132.5));
#45443=CARTESIAN_POINT('Ctrl Pts',(0.50049723434429,-1.26853868323638,132.5));
#45444=CARTESIAN_POINT('Ctrl Pts',(0.51016987966283,-1.26389987330333,132.5));
#45445=CARTESIAN_POINT('Ctrl Pts',(0.519792835446406,-1.25914522637774,
132.5));
#45446=CARTESIAN_POINT('Ctrl Pts',(0.529363810934624,-1.25427541756582,
132.5));
#45447=CARTESIAN_POINT('Ctrl Pts',(0.538615327196273,-1.24956815282879,
132.5));
#45448=CARTESIAN_POINT('Ctrl Pts',(0.54781100101367,-1.24475694311704,132.5));
#45449=CARTESIAN_POINT('Ctrl Pts',(0.556944545350045,-1.23984536162613,
132.5));
#45450=CARTESIAN_POINT('Ctrl Pts',(0.605505112344534,-1.21373182089604,
132.5));
#45451=CARTESIAN_POINT('Ctrl Pts',(0.652353503329041,-1.18476332689692,
132.5));
#45452=CARTESIAN_POINT('Ctrl Pts',(0.697227106842703,-1.1530956883318,132.5));
#45453=CARTESIAN_POINT('Ctrl Pts',(0.741542679959258,-1.12182185600332,
132.5));
#45454=CARTESIAN_POINT('Ctrl Pts',(0.78393305031491,-1.0879149147509,132.5));
#45455=CARTESIAN_POINT('Ctrl Pts',(0.824110992015511,-1.05148810793158,
132.5));
#45456=CARTESIAN_POINT('Ctrl Pts',(0.83326922342897,-1.04318491686743,132.5));
#45457=CARTESIAN_POINT('Ctrl Pts',(0.842312333357698,-1.03475067051344,
132.5));
#45458=CARTESIAN_POINT('Ctrl Pts',(0.851236602531774,-1.02618649277957,
132.5));
#45459=CARTESIAN_POINT('Ctrl Pts',(0.870313615897425,-1.00787923087299,
132.5));
#45460=CARTESIAN_POINT('Ctrl Pts',(0.888847746986408,-0.988978296120459,
132.5));
#45461=CARTESIAN_POINT('Ctrl Pts',(0.906815286248638,-0.969510836032861,
132.5));
#45462=CARTESIAN_POINT('Ctrl Pts',(0.915830068492709,-0.959743504459318,
132.5));
#45463=CARTESIAN_POINT('Ctrl Pts',(0.924702181967323,-0.949833545936108,
132.5));
#45464=CARTESIAN_POINT('Ctrl Pts',(0.933428374226774,-0.939784308310312,
132.5));
#45465=CARTESIAN_POINT('Ctrl Pts',(0.939813745749803,-0.932430801321692,
132.5));
#45466=CARTESIAN_POINT('Ctrl Pts',(0.946120382516669,-0.92500325455595,
132.5));
#45467=CARTESIAN_POINT('Ctrl Pts',(0.952338780021893,-0.917513345854709,
132.5));
#45468=CARTESIAN_POINT('Ctrl Pts',(0.986818201658188,-0.875983720270228,
132.5));
#45469=CARTESIAN_POINT('Ctrl Pts',(1.01865914174794,-0.832458627176748,
132.5));
#45470=CARTESIAN_POINT('Ctrl Pts',(1.04771225996938,-0.787203227418373,
132.5));
#45471=CARTESIAN_POINT('Ctrl Pts',(1.07693733284606,-0.74167997769622,132.5));
#45472=CARTESIAN_POINT('Ctrl Pts',(1.10334204163176,-0.694404893510236,
132.5));
#45473=CARTESIAN_POINT('Ctrl Pts',(1.12672619137727,-0.645625392877356,
132.5));
#45474=CARTESIAN_POINT('Ctrl Pts',(1.15011034112277,-0.596845892244476,
132.5));
#45475=CARTESIAN_POINT('Ctrl Pts',(1.17047445367726,-0.546560987753008,
132.5));
#45476=CARTESIAN_POINT('Ctrl Pts',(1.18756226708949,-0.495010526943894,
132.5));
#45477=CARTESIAN_POINT('Ctrl Pts',(-1.48668131839924,3.04819389219259E-5,
132.46254146791));
#45478=CARTESIAN_POINT('Ctrl Pts',(-1.48655520767872,-0.16343428003251,
132.46866554663));
#45479=CARTESIAN_POINT('Ctrl Pts',(-1.45963517263437,-0.326939632586996,
132.47478962535));
#45480=CARTESIAN_POINT('Ctrl Pts',(-1.40671181507228,-0.481543756720818,
132.48091370407));
#45481=CARTESIAN_POINT('Ctrl Pts',(-1.35173152550569,-0.642156762104989,
132.487275802713));
#45482=CARTESIAN_POINT('Ctrl Pts',(-1.26868733036522,-0.793163178418914,
132.493637901357));
#45483=CARTESIAN_POINT('Ctrl Pts',(-1.16302251498203,-0.926096109379588,
132.5));
#45484=CARTESIAN_POINT('',(-0.746857044344933,-1.04763739686609,131.));
#45485=CARTESIAN_POINT('Ctrl Pts',(-0.746861959042824,-1.04760678153428,
131.));
#45486=CARTESIAN_POINT('Ctrl Pts',(-0.79290540902848,-1.01977850456588,
131.));
#45487=CARTESIAN_POINT('Ctrl Pts',(-0.837111201294298,-0.989131878238612,
131.));
#45488=CARTESIAN_POINT('Ctrl Pts',(-0.879206377167662,-0.955837561748656,
131.));
#45489=CARTESIAN_POINT('Ctrl Pts',(-0.884791465636455,-0.95142015050743,
131.));
#45490=CARTESIAN_POINT('Ctrl Pts',(-0.890339378075958,-0.946956059295192,
131.));
#45491=CARTESIAN_POINT('Ctrl Pts',(-0.895849453575902,-0.942445622075628,
131.));
#45492=CARTESIAN_POINT('Ctrl Pts',(-0.926217339091838,-0.917587080461831,
131.));
#45493=CARTESIAN_POINT('Ctrl Pts',(-0.955436613451353,-0.891321827243511,
131.));
#45494=CARTESIAN_POINT('Ctrl Pts',(-0.983445198717416,-0.863753973035975,
131.));
#45495=CARTESIAN_POINT('Ctrl Pts',(-0.992679469403162,-0.854665008864478,
131.));
#45496=CARTESIAN_POINT('Ctrl Pts',(-1.00178207011453,-0.845434352437698,
131.));
#45497=CARTESIAN_POINT('Ctrl Pts',(-1.01075055479975,-0.836065450228404,
131.));
#45498=CARTESIAN_POINT('Ctrl Pts',(-1.01912420496792,-0.827317940218179,
131.));
#45499=CARTESIAN_POINT('Ctrl Pts',(-1.02737472791407,-0.818456358266283,
131.));
#45500=CARTESIAN_POINT('Ctrl Pts',(-1.0354984320536,-0.809486419032962,
131.));
#45501=CARTESIAN_POINT('Ctrl Pts',(-1.07199487788031,-0.769188188610594,
131.));
#45502=CARTESIAN_POINT('Ctrl Pts',(-1.10594836061416,-0.726691494335613,
131.));
#45503=CARTESIAN_POINT('Ctrl Pts',(-1.13720585307844,-0.682279068598729,
131.));
#45504=CARTESIAN_POINT('Ctrl Pts',(-1.15346249868424,-0.659180700534707,
131.));
#45505=CARTESIAN_POINT('Ctrl Pts',(-1.16898942799938,-0.635563406373612,
131.));
#45506=CARTESIAN_POINT('Ctrl Pts',(-1.18376147727168,-0.611462797325301,
131.));
#45507=CARTESIAN_POINT('Ctrl Pts',(-1.19227111129058,-0.597579323282302,
131.));
#45508=CARTESIAN_POINT('Ctrl Pts',(-1.20053018904277,-0.583535413960466,
131.));
#45509=CARTESIAN_POINT('Ctrl Pts',(-1.20853345336714,-0.569337528515594,
131.));
#45510=CARTESIAN_POINT('Ctrl Pts',(-1.21501758519943,-0.557834602055454,
131.));
#45511=CARTESIAN_POINT('Ctrl Pts',(-1.2213347587292,-0.546228423437439,
131.));
#45512=CARTESIAN_POINT('Ctrl Pts',(-1.22747166438142,-0.534543038687395,
131.));
#45513=CARTESIAN_POINT('Ctrl Pts',(-1.24489028000614,-0.50137596118562,
131.));
#45514=CARTESIAN_POINT('Ctrl Pts',(-1.2608770606582,-0.46753740688374,131.));
#45515=CARTESIAN_POINT('Ctrl Pts',(-1.27538574703159,-0.43311685629096,
131.));
#45516=CARTESIAN_POINT('Ctrl Pts',(-1.29685816110231,-0.382175489453921,
131.));
#45517=CARTESIAN_POINT('Ctrl Pts',(-1.31509556112442,-0.329960528095882,
131.));
#45518=CARTESIAN_POINT('Ctrl Pts',(-1.33010366412696,-0.276796734514434,
131.));
#45519=CARTESIAN_POINT('Ctrl Pts',(-1.34135974137886,-0.236923889328347,
131.));
#45520=CARTESIAN_POINT('Ctrl Pts',(-1.35079846340778,-0.196516449979369,
131.));
#45521=CARTESIAN_POINT('Ctrl Pts',(-1.35840472687476,-0.155702664587729,
131.));
#45522=CARTESIAN_POINT('Ctrl Pts',(-1.36226900717259,-0.134967660146506,
131.));
#45523=CARTESIAN_POINT('Ctrl Pts',(-1.36566007611252,-0.114127685083141,
131.));
#45524=CARTESIAN_POINT('Ctrl Pts',(-1.36857437917471,-0.0931991623570564,
131.));
#45525=CARTESIAN_POINT('Ctrl Pts',(-1.37032032486804,-0.0806609796967288,
131.));
#45526=CARTESIAN_POINT('Ctrl Pts',(-1.37189513129338,-0.0680910121185238,
131.));
#45527=CARTESIAN_POINT('Ctrl Pts',(-1.37329784488209,-0.0554927709829172,
131.));
#45528=CARTESIAN_POINT('Ctrl Pts',(-1.37435287170058,-0.0460172213261885,
131.));
#45529=CARTESIAN_POINT('Ctrl Pts',(-1.37530946257138,-0.0365353663362607,
131.));
#45530=CARTESIAN_POINT('Ctrl Pts',(-1.37616775261068,-0.0270488533894786,
131.));
#45531=CARTESIAN_POINT('Ctrl Pts',(-1.38126770774191,0.0293199592087556,
131.));
#45532=CARTESIAN_POINT('Ctrl Pts',(-1.38290082952566,0.0858515591714624,
131.));
#45533=CARTESIAN_POINT('Ctrl Pts',(-1.3810680521945,0.142217815274853,131.));
#45534=CARTESIAN_POINT('Ctrl Pts',(-1.38026175318832,0.167015184549204,
131.));
#45535=CARTESIAN_POINT('Ctrl Pts',(-1.3787840345135,0.191780836376777,131.));
#45536=CARTESIAN_POINT('Ctrl Pts',(-1.37663194421336,0.216487800262018,
131.));
#45537=CARTESIAN_POINT('Ctrl Pts',(-1.37167800010617,0.273361305122912,
131.));
#45538=CARTESIAN_POINT('Ctrl Pts',(-1.3631544857951,0.329924039407384,131.));
#45539=CARTESIAN_POINT('Ctrl Pts',(-1.35119091111081,0.385880739631646,
131.));
#45540=CARTESIAN_POINT('Ctrl Pts',(-1.34632600887317,0.408635132304057,
131.));
#45541=CARTESIAN_POINT('Ctrl Pts',(-1.34089162405852,0.431289287179278,
131.));
#45542=CARTESIAN_POINT('Ctrl Pts',(-1.33489389522501,0.45382298681954,131.));
#45543=CARTESIAN_POINT('Ctrl Pts',(-1.33224239577941,0.463784772982573,
131.));
#45544=CARTESIAN_POINT('Ctrl Pts',(-1.32948021180854,0.473724958560968,
131.));
#45545=CARTESIAN_POINT('Ctrl Pts',(-1.32660959425527,0.483635551674743,
131.));
#45546=CARTESIAN_POINT('Ctrl Pts',(-1.31067425301938,0.538651129399031,
131.));
#45547=CARTESIAN_POINT('Ctrl Pts',(-1.29146044376945,0.592556875483699,
131.));
#45548=CARTESIAN_POINT('Ctrl Pts',(-1.26913667157012,0.645068264124258,
131.));
#45549=CARTESIAN_POINT('Ctrl Pts',(-1.24656696606482,0.698158152639027,
131.));
#45550=CARTESIAN_POINT('Ctrl Pts',(-1.2208182026231,0.7498238393096,131.));
#45551=CARTESIAN_POINT('Ctrl Pts',(-1.19201211730027,0.799766583668426,
131.));
#45552=CARTESIAN_POINT('Ctrl Pts',(-1.18039996771779,0.819899226183185,
131.));
#45553=CARTESIAN_POINT('Ctrl Pts',(-1.16829042624204,0.839751747079717,
131.));
#45554=CARTESIAN_POINT('Ctrl Pts',(-1.1556892086837,0.859303760062855,131.));
#45555=CARTESIAN_POINT('Ctrl Pts',(-1.13970882525568,0.884098877107183,
131.));
#45556=CARTESIAN_POINT('Ctrl Pts',(-1.12293779488653,0.908410786623963,
131.));
#45557=CARTESIAN_POINT('Ctrl Pts',(-1.10540618886941,0.93221250033084,131.));
#45558=CARTESIAN_POINT('Ctrl Pts',(-1.09666464487149,0.944080422036999,
131.));
#45559=CARTESIAN_POINT('Ctrl Pts',(-1.08773396101947,0.955821468651418,
131.));
#45560=CARTESIAN_POINT('Ctrl Pts',(-1.07861760001237,0.96743209119293,131.));
#45561=CARTESIAN_POINT('Ctrl Pts',(-1.07225241782588,0.97553880479475,131.));
#45562=CARTESIAN_POINT('Ctrl Pts',(-1.06579920898365,0.98357864484497,131.));
#45563=CARTESIAN_POINT('Ctrl Pts',(-1.05926555171675,0.991543240500075,
131.));
#45564=CARTESIAN_POINT('Ctrl Pts',(-1.02223281978106,1.03668652301743,131.));
#45565=CARTESIAN_POINT('Ctrl Pts',(-0.982563863156014,1.07948549390314,
131.));
#45566=CARTESIAN_POINT('Ctrl Pts',(-0.940543142400786,1.11976824348413,
131.));
#45567=CARTESIAN_POINT('Ctrl Pts',(-0.896036753133427,1.16243385467282,
131.));
#45568=CARTESIAN_POINT('Ctrl Pts',(-0.848891793255228,1.20227795490809,
131.));
#45569=CARTESIAN_POINT('Ctrl Pts',(-0.799392172671262,1.23906470001876,
131.));
#45570=CARTESIAN_POINT('Ctrl Pts',(-0.752607904601772,1.27383347045292,
131.));
#45571=CARTESIAN_POINT('Ctrl Pts',(-0.703719130108104,1.30587158459506,
131.));
#45572=CARTESIAN_POINT('Ctrl Pts',(-0.652930875785528,1.33494126253536,
131.));
#45573=CARTESIAN_POINT('Ctrl Pts',(-0.649983132457026,1.33662846266368,
131.));
#45574=CARTESIAN_POINT('Ctrl Pts',(-0.647028982870071,1.33830565070331,
131.));
#45575=CARTESIAN_POINT('Ctrl Pts',(-0.644068464422466,1.33997277538071,
131.));
#45576=CARTESIAN_POINT('Ctrl Pts',(-0.746861959043068,-1.04760678153411,
131.));
#45577=CARTESIAN_POINT('Ctrl Pts',(-0.627129610382755,-1.13281069019958,
131.006362098643));
#45578=CARTESIAN_POINT('Ctrl Pts',(-0.303340278729474,-1.28908730893346,
131.021699431857));
#45579=CARTESIAN_POINT('Ctrl Pts',(0.274526574308514,-1.30932546829921,
131.046011999641));
#45580=CARTESIAN_POINT('Ctrl Pts',(0.851603122293372,-1.03172996338952,
131.072937703351));
#45581=CARTESIAN_POINT('Ctrl Pts',(1.23354957705434,-0.517733871181562,
131.099863407061));
#45582=CARTESIAN_POINT('Ctrl Pts',(1.3328512265448,0.114891597751729,131.126789110772));
#45583=CARTESIAN_POINT('Ctrl Pts',(1.12675416518279,0.721191403089574,131.153714814482));
#45584=CARTESIAN_POINT('Ctrl Pts',(0.662482047549443,1.16224333958056,131.180640518192));
#45585=CARTESIAN_POINT('Ctrl Pts',(0.0464142156206867,1.33698831153762,
131.207566221903));
#45586=CARTESIAN_POINT('Ctrl Pts',(-0.580288559487598,1.20538676777764,
131.234491925613));
#45587=CARTESIAN_POINT('Ctrl Pts',(-1.07402878803166,0.797592790182427,
131.261417629323));
#45588=CARTESIAN_POINT('Ctrl Pts',(-1.26566344030531,0.340612318858289,
131.282253402549));
#45589=CARTESIAN_POINT('Ctrl Pts',(-1.28660881016683,0.0666735963628725,
131.294113941204));
#45590=CARTESIAN_POINT('Ctrl Pts',(-1.28655804524971,2.50455016348322E-5,
131.296999245288));
#45591=CARTESIAN_POINT('Origin',(0.,0.,130.353000754712));
#45592=CARTESIAN_POINT('',(0.746857044345347,-1.04763739686579,131.));
#45593=CARTESIAN_POINT('Origin',(0.,0.,131.));
#45594=CARTESIAN_POINT('Ctrl Pts',(0.746857044345091,-1.04763739686597,
131.));
#45595=CARTESIAN_POINT('Ctrl Pts',(0.915655560497863,-0.927301523747248,
131.00897523457));
#45596=CARTESIAN_POINT('Ctrl Pts',(1.19383071914578,-0.603582305382327,
131.02692570371));
#45597=CARTESIAN_POINT('Ctrl Pts',(1.33763256702269,0.0204649803060436,
131.053851407421));
#45598=CARTESIAN_POINT('Ctrl Pts',(1.17488299294373,0.639781288322262,131.080777111131));
#45599=CARTESIAN_POINT('Ctrl Pts',(0.742945664266514,1.11253782599317,131.107702814841));
#45600=CARTESIAN_POINT('Ctrl Pts',(0.140763636876506,1.33036910873258,131.134628518552));
#45601=CARTESIAN_POINT('Ctrl Pts',(-0.49366903146045,1.24337802076997,131.161554222262));
#45602=CARTESIAN_POINT('Ctrl Pts',(-1.01498908290289,0.871488239228939,
131.188479925973));
#45603=CARTESIAN_POINT('Ctrl Pts',(-1.2525149888957,0.401316727103227,131.210628770122));
#45604=CARTESIAN_POINT('Ctrl Pts',(-1.28652850751777,0.0969951814981651,
131.223802379702));
#45605=CARTESIAN_POINT('Ctrl Pts',(-1.28651324097226,5.80358258382013E-6,
131.228000754712));
#45606=CARTESIAN_POINT('Ctrl Pts',(0.863027389440352,-1.21059280961881,
130.884457777378));
#45607=CARTESIAN_POINT('Ctrl Pts',(1.05808177613958,-1.07153921801113,130.893433011949));
#45608=CARTESIAN_POINT('Ctrl Pts',(1.37952586345563,-0.69746689178419,130.911383481089));
#45609=CARTESIAN_POINT('Ctrl Pts',(1.54569545951096,0.0236482184404665,
130.938309184799));
#45610=CARTESIAN_POINT('Ctrl Pts',(1.35763090135572,0.739296468118232,130.96523488851));
#45611=CARTESIAN_POINT('Ctrl Pts',(0.858507611306259,1.28558821650061,130.99216059222));
#45612=CARTESIAN_POINT('Ctrl Pts',(0.162658804628651,1.53730220206782,131.01908629593));
#45613=CARTESIAN_POINT('Ctrl Pts',(-0.570457089070449,1.43678003103469,
131.046011999641));
#45614=CARTESIAN_POINT('Ctrl Pts',(-1.17286619328369,1.00704442131793,131.072937703351));
#45615=CARTESIAN_POINT('Ctrl Pts',(-1.50653382270734,0.34656482765933,131.099863407061));
#45616=CARTESIAN_POINT('Ctrl Pts',(-1.49500734612767,-0.393324007405797,
131.126789110772));
#45617=CARTESIAN_POINT('Ctrl Pts',(-1.14092708773515,-1.04308939023749,
131.153714814482));
#45618=CARTESIAN_POINT('Ctrl Pts',(-0.525424324038318,-1.45384987150975,
131.180640518192));
#45619=CARTESIAN_POINT('Ctrl Pts',(0.210469861461765,-1.53148704892802,
131.207566221903));
#45620=CARTESIAN_POINT('Ctrl Pts',(0.898138679547195,-1.25821187382816,
131.234491925613));
#45621=CARTESIAN_POINT('Ctrl Pts',(1.38001538427226,-0.696640351025329,
131.261417629323));
#45622=CARTESIAN_POINT('Ctrl Pts',(1.54568670044473,0.0245536163580204,
131.288343333034));
#45623=CARTESIAN_POINT('Ctrl Pts',(1.35719207190964,0.740121575040211,131.315269036744));
#45624=CARTESIAN_POINT('Ctrl Pts',(0.857721606883694,1.28610416068526,131.342194740455));
#45625=CARTESIAN_POINT('Ctrl Pts',(0.16171986348354,1.53739941243649,131.369120444165));
#45626=CARTESIAN_POINT('Ctrl Pts',(-0.571337040454812,1.43642760104845,
131.396046147875));
#45627=CARTESIAN_POINT('Ctrl Pts',(-1.17348247162191,1.00632457743981,131.422971851586));
#45628=CARTESIAN_POINT('Ctrl Pts',(-1.50674577582422,0.345640612600471,
131.449897555296));
#45629=CARTESIAN_POINT('Ctrl Pts',(-1.49476573901151,-0.394240600839361,
131.476823259006));
#45630=CARTESIAN_POINT('Ctrl Pts',(-1.14028736834168,-1.04378876379489,
131.503748962717));
#45631=CARTESIAN_POINT('Ctrl Pts',(-0.52453292370194,-1.45417174974665,
131.530674666427));
#45632=CARTESIAN_POINT('Ctrl Pts',(0.211408683204288,-1.53135777481333,
131.557600370137));
#45633=CARTESIAN_POINT('Ctrl Pts',(0.898909842300872,-1.25766106771139,
131.584526073848));
#45634=CARTESIAN_POINT('Ctrl Pts',(1.38044218951963,-0.695794242015611,
131.611451777558));
#45635=CARTESIAN_POINT('Ctrl Pts',(1.54567136120299,0.0255011565974578,
131.638377481268));
#45636=CARTESIAN_POINT('Ctrl Pts',(1.35673810319962,0.740953429817608,131.665303184979));
#45637=CARTESIAN_POINT('Ctrl Pts',(0.856933029143843,1.28662972505494,131.692228888689));
#45638=CARTESIAN_POINT('Ctrl Pts',(0.160777365112824,1.53749826168993,131.7191545924));
#45639=CARTESIAN_POINT('Ctrl Pts',(-0.572217502707418,1.43607708547494,
131.74608029611));
#45640=CARTESIAN_POINT('Ctrl Pts',(-1.17409915580718,1.00560501100616,131.77300599982));
#45641=CARTESIAN_POINT('Ctrl Pts',(-1.50695737989574,0.344716870779641,
131.799931703531));
#45642=CARTESIAN_POINT('Ctrl Pts',(-1.49452377772872,-0.395156859511377,
131.826857407241));
#45643=CARTESIAN_POINT('Ctrl Pts',(-1.1396472826949,-1.04448759535701,131.853783110951));
#45644=CARTESIAN_POINT('Ctrl Pts',(-0.523641377640934,-1.45449302970016,
131.880708814662));
#45645=CARTESIAN_POINT('Ctrl Pts',(0.212347408168359,-1.53122788771527,
131.907634518372));
#45646=CARTESIAN_POINT('Ctrl Pts',(0.899680654475158,-1.25710977484312,
131.934560222082));
#45647=CARTESIAN_POINT('Ctrl Pts',(1.38086847141359,-0.694947862086922,
131.961485925793));
#45648=CARTESIAN_POINT('Ctrl Pts',(1.54565543818633,0.0264486909784084,
131.988411629503));
#45649=CARTESIAN_POINT('Ctrl Pts',(1.35628362403499,0.74178500846249,132.015337333214));
#45650=CARTESIAN_POINT('Ctrl Pts',(0.856144129802408,1.28715480656056,132.042263036924));
#45651=CARTESIAN_POINT('Ctrl Pts',(0.159834808689029,1.53759653349821,132.069188740634));
#45652=CARTESIAN_POINT('Ctrl Pts',(-0.573097745361402,1.43572602897267,
132.096114444345));
#45653=CARTESIAN_POINT('Ctrl Pts',(-1.17471538828929,1.00488506607529,132.123040148055));
#45654=CARTESIAN_POINT('Ctrl Pts',(-1.50716839969975,0.343792993074946,
132.149965851765));
#45655=CARTESIAN_POINT('Ctrl Pts',(-1.49428121352215,-0.396072971222168,
132.176891555476));
#45656=CARTESIAN_POINT('Ctrl Pts',(-1.13900670115657,-1.04518606185716,
132.203817259186));
#45657=CARTESIAN_POINT('Ctrl Pts',(-0.522749472625893,-1.45481376279687,
132.230742962896));
#45658=CARTESIAN_POINT('Ctrl Pts',(0.2132863055228,-1.53109754478736,132.257668666607));
#45659=CARTESIAN_POINT('Ctrl Pts',(0.900451768791074,-1.25655797749756,
132.284594370317));
#45660=CARTESIAN_POINT('Ctrl Pts',(1.38129516574151,-0.694101749712872,
132.311520074027));
#45661=CARTESIAN_POINT('Ctrl Pts',(1.5456414785732,0.027396491834726,132.338445777738));
#45662=CARTESIAN_POINT('Ctrl Pts',(1.35583202819204,0.742613936399278,132.365371481448));
#45663=CARTESIAN_POINT('Ctrl Pts',(0.855365099195844,1.28768122148057,132.392297185159));
#45664=CARTESIAN_POINT('Ctrl Pts',(0.158904313890113,1.53768343657436,132.419222888869));
#45665=CARTESIAN_POINT('Ctrl Pts',(-0.57393656553719,1.4353851436209,132.446148592579));
#45666=CARTESIAN_POINT('Ctrl Pts',(-1.17528939195008,1.00411479336165,132.47307429629));
#45667=CARTESIAN_POINT('Ctrl Pts',(-1.39656552507781,0.563327679862032,
132.49102476543));
#45668=CARTESIAN_POINT('Ctrl Pts',(-1.44969557651745,0.32974832986801,132.5));
#45669=CARTESIAN_POINT('Ctrl Pts',(0.824303941075265,-1.1562743387012,130.922971851586));
#45670=CARTESIAN_POINT('Ctrl Pts',(1.01060637092568,-1.02345998658984,130.931947086156));
#45671=CARTESIAN_POINT('Ctrl Pts',(1.31762748201901,-0.666172029650235,
130.949897555296));
#45672=CARTESIAN_POINT('Ctrl Pts',(1.47634116201487,0.0225871390623255,
130.976823259006));
#45673=CARTESIAN_POINT('Ctrl Pts',(1.29671493188506,0.706124741519575,131.003748962717));
#45674=CARTESIAN_POINT('Ctrl Pts',(0.81998696229301,1.22790475299813,131.030674666427));
#45675=CARTESIAN_POINT('Ctrl Pts',(0.155360415377937,1.46832450428941,131.057600370137));
#45676=CARTESIAN_POINT('Ctrl Pts',(-0.544861069867116,1.37231269427979,
131.084526073848));
#45677=CARTESIAN_POINT('Ctrl Pts',(-1.12024048982342,0.961859027288264,
131.111451777558));
#45678=CARTESIAN_POINT('Ctrl Pts',(-1.43893668105498,0.331014701008398,
131.138377481268));
#45679=CARTESIAN_POINT('Ctrl Pts',(-1.42792738959148,-0.375675828358543,
131.165303184979));
#45680=CARTESIAN_POINT('Ctrl Pts',(-1.08973447008383,-0.996286683119207,
131.192228888689));
#45681=CARTESIAN_POINT('Ctrl Pts',(-0.501848894184519,-1.3886166226942,
131.2191545924));
#45682=CARTESIAN_POINT('Ctrl Pts',(0.201026222809685,-1.46277027309148,
131.24608029611));
#45683=CARTESIAN_POINT('Ctrl Pts',(0.857839811622868,-1.20175676808682,
131.27300599982));
#45684=CARTESIAN_POINT('Ctrl Pts',(1.31809503837159,-0.665382575209595,
131.299931703531));
#45685=CARTESIAN_POINT('Ctrl Pts',(1.47633279596194,0.0234519123949133,
131.326857407241));
#45686=CARTESIAN_POINT('Ctrl Pts',(1.29629579241592,0.706912826458615,131.353783110951));
#45687=CARTESIAN_POINT('Ctrl Pts',(0.819236225350996,1.22839754712029,131.380708814662));
#45688=CARTESIAN_POINT('Ctrl Pts',(0.154463603879457,1.46841735289536,131.407634518372));
#45689=CARTESIAN_POINT('Ctrl Pts',(-0.545701538435044,1.37197607758584,
131.434560222082));
#45690=CARTESIAN_POINT('Ctrl Pts',(-1.12082911617435,0.961171482312347,
131.461485925793));
#45691=CARTESIAN_POINT('Ctrl Pts',(-1.43913912398055,0.330131954846758,
131.488411629503));
#45692=CARTESIAN_POINT('Ctrl Pts',(-1.42769662322128,-0.376551294871999,
131.515337333214));
#45693=CARTESIAN_POINT('Ctrl Pts',(-1.08912345446176,-0.996954676263693,
131.542263036924));
#45694=CARTESIAN_POINT('Ctrl Pts',(-0.500997490371219,-1.38892405847489,
131.569188740634));
#45695=CARTESIAN_POINT('Ctrl Pts',(0.20192292026309,-1.46264679941786,131.596114444345));
#45696=CARTESIAN_POINT('Ctrl Pts',(0.85857637283152,-1.20123067626358,131.623040148055));
#45697=CARTESIAN_POINT('Ctrl Pts',(1.3185026931596,-0.664574430532121,131.649965851765));
#45698=CARTESIAN_POINT('Ctrl Pts',(1.47631814498149,0.0243569371522413,
131.676891555476));
#45699=CARTESIAN_POINT('Ctrl Pts',(1.29586219297125,0.707707356481415,131.703817259186));
#45700=CARTESIAN_POINT('Ctrl Pts',(0.818483030554682,1.22889952977637,131.730742962896));
#45701=CARTESIAN_POINT('Ctrl Pts',(0.153563394765651,1.46851176685045,131.757668666607));
#45702=CARTESIAN_POINT('Ctrl Pts',(-0.546542494948905,1.37164128940625,
131.784594370317));
#45703=CARTESIAN_POINT('Ctrl Pts',(-1.12141813016224,0.960484202332149,
131.811520074027));
#45704=CARTESIAN_POINT('Ctrl Pts',(-1.43934123352219,0.32924966068928,131.838445777738));
#45705=CARTESIAN_POINT('Ctrl Pts',(-1.42746551857567,-0.377426441644429,
131.865371481448));
#45706=CARTESIAN_POINT('Ctrl Pts',(-1.08851208901992,-0.997622151731854,
131.892297185159));
#45707=CARTESIAN_POINT('Ctrl Pts',(-0.500145947371855,-1.38923092281675,
131.919222888869));
#45708=CARTESIAN_POINT('Ctrl Pts',(0.202819525280424,-1.462522740265,131.946148592579));
#45709=CARTESIAN_POINT('Ctrl Pts',(0.859312599191039,-1.20070411952904,
131.97307429629));
#45710=CARTESIAN_POINT('Ctrl Pts',(1.31890984807669,-0.663766027091625,
132.));
#45711=CARTESIAN_POINT('Ctrl Pts',(1.47630293641969,0.0252619563139483,
132.02692570371));
#45712=CARTESIAN_POINT('Ctrl Pts',(1.29542810597572,0.70850162276158,132.053851407421));
#45713=CARTESIAN_POINT('Ctrl Pts',(0.817729528586826,1.22940105123416,132.080777111131));
#45714=CARTESIAN_POINT('Ctrl Pts',(0.152663130203568,1.46860562926994,132.107702814841));
#45715=CARTESIAN_POINT('Ctrl Pts',(-0.547383241717385,1.371305984569,132.134628518552));
#45716=CARTESIAN_POINT('Ctrl Pts',(-1.12200671271459,0.959796560837642,
132.161554222262));
#45717=CARTESIAN_POINT('Ctrl Pts',(-1.43954278501201,0.328367236744954,
132.188479925973));
#45718=CARTESIAN_POINT('Ctrl Pts',(-1.42723383805905,-0.378301448049683,
132.215405629683));
#45719=CARTESIAN_POINT('Ctrl Pts',(-1.08790024993684,-0.998289278518124,
132.242331333393));
#45720=CARTESIAN_POINT('Ctrl Pts',(-0.499294061524478,-1.38953726483889,
132.269257037104));
#45721=CARTESIAN_POINT('Ctrl Pts',(0.203716294953091,-1.46239824573507,
132.296182740814));
#45722=CARTESIAN_POINT('Ctrl Pts',(0.8600491141353,-1.20017708095276,132.323108444524));
#45723=CARTESIAN_POINT('Ctrl Pts',(1.31931739692212,-0.662957879200776,
132.350034148235));
#45724=CARTESIAN_POINT('Ctrl Pts',(1.47628960316484,0.0261672299944563,
132.376959851945));
#45725=CARTESIAN_POINT('Ctrl Pts',(1.2949967729292,0.709293357269108,132.403885555655));
#45726=CARTESIAN_POINT('Ctrl Pts',(0.816985452550462,1.22990384627695,132.430811259366));
#45727=CARTESIAN_POINT('Ctrl Pts',(0.15177438606951,1.46868863306454,132.457736963076));
#45728=CARTESIAN_POINT('Ctrl Pts',(-0.54818442460592,1.37098039450968,132.484662666787));
#45729=CARTESIAN_POINT('Ctrl Pts',(-1.12255496122393,0.959060849733538,
132.511588370497));
#45730=CARTESIAN_POINT('Ctrl Pts',(-1.33390258568503,0.538051552370983,
132.529538839637));
#45731=CARTESIAN_POINT('Ctrl Pts',(-1.38464872807528,0.314952747964871,
132.538514074207));
#45732=CARTESIAN_POINT('Ctrl Pts',(0.785580492710178,-1.10195586778359,
130.961485925793));
#45733=CARTESIAN_POINT('Ctrl Pts',(0.96313096571177,-0.975380755168544,
130.970461160363));
#45734=CARTESIAN_POINT('Ctrl Pts',(1.2557291005824,-0.634877167516282,130.988411629503));
#45735=CARTESIAN_POINT('Ctrl Pts',(1.40698686451878,0.0215260596841844,
131.015337333214));
#45736=CARTESIAN_POINT('Ctrl Pts',(1.23579896241439,0.672953014920919,131.042263036924));
#45737=CARTESIAN_POINT('Ctrl Pts',(0.781466313279763,1.17022128949565,131.069188740634));
#45738=CARTESIAN_POINT('Ctrl Pts',(0.14806202612722,1.399346806511,131.096114444345));
#45739=CARTESIAN_POINT('Ctrl Pts',(-0.519265050663783,1.30784535752488,
131.123040148055));
#45740=CARTESIAN_POINT('Ctrl Pts',(-1.06761478636316,0.916673633258601,
131.149965851765));
#45741=CARTESIAN_POINT('Ctrl Pts',(-1.37133953940263,0.315464574357466,
131.176891555476));
#45742=CARTESIAN_POINT('Ctrl Pts',(-1.36084743305529,-0.358027649311288,
131.203817259186));
#45743=CARTESIAN_POINT('Ctrl Pts',(-1.0385418524325,-0.949483976000927,
131.230742962896));
#45744=CARTESIAN_POINT('Ctrl Pts',(-0.478273464330721,-1.32338337387865,
131.257668666607));
#45745=CARTESIAN_POINT('Ctrl Pts',(0.191582584157607,-1.39405349725495,
131.284594370317));
#45746=CARTESIAN_POINT('Ctrl Pts',(0.817540943698542,-1.14530166234549,
131.311520074027));
#45747=CARTESIAN_POINT('Ctrl Pts',(1.25617469247093,-0.63412479939386,131.338445777738));
#45748=CARTESIAN_POINT('Ctrl Pts',(1.40697889147916,0.0223502084318068,
131.365371481448));
#45749=CARTESIAN_POINT('Ctrl Pts',(1.23539951292219,0.673704077877018,131.392297185159));
#45750=CARTESIAN_POINT('Ctrl Pts',(0.7807508438183,1.17069093355532,131.419222888869));
#45751=CARTESIAN_POINT('Ctrl Pts',(0.147207344275373,1.39943529335423,131.446148592579));
#45752=CARTESIAN_POINT('Ctrl Pts',(-0.520066036415274,1.30752455412324,
131.47307429629));
#45753=CARTESIAN_POINT('Ctrl Pts',(-1.06817576072678,0.916018387184884,
131.5));
#45754=CARTESIAN_POINT('Ctrl Pts',(-1.37153247213689,0.314623297093045,
131.52692570371));
#45755=CARTESIAN_POINT('Ctrl Pts',(-1.36062750743105,-0.358861988904637,
131.553851407421));
#45756=CARTESIAN_POINT('Ctrl Pts',(-1.03795954058184,-0.950120588732497,
131.580777111131));
#45757=CARTESIAN_POINT('Ctrl Pts',(-0.477462057040497,-1.32367636720312,
131.607702814841));
#45758=CARTESIAN_POINT('Ctrl Pts',(0.19243715732189,-1.39393582402238,131.634628518552));
#45759=CARTESIAN_POINT('Ctrl Pts',(0.81824290336217,-1.14480028481577,131.661554222262));
#45760=CARTESIAN_POINT('Ctrl Pts',(1.25656319679956,-0.633354619048632,
131.688479925973));
#45761=CARTESIAN_POINT('Ctrl Pts',(1.40696492875998,0.0232127177070255,
131.715405629683));
#45762=CARTESIAN_POINT('Ctrl Pts',(1.23498628274288,0.674461283145224,131.742331333393));
#45763=CARTESIAN_POINT('Ctrl Pts',(0.780033031965522,1.17116933449779,131.769257037104));
#45764=CARTESIAN_POINT('Ctrl Pts',(0.146349424418478,1.39952527201097,131.796182740814));
#45765=CARTESIAN_POINT('Ctrl Pts',(-0.520867487190394,1.30720549333756,
131.823108444524));
#45766=CARTESIAN_POINT('Ctrl Pts',(-1.0687371045173,0.91536339365814,131.850034148235));
#45767=CARTESIAN_POINT('Ctrl Pts',(-1.37172508714864,0.313782450598919,
131.876959851945));
#45768=CARTESIAN_POINT('Ctrl Pts',(-1.36040725942262,-0.35969602377748,
131.903885555655));
#45769=CARTESIAN_POINT('Ctrl Pts',(-1.03737689534494,-0.950756708106701,
131.930811259366));
#45770=CARTESIAN_POINT('Ctrl Pts',(-0.476650517102775,-1.32396881593333,
131.957736963076));
#45771=CARTESIAN_POINT('Ctrl Pts',(0.193291642392489,-1.39381759281473,
131.984662666786));
#45772=CARTESIAN_POINT('Ctrl Pts',(0.818944543906922,-1.14429846421496,
132.011588370497));
#45773=CARTESIAN_POINT('Ctrl Pts',(1.2569512247398,-0.63258419209633,132.038514074207));
#45774=CARTESIAN_POINT('Ctrl Pts',(1.40695043465305,0.0240752216494901,
132.065439777918));
#45775=CARTESIAN_POINT('Ctrl Pts',(1.23457258791645,0.675218237060669,132.092365481628));
#45776=CARTESIAN_POINT('Ctrl Pts',(0.779314927371245,1.17164729590776,132.119291185338));
#45777=CARTESIAN_POINT('Ctrl Pts',(0.145491451718108,1.39961472504167,132.146216889049));
#45778=CARTESIAN_POINT('Ctrl Pts',(-0.52166873807337,1.30688594016532,132.173142592759));
#45779=CARTESIAN_POINT('Ctrl Pts',(-1.06929803713989,0.914708055599997,
132.200068296469));
#45780=CARTESIAN_POINT('Ctrl Pts',(-1.37191717032426,0.312941480414962,
132.22699400018));
#45781=CARTESIAN_POINT('Ctrl Pts',(-1.36018646259596,-0.360529924877197,
132.25391970389));
#45782=CARTESIAN_POINT('Ctrl Pts',(-1.03679379871711,-0.951392495179094,
132.2808454076));
#45783=CARTESIAN_POINT('Ctrl Pts',(-0.475838650423062,-1.32426076688091,
132.307771111311));
#45784=CARTESIAN_POINT('Ctrl Pts',(0.194146284383382,-1.39369894668277,
132.334696815021));
#45785=CARTESIAN_POINT('Ctrl Pts',(0.819646459479526,-1.14379618440796,
132.361622518732));
#45786=CARTESIAN_POINT('Ctrl Pts',(1.25733962810273,-0.631814008688681,
132.388548222442));
#45787=CARTESIAN_POINT('Ctrl Pts',(1.40693772775649,0.0249379681541858,
132.415473926152));
#45788=CARTESIAN_POINT('Ctrl Pts',(1.23416151766636,0.675972778138939,132.442399629863));
#45789=CARTESIAN_POINT('Ctrl Pts',(0.77860580590508,1.17212647107333,132.469325333573));
#45790=CARTESIAN_POINT('Ctrl Pts',(0.144644458248906,1.39969382955471,132.496251037283));
#45791=CARTESIAN_POINT('Ctrl Pts',(-0.522432283674648,1.30657564539846,
132.523176740994));
#45792=CARTESIAN_POINT('Ctrl Pts',(-1.06982053049778,0.914006906105429,
132.550102444704));
#45793=CARTESIAN_POINT('Ctrl Pts',(-1.27123964629225,0.512775424879935,
132.568052913844));
#45794=CARTESIAN_POINT('Ctrl Pts',(-1.31960187963311,0.300157166061732,
132.577028148414));
#45795=CARTESIAN_POINT('Ctrl Pts',(0.746857044345091,-1.04763739686597,
131.));
#45796=CARTESIAN_POINT('Ctrl Pts',(0.915655560497863,-0.927301523747248,
131.00897523457));
#45797=CARTESIAN_POINT('Ctrl Pts',(1.19383071914578,-0.603582305382327,
131.02692570371));
#45798=CARTESIAN_POINT('Ctrl Pts',(1.33763256702269,0.0204649803060436,
131.053851407421));
#45799=CARTESIAN_POINT('Ctrl Pts',(1.17488299294373,0.639781288322262,131.080777111131));
#45800=CARTESIAN_POINT('Ctrl Pts',(0.742945664266514,1.11253782599317,131.107702814841));
#45801=CARTESIAN_POINT('Ctrl Pts',(0.140763636876506,1.33036910873258,131.134628518552));
#45802=CARTESIAN_POINT('Ctrl Pts',(-0.49366903146045,1.24337802076997,131.161554222262));
#45803=CARTESIAN_POINT('Ctrl Pts',(-1.01498908290289,0.871488239228939,
131.188479925973));
#45804=CARTESIAN_POINT('Ctrl Pts',(-1.30374239775027,0.299914447706534,
131.215405629683));
#45805=CARTESIAN_POINT('Ctrl Pts',(-1.2937674765191,-0.340379470264034,
131.242331333393));
#45806=CARTESIAN_POINT('Ctrl Pts',(-0.98734923478118,-0.902681268882645,
131.269257037104));
#45807=CARTESIAN_POINT('Ctrl Pts',(-0.454698034476922,-1.2581501250631,
131.296182740814));
#45808=CARTESIAN_POINT('Ctrl Pts',(0.182138945505527,-1.32533672141841,
131.323108444524));
#45809=CARTESIAN_POINT('Ctrl Pts',(0.777242075774215,-1.08884655660415,
131.350034148235));
#45810=CARTESIAN_POINT('Ctrl Pts',(1.19425434657027,-0.602867023578126,
131.376959851945));
#45811=CARTESIAN_POINT('Ctrl Pts',(1.33762498699637,0.0212485044686996,
131.403885555655));
#45812=CARTESIAN_POINT('Ctrl Pts',(1.17450323342847,0.640495329295421,131.430811259366));
#45813=CARTESIAN_POINT('Ctrl Pts',(0.742265462285602,1.11298431999035,131.457736963076));
#45814=CARTESIAN_POINT('Ctrl Pts',(0.139951084671291,1.3304532338131,131.484662666786));
#45815=CARTESIAN_POINT('Ctrl Pts',(-0.494430534395506,1.24307303066064,
131.511588370497));
#45816=CARTESIAN_POINT('Ctrl Pts',(-1.01552240527922,0.870865292057418,
131.538514074207));
#45817=CARTESIAN_POINT('Ctrl Pts',(-1.30392582029322,0.299114639339331,
131.565439777918));
#45818=CARTESIAN_POINT('Ctrl Pts',(-1.29355839164082,-0.341172682937275,
131.592365481628));
#45819=CARTESIAN_POINT('Ctrl Pts',(-0.986795626701916,-0.903286501201301,
131.619291185338));
#45820=CARTESIAN_POINT('Ctrl Pts',(-0.453926623709776,-1.25842867593135,
131.646216889049));
#45821=CARTESIAN_POINT('Ctrl Pts',(0.182951394380693,-1.3252248486269,131.673142592759));
#45822=CARTESIAN_POINT('Ctrl Pts',(0.777909433892818,-1.08836989336796,
131.700068296469));
#45823=CARTESIAN_POINT('Ctrl Pts',(1.19462370043953,-0.602134807565142,
131.72699400018));
#45824=CARTESIAN_POINT('Ctrl Pts',(1.33761171253848,0.0220684982618089,
131.75391970389));
#45825=CARTESIAN_POINT('Ctrl Pts',(1.17411037251451,0.641215209809031,131.7808454076));
#45826=CARTESIAN_POINT('Ctrl Pts',(0.741583033376361,1.11343913921922,131.807771111311));
#45827=CARTESIAN_POINT('Ctrl Pts',(0.139135454071305,1.33053877717148,131.834696815021));
#45828=CARTESIAN_POINT('Ctrl Pts',(-0.495192479431881,1.24276969726887,
131.861622518732));
#45829=CARTESIAN_POINT('Ctrl Pts',(-1.01605607887236,0.870242584984128,
131.888548222442));
#45830=CARTESIAN_POINT('Ctrl Pts',(-1.3041089407751,0.298315240508559,131.915473926152));
#45831=CARTESIAN_POINT('Ctrl Pts',(-1.29334900026956,-0.341965605910532,
131.942399629863));
#45832=CARTESIAN_POINT('Ctrl Pts',(-0.986241701669955,-0.903891264481546,
131.969325333573));
#45833=CARTESIAN_POINT('Ctrl Pts',(-0.453155086833697,-1.25870670904991,
131.996251037283));
#45834=CARTESIAN_POINT('Ctrl Pts',(0.183763759504555,-1.32511244536446,
132.023176740994));
#45835=CARTESIAN_POINT('Ctrl Pts',(0.778576488622803,-1.08789280890088,
132.050102444704));
#45836=CARTESIAN_POINT('Ctrl Pts',(1.1949926014029,-0.601402357101034,132.077028148414));
#45837=CARTESIAN_POINT('Ctrl Pts',(1.3375979328864,0.02288848698503,132.103953852125));
#45838=CARTESIAN_POINT('Ctrl Pts',(1.17371706985718,0.641934851359759,132.130879555835));
#45839=CARTESIAN_POINT('Ctrl Pts',(0.740900326155663,1.11389354058136,132.157805259545));
#45840=CARTESIAN_POINT('Ctrl Pts',(0.138319773232647,1.3306238208134,132.184730963256));
#45841=CARTESIAN_POINT('Ctrl Pts',(-0.495954234429353,1.24246589576165,
132.211656666966));
#45842=CARTESIAN_POINT('Ctrl Pts',(-1.01658936156519,0.869619550362351,
132.238582370677));
#45843=CARTESIAN_POINT('Ctrl Pts',(-1.30429155563652,0.29751572408497,132.265508074387));
#45844=CARTESIAN_POINT('Ctrl Pts',(-1.29313908713286,-0.342758401704713,
132.292433778097));
#45845=CARTESIAN_POINT('Ctrl Pts',(-0.98568734749738,-0.904495711840062,
132.319359481808));
#45846=CARTESIAN_POINT('Ctrl Pts',(-0.452383239321647,-1.25898426892294,
132.346285185518));
#45847=CARTESIAN_POINT('Ctrl Pts',(0.184576273813673,-1.32499964763048,
132.373210889228));
#45848=CARTESIAN_POINT('Ctrl Pts',(0.779243804823753,-1.08741528786317,
132.400136592939));
#45849=CARTESIAN_POINT('Ctrl Pts',(1.19536185928334,-0.600670138176585,
132.427062296649));
#45850=CARTESIAN_POINT('Ctrl Pts',(1.33758585234813,0.0237087063139161,
132.453988000359));
#45851=CARTESIAN_POINT('Ctrl Pts',(1.17332626240353,0.642652199008768,132.48091370407));
#45852=CARTESIAN_POINT('Ctrl Pts',(0.740226159259698,1.11434909586972,132.50783940778));
#45853=CARTESIAN_POINT('Ctrl Pts',(0.137514530428304,1.33069902604488,132.53476511149));
#45854=CARTESIAN_POINT('Ctrl Pts',(-0.496680142743377,1.24217089628724,
132.561690815201));
#45855=CARTESIAN_POINT('Ctrl Pts',(-1.01708609977163,0.868952962477321,
132.588616518911));
#45856=CARTESIAN_POINT('Ctrl Pts',(-1.20857670689947,0.487499297388886,
132.606566988051));
#45857=CARTESIAN_POINT('Ctrl Pts',(-1.25455503119094,0.285361584158592,
132.615542222622));
#45858=CARTESIAN_POINT('Ctrl Pts',(0.855148668267253,0.961251009261909,
132.5));
#45859=CARTESIAN_POINT('Ctrl Pts',(0.817772472755866,0.999947679620164,
132.5));
#45860=CARTESIAN_POINT('Ctrl Pts',(0.778057507095388,1.03622562444653,132.5));
#45861=CARTESIAN_POINT('Ctrl Pts',(0.73623089071545,1.06985670395616,132.5));
#45862=CARTESIAN_POINT('Ctrl Pts',(0.730681434083883,1.07431879612054,132.5));
#45863=CARTESIAN_POINT('Ctrl Pts',(0.725094740290237,1.0787342570656,132.5));
#45864=CARTESIAN_POINT('Ctrl Pts',(0.719471281991385,1.08310251676537,132.5));
#45865=CARTESIAN_POINT('Ctrl Pts',(0.68847850560881,1.10717747008791,132.5));
#45866=CARTESIAN_POINT('Ctrl Pts',(0.656369876840734,1.12981958755506,132.5));
#45867=CARTESIAN_POINT('Ctrl Pts',(0.623260709674728,1.15099151444455,132.5));
#45868=CARTESIAN_POINT('Ctrl Pts',(0.612344806238366,1.15797177789632,132.5));
#45869=CARTESIAN_POINT('Ctrl Pts',(0.601320062392497,1.16479214312164,132.5));
#45870=CARTESIAN_POINT('Ctrl Pts',(0.590190382497418,1.1714509923087,132.5));
#45871=CARTESIAN_POINT('Ctrl Pts',(0.579798878378454,1.17766819346878,132.5));
#45872=CARTESIAN_POINT('Ctrl Pts',(0.569323560724368,1.18373997106925,132.5));
#45873=CARTESIAN_POINT('Ctrl Pts',(0.558770822371714,1.18966399771288,132.5));
#45874=CARTESIAN_POINT('Ctrl Pts',(0.511361729429498,1.21627820156729,132.5));
#45875=CARTESIAN_POINT('Ctrl Pts',(0.462375155234433,1.23992399549733,132.5));
#45876=CARTESIAN_POINT('Ctrl Pts',(0.412120795241606,1.26051510291273,132.5));
#45877=CARTESIAN_POINT('Ctrl Pts',(0.385984107461683,1.27122429004864,132.5));
#45878=CARTESIAN_POINT('Ctrl Pts',(0.35950388129632,1.28110658448462,132.5));
#45879=CARTESIAN_POINT('Ctrl Pts',(0.33272043457049,1.29014537761593,132.5));
#45880=CARTESIAN_POINT('Ctrl Pts',(0.317291476468849,1.29535229373617,132.5));
#45881=CARTESIAN_POINT('Ctrl Pts',(0.301761859550774,1.30027923535042,132.5));
#45882=CARTESIAN_POINT('Ctrl Pts',(0.286139050856096,1.30492251440297,132.5));
#45883=CARTESIAN_POINT('Ctrl Pts',(0.273481671713227,1.30868443356764,132.5));
#45884=CARTESIAN_POINT('Ctrl Pts',(0.260760780877808,1.31226060465732,132.5));
#45885=CARTESIAN_POINT('Ctrl Pts',(0.248002783150692,1.31564340253996,132.5));
#45886=CARTESIAN_POINT('Ctrl Pts',(0.21179126686695,1.32524492804826,132.5));
#45887=CARTESIAN_POINT('Ctrl Pts',(0.175243722368574,1.33330110003331,132.5));
#45888=CARTESIAN_POINT('Ctrl Pts',(0.138457680367238,1.33978673029291,132.5));
#45889=CARTESIAN_POINT('Ctrl Pts',(0.0840154582679713,1.34938526560242,
132.5));
#45890=CARTESIAN_POINT('Ctrl Pts',(0.0290514316829271,1.35554649398119,
132.5));
#45891=CARTESIAN_POINT('Ctrl Pts',(-0.0261190517268831,1.35834825553041,
132.5));
#45892=CARTESIAN_POINT('Ctrl Pts',(-0.0674969142842407,1.36044957669233,
132.5));
#45893=CARTESIAN_POINT('Ctrl Pts',(-0.108991568028323,1.36066014913089,
132.5));
#45894=CARTESIAN_POINT('Ctrl Pts',(-0.150474619481714,1.358993786071,132.5));
#45895=CARTESIAN_POINT('Ctrl Pts',(-0.171549637335457,1.35814720825168,
132.5));
#45896=CARTESIAN_POINT('Ctrl Pts',(-0.192621694545607,1.35681592531128,
132.5));
#45897=CARTESIAN_POINT('Ctrl Pts',(-0.213673988956076,1.35500012630149,
132.5));
#45898=CARTESIAN_POINT('Ctrl Pts',(-0.226286322656649,1.35391228938462,
132.5));
#45899=CARTESIAN_POINT('Ctrl Pts',(-0.238891562291373,1.35265053120959,
132.5));
#45900=CARTESIAN_POINT('Ctrl Pts',(-0.25148607234807,1.35121470346695,132.5));
#45901=CARTESIAN_POINT('Ctrl Pts',(-0.260958815768057,1.35013477040563,
132.5));
#45902=CARTESIAN_POINT('Ctrl Pts',(-0.270415802374623,1.34895746632245,
132.5));
#45903=CARTESIAN_POINT('Ctrl Pts',(-0.279855456160633,1.34768328952174,
132.5));
#45904=CARTESIAN_POINT('Ctrl Pts',(-0.335945831775187,1.34011213734059,
132.5));
#45905=CARTESIAN_POINT('Ctrl Pts',(-0.391423470349234,1.32912484896805,
132.5));
#45906=CARTESIAN_POINT('Ctrl Pts',(-0.445968675489026,1.31479535128022,
132.5));
#45907=CARTESIAN_POINT('Ctrl Pts',(-0.469964904553905,1.30849133412563,
132.5));
#45908=CARTESIAN_POINT('Ctrl Pts',(-0.493780806466491,1.30153978899266,
132.5));
#45909=CARTESIAN_POINT('Ctrl Pts',(-0.517389430066538,1.29394383943621,
132.5));
#45910=CARTESIAN_POINT('Ctrl Pts',(-0.57173464123408,1.27645855568328,132.5));
#45911=CARTESIAN_POINT('Ctrl Pts',(-0.624982569419363,1.25556235126801,
132.5));
#45912=CARTESIAN_POINT('Ctrl Pts',(-0.676874172622024,1.23144719124002,
132.5));
#45913=CARTESIAN_POINT('Ctrl Pts',(-0.697975522611471,1.22164093357219,
132.5));
#45914=CARTESIAN_POINT('Ctrl Pts',(-0.718852426177283,1.21130177645272,
132.5));
#45915=CARTESIAN_POINT('Ctrl Pts',(-0.739486538730255,1.20044020333604,
132.5));
#45916=CARTESIAN_POINT('Ctrl Pts',(-0.748608547965024,1.19563847658282,
132.5));
#45917=CARTESIAN_POINT('Ctrl Pts',(-0.757684868562274,1.19073364697938,
132.5));
#45918=CARTESIAN_POINT('Ctrl Pts',(-0.766708209897055,1.18572968739322,
132.5));
#45919=CARTESIAN_POINT('Ctrl Pts',(-0.816798485324484,1.15795176072512,
132.5));
#45920=CARTESIAN_POINT('Ctrl Pts',(-0.865077227104213,1.12722452484418,
132.5));
#45921=CARTESIAN_POINT('Ctrl Pts',(-0.911304538955749,1.09377557298447,
132.5));
#45922=CARTESIAN_POINT('Ctrl Pts',(-0.958041120987901,1.05995812568187,
132.5));
#45923=CARTESIAN_POINT('Ctrl Pts',(-1.00268180188713,1.02335824079455,132.5));
#45924=CARTESIAN_POINT('Ctrl Pts',(-1.04496242001946,0.984161078201646,
132.5));
#45925=CARTESIAN_POINT('Ctrl Pts',(-1.06200634880544,0.968360134947809,
132.5));
#45926=CARTESIAN_POINT('Ctrl Pts',(-1.07866649907554,0.95213660337011,132.5));
#45927=CARTESIAN_POINT('Ctrl Pts',(-1.09492426754628,0.935500592349208,
132.5));
#45928=CARTESIAN_POINT('Ctrl Pts',(-1.11554174922657,0.914403437898156,
132.5));
#45929=CARTESIAN_POINT('Ctrl Pts',(-1.13551220287225,0.892642983461476,
132.5));
#45930=CARTESIAN_POINT('Ctrl Pts',(-1.15481600835651,0.870254551841039,
132.5));
#45931=CARTESIAN_POINT('Ctrl Pts',(-1.16444119992803,0.859091315477714,
132.5));
#45932=CARTESIAN_POINT('Ctrl Pts',(-1.17390060984583,0.84777191375158,132.5));
#45933=CARTESIAN_POINT('Ctrl Pts',(-1.18319154863334,0.836300512267484,
132.5));
#45934=CARTESIAN_POINT('Ctrl Pts',(-1.18967862373224,0.828291004873353,
132.5));
#45935=CARTESIAN_POINT('Ctrl Pts',(-1.19608091416041,0.820210558598525,
132.5));
#45936=CARTESIAN_POINT('Ctrl Pts',(-1.20239194526469,0.812068424359708,
132.5));
#45937=CARTESIAN_POINT('Ctrl Pts',(-1.23816283253369,0.765918855268116,
132.5));
#45938=CARTESIAN_POINT('Ctrl Pts',(-1.27106156977561,0.717720815582551,
132.5));
#45939=CARTESIAN_POINT('Ctrl Pts',(-1.30098385596562,0.667789887343701,
132.5));
#45940=CARTESIAN_POINT('Ctrl Pts',(-1.33267614741923,0.614905374434283,
132.5));
#45941=CARTESIAN_POINT('Ctrl Pts',(-1.36103053192321,0.560076290633097,
132.5));
#45942=CARTESIAN_POINT('Ctrl Pts',(-1.38588025440444,0.503631907907152,
132.5));
#45943=CARTESIAN_POINT('Ctrl Pts',(-1.40936682016066,0.450283839031791,
132.5));
#45944=CARTESIAN_POINT('Ctrl Pts',(-1.42972289617106,0.395491656254383,
132.5));
#45945=CARTESIAN_POINT('Ctrl Pts',(-1.44676228694776,0.339508156752185,
132.5));
#45946=CARTESIAN_POINT('Ctrl Pts',(-1.44775125061185,0.336258882906532,
132.5));
#45947=CARTESIAN_POINT('Ctrl Pts',(-1.44872902769048,0.33300559132195,132.5));
#45948=CARTESIAN_POINT('Ctrl Pts',(-1.44969557651745,0.32974832986801,132.5));
#45949=CARTESIAN_POINT('Ctrl Pts',(0.644080091014819,1.33993887967342,131.));
#45950=CARTESIAN_POINT('Ctrl Pts',(0.69545855375229,1.31106406966807,131.));
#45951=CARTESIAN_POINT('Ctrl Pts',(0.74501305727242,1.27920888146368,131.));
#45952=CARTESIAN_POINT('Ctrl Pts',(0.79244836341944,1.2444798284805,131.));
#45953=CARTESIAN_POINT('Ctrl Pts',(0.801096314078014,1.23814836019216,131.));
#45954=CARTESIAN_POINT('Ctrl Pts',(0.809673740649968,1.23172126484837,131.));
#45955=CARTESIAN_POINT('Ctrl Pts',(0.818178728015053,1.22519904766394,131.));
#45956=CARTESIAN_POINT('Ctrl Pts',(0.849870741953171,1.20089540216238,131.));
#45957=CARTESIAN_POINT('Ctrl Pts',(0.880557609427367,1.17527144874649,131.));
#45958=CARTESIAN_POINT('Ctrl Pts',(0.910170030271529,1.14840188938563,131.));
#45959=CARTESIAN_POINT('Ctrl Pts',(0.924142438892699,1.1357236803045,131.));
#45960=CARTESIAN_POINT('Ctrl Pts',(0.937875509062744,1.12276806491419,131.));
#45961=CARTESIAN_POINT('Ctrl Pts',(0.951361230019935,1.10954246813862,131.));
#45962=CARTESIAN_POINT('Ctrl Pts',(0.960549382748327,1.10053154440056,131.));
#45963=CARTESIAN_POINT('Ctrl Pts',(0.969616382834828,1.09140144700476,131.));
#45964=CARTESIAN_POINT('Ctrl Pts',(0.978557707856144,1.08215751935785,131.));
#45965=CARTESIAN_POINT('Ctrl Pts',(1.01915721296604,1.04018399900805,131.));
#45966=CARTESIAN_POINT('Ctrl Pts',(1.05718615879812,0.995849105860942,131.));
#45967=CARTESIAN_POINT('Ctrl Pts',(1.09243705884413,0.949397585827403,131.));
#45968=CARTESIAN_POINT('Ctrl Pts',(1.10966817281199,0.92669145819283,131.));
#45969=CARTESIAN_POINT('Ctrl Pts',(1.12623485703778,0.903479138792705,131.));
#45970=CARTESIAN_POINT('Ctrl Pts',(1.14210882027374,0.879787145895407,131.));
#45971=CARTESIAN_POINT('Ctrl Pts',(1.15509929664831,0.860398775806344,131.));
#45972=CARTESIAN_POINT('Ctrl Pts',(1.16762581229777,0.840689140294072,131.));
#45973=CARTESIAN_POINT('Ctrl Pts',(1.1796713745992,0.820672327962755,131.));
#45974=CARTESIAN_POINT('Ctrl Pts',(1.18580410439404,0.810481213732452,131.));
#45975=CARTESIAN_POINT('Ctrl Pts',(1.19181264491176,0.800209353684452,131.));
#45976=CARTESIAN_POINT('Ctrl Pts',(1.19768623361316,0.789874026042805,131.));
#45977=CARTESIAN_POINT('Ctrl Pts',(1.21764656797304,0.754751274700468,131.));
#45978=CARTESIAN_POINT('Ctrl Pts',(1.2360737454091,0.718856382057069,131.));
#45979=CARTESIAN_POINT('Ctrl Pts',(1.25290111099389,0.682270801499543,131.));
#45980=CARTESIAN_POINT('Ctrl Pts',(1.27683978739331,0.630224010845455,131.));
#45981=CARTESIAN_POINT('Ctrl Pts',(1.29754304910658,0.576779540065319,131.));
#45982=CARTESIAN_POINT('Ctrl Pts',(1.31495193836166,0.522251731680102,131.));
#45983=CARTESIAN_POINT('Ctrl Pts',(1.3278134384389,0.481967173516586,131.));
#45984=CARTESIAN_POINT('Ctrl Pts',(1.3388758149635,0.441090831843476,131.));
#45985=CARTESIAN_POINT('Ctrl Pts',(1.34809711264878,0.399747850113526,131.));
#45986=CARTESIAN_POINT('Ctrl Pts',(1.3522739374108,0.381021376278836,131.));
#45987=CARTESIAN_POINT('Ctrl Pts',(1.35607281945074,0.362199171744182,131.));
#45988=CARTESIAN_POINT('Ctrl Pts',(1.35948878751085,0.343293002470523,131.));
#45989=CARTESIAN_POINT('Ctrl Pts',(1.36178540468056,0.330582042589365,131.));
#45990=CARTESIAN_POINT('Ctrl Pts',(1.36390892640178,0.31783313200029,131.));
#45991=CARTESIAN_POINT('Ctrl Pts',(1.36585766900664,0.305049889819707,131.));
#45992=CARTESIAN_POINT('Ctrl Pts',(1.36749890793905,0.294283791363784,131.));
#45993=CARTESIAN_POINT('Ctrl Pts',(1.36901622844932,0.283492059509838,131.));
#45994=CARTESIAN_POINT('Ctrl Pts',(1.37040659854361,0.272694555744875,131.));
#45995=CARTESIAN_POINT('Ctrl Pts',(1.37758020654124,0.216984885578319,131.));
#45996=CARTESIAN_POINT('Ctrl Pts',(1.38139594905319,0.161015108050636,131.));
#45997=CARTESIAN_POINT('Ctrl Pts',(1.38179530614646,0.105081015157366,131.));
#45998=CARTESIAN_POINT('Ctrl Pts',(1.38199532044291,0.077066943476098,131.));
#45999=CARTESIAN_POINT('Ctrl Pts',(1.38133755560142,0.0490617639963321,
131.));
#46000=CARTESIAN_POINT('Ctrl Pts',(1.37980973540542,0.0211029507209763,
131.));
#46001=CARTESIAN_POINT('Ctrl Pts',(1.37682437540304,-0.0335285583302587,
131.));
#46002=CARTESIAN_POINT('Ctrl Pts',(1.37051962444526,-0.0879843276874055,
131.));
#46003=CARTESIAN_POINT('Ctrl Pts',(1.36095581982918,-0.141970240438976,
131.));
#46004=CARTESIAN_POINT('Ctrl Pts',(1.35717999267375,-0.16328408817649,131.));
#46005=CARTESIAN_POINT('Ctrl Pts',(1.35289570340238,-0.184524487242908,
131.));
#46006=CARTESIAN_POINT('Ctrl Pts',(1.34810488396129,-0.205672316005588,
131.));
#46007=CARTESIAN_POINT('Ctrl Pts',(1.34573474475713,-0.216134680252416,
131.));
#46008=CARTESIAN_POINT('Ctrl Pts',(1.34324061587303,-0.226574376939408,
131.));
#46009=CARTESIAN_POINT('Ctrl Pts',(1.34062264574658,-0.236989022514862,
131.));
#46010=CARTESIAN_POINT('Ctrl Pts',(1.33809205801851,-0.247056048879768,
131.));
#46011=CARTESIAN_POINT('Ctrl Pts',(1.33544770532017,-0.257091762818921,
131.));
#46012=CARTESIAN_POINT('Ctrl Pts',(1.33269167226224,-0.267089239813752,
131.));
#46013=CARTESIAN_POINT('Ctrl Pts',(1.31803859533809,-0.320243101314323,
131.));
#46014=CARTESIAN_POINT('Ctrl Pts',(1.30022114977825,-0.37236300147042,131.));
#46015=CARTESIAN_POINT('Ctrl Pts',(1.27933280126981,-0.423158242313197,
131.));
#46016=CARTESIAN_POINT('Ctrl Pts',(1.2587042121418,-0.473321813290589,131.));
#46017=CARTESIAN_POINT('Ctrl Pts',(1.23508013373137,-0.522194372177886,
131.));
#46018=CARTESIAN_POINT('Ctrl Pts',(1.20850705635476,-0.569470695394981,
131.));
#46019=CARTESIAN_POINT('Ctrl Pts',(1.20244994149213,-0.580246945204162,
131.));
#46020=CARTESIAN_POINT('Ctrl Pts',(1.19623944020916,-0.590940122396141,
131.));
#46021=CARTESIAN_POINT('Ctrl Pts',(1.18987582062145,-0.601546350856353,
131.));
#46022=CARTESIAN_POINT('Ctrl Pts',(1.17627259476364,-0.624218812535633,
131.));
#46023=CARTESIAN_POINT('Ctrl Pts',(1.16196977799215,-0.646494107742248,
131.));
#46024=CARTESIAN_POINT('Ctrl Pts',(1.14698856130615,-0.668343080492641,
131.));
#46025=CARTESIAN_POINT('Ctrl Pts',(1.13947209480414,-0.679305279039234,
131.));
#46026=CARTESIAN_POINT('Ctrl Pts',(1.13178483051549,-0.690160123296984,
131.));
#46027=CARTESIAN_POINT('Ctrl Pts',(1.12392930861312,-0.700903697400656,
131.));
#46028=CARTESIAN_POINT('Ctrl Pts',(1.11818104819913,-0.708765283491613,
131.));
#46029=CARTESIAN_POINT('Ctrl Pts',(1.11234308420749,-0.716566584269759,
131.));
#46030=CARTESIAN_POINT('Ctrl Pts',(1.10642468674068,-0.724295734963858,
131.));
#46031=CARTESIAN_POINT('Ctrl Pts',(1.07360868842271,-0.767151896213436,
131.));
#46032=CARTESIAN_POINT('Ctrl Pts',(1.03826013572302,-0.807879761409639,
131.));
#46033=CARTESIAN_POINT('Ctrl Pts',(1.00060431004052,-0.846274730734576,
131.));
#46034=CARTESIAN_POINT('Ctrl Pts',(0.962725613573854,-0.884896945559157,
131.));
#46035=CARTESIAN_POINT('Ctrl Pts',(0.92251141476043,-0.921159328591376,
131.));
#46036=CARTESIAN_POINT('Ctrl Pts',(0.88015838080179,-0.954811648572381,
131.));
#46037=CARTESIAN_POINT('Ctrl Pts',(0.83780534684315,-0.988463968553386,
131.));
#46038=CARTESIAN_POINT('Ctrl Pts',(0.793312631206348,-1.01950695396809,
131.));
#46039=CARTESIAN_POINT('Ctrl Pts',(0.746857044345091,-1.04763739686597,
131.));
#46040=CARTESIAN_POINT('Origin',(0.,0.,131.75));
#46041=CARTESIAN_POINT('Origin',(0.,0.,132.5));
#46042=CARTESIAN_POINT('Origin',(2.55,0.,111.5));
#46043=CARTESIAN_POINT('',(-2.55,-3.12284933782575E-16,111.5));
#46044=CARTESIAN_POINT('Origin',(0.,0.,111.5));
#46045=CARTESIAN_POINT('Origin',(0.,0.,111.55));
#46046=CARTESIAN_POINT('',(-2.65,-3.24531401774049E-16,111.6));
#46047=CARTESIAN_POINT('Origin',(0.,0.,111.6));
#46048=CARTESIAN_POINT('',(-2.6,-3.18408167778312E-16,111.55));
#46049=CARTESIAN_POINT('Origin',(0.,0.,121.225));
#46050=CARTESIAN_POINT('',(-2.65,-3.24531401774049E-16,130.85));
#46051=CARTESIAN_POINT('Origin',(0.,0.,130.85));
#46052=CARTESIAN_POINT('',(-2.65,-3.24531401774049E-16,121.225));
#46053=CARTESIAN_POINT('Origin',(0.,0.,130.925));
#46054=CARTESIAN_POINT('',(-2.50000000000001,-3.06161699786839E-16,131.));
#46055=CARTESIAN_POINT('Origin',(0.,0.,131.));
#46056=CARTESIAN_POINT('',(-2.575,-3.15346550780443E-16,130.925));
#46057=CARTESIAN_POINT('Origin',(1.5,0.,131.));
#46058=CARTESIAN_POINT('Origin',(2.15,0.,132.5));
#46059=CARTESIAN_POINT('',(-2.14999999999999,-2.6329906181668E-16,132.5));
#46060=CARTESIAN_POINT('Origin',(0.,0.,132.5));
#46061=CARTESIAN_POINT('Origin',(0.,0.,132.55));
#46062=CARTESIAN_POINT('Origin',(0.,0.,132.6));
#46063=CARTESIAN_POINT('',(-2.2,-2.69422295812418E-16,132.55));
#46064=CARTESIAN_POINT('Origin',(0.,0.,133.225));
#46065=CARTESIAN_POINT('Origin',(0.,0.,134.));
#46066=CARTESIAN_POINT('',(0.,0.,0.));
#46067=CARTESIAN_POINT('Origin',(3.,-8.675,108.25));
#46068=CARTESIAN_POINT('',(2.60625649213161,-7.7837163522035,108.250229924968));
#46069=CARTESIAN_POINT('',(2.60668122837429,-7.76538364779651,108.250085965705));
#46070=CARTESIAN_POINT('',(2.6067,-8.675,108.25));
#46071=CARTESIAN_POINT('',(3.17509927743318,-7.7433,108.602463550232));
#46072=CARTESIAN_POINT('Ctrl Pts',(2.60625649213161,-7.7837163522035,108.250229924968));
#46073=CARTESIAN_POINT('Ctrl Pts',(2.60613945209692,-7.78293249916356,108.265681706531));
#46074=CARTESIAN_POINT('Ctrl Pts',(2.6069678498412,-7.78214864612363,108.281121586166));
#46075=CARTESIAN_POINT('Ctrl Pts',(2.60878318617272,-7.78136479308369,108.296444836968));
#46076=CARTESIAN_POINT('Ctrl Pts',(2.62404334187615,-7.77477553508761,108.425255784597));
#46077=CARTESIAN_POINT('Ctrl Pts',(2.70904541124582,-7.76818627709154,108.545825167833));
#46078=CARTESIAN_POINT('Ctrl Pts',(2.82537830757008,-7.76159701909547,108.603239329314));
#46079=CARTESIAN_POINT('Ctrl Pts',(2.93305584509882,-7.75549801273031,108.656381782763));
#46080=CARTESIAN_POINT('Ctrl Pts',(3.06757551455752,-7.74939900636515,108.655417116828));
#46081=CARTESIAN_POINT('Ctrl Pts',(3.17532910733319,-7.7433,108.602640901019));
#46082=CARTESIAN_POINT('',(2.82513055246694,-7.7433,108.602286199445));
#46083=CARTESIAN_POINT('Origin',(3.,-7.7433,108.25));
#46084=CARTESIAN_POINT('Ctrl Pts',(2.82513055246694,-7.7433,108.602286199445));
#46085=CARTESIAN_POINT('Ctrl Pts',(2.76678980321959,-7.74659462899803,108.573326749414));
#46086=CARTESIAN_POINT('Ctrl Pts',(2.71608793488113,-7.74988925799607,108.529614647539));
#46087=CARTESIAN_POINT('Ctrl Pts',(2.67847603852021,-7.75318388699411,108.476364995972));
#46088=CARTESIAN_POINT('Ctrl Pts',(2.64086414215929,-7.75647851599215,108.423115344405));
#46089=CARTESIAN_POINT('Ctrl Pts',(2.61634221777591,-7.75977314499018,108.360328143146));
#46090=CARTESIAN_POINT('Ctrl Pts',(2.60902703442541,-7.76306777398822,108.295710507143));
#46091=CARTESIAN_POINT('Ctrl Pts',(2.60731302843422,-7.76383973192431,108.280570077992));
#46092=CARTESIAN_POINT('Ctrl Pts',(2.6065436766476,-7.76461168986041,108.265329157535));
#46093=CARTESIAN_POINT('Ctrl Pts',(2.60668122837429,-7.76538364779651,108.250085965705));
#46094=CARTESIAN_POINT('Origin',(3.,-8.675,108.25));
#46095=CARTESIAN_POINT('',(2.6072504675668,-7.9087163522035,108.250119138638));
#46096=CARTESIAN_POINT('',(2.60725049571743,-7.8903836477965,108.250120855519));
#46097=CARTESIAN_POINT('',(2.6067,-8.675,108.25));
#46098=CARTESIAN_POINT('Ctrl Pts',(2.6072504675668,-7.9087163522035,108.250119138638));
#46099=CARTESIAN_POINT('Ctrl Pts',(2.60709204657907,-7.90580138047333,108.307959202922));
#46100=CARTESIAN_POINT('Ctrl Pts',(2.6190548870917,-7.90288640874317,108.365736924121));
#46101=CARTESIAN_POINT('Ctrl Pts',(2.64347095486817,-7.89997143701301,108.417658509612));
#46102=CARTESIAN_POINT('Ctrl Pts',(2.69866317788841,-7.89338217901694,108.535026619507));
#46103=CARTESIAN_POINT('Ctrl Pts',(2.81748896429703,-7.88679292102086,108.622471017667));
#46104=CARTESIAN_POINT('Ctrl Pts',(2.94596136011873,-7.88020366302479,108.640259746685));
#46105=CARTESIAN_POINT('Ctrl Pts',(3.07443375594042,-7.87361440502872,108.658048475703));
#46106=CARTESIAN_POINT('Ctrl Pts',(3.21255276117519,-7.86702514703264,108.60618153558));
#46107=CARTESIAN_POINT('Ctrl Pts',(3.29755898965757,-7.86043588903657,108.508227566117));
#46108=CARTESIAN_POINT('Ctrl Pts',(3.38256521813994,-7.85384663104049,108.410273596654));
#46109=CARTESIAN_POINT('Ctrl Pts',(3.41445866986993,-7.84725737304442,108.266232597851));
#46110=CARTESIAN_POINT('Ctrl Pts',(3.37875802532747,-7.84066811504835,108.141544345639));
#46111=CARTESIAN_POINT('Ctrl Pts',(3.34305738078501,-7.83407885705227,108.016856093426));
#46112=CARTESIAN_POINT('Ctrl Pts',(3.2397626399701,-7.8274895990562,107.911520587802));
#46113=CARTESIAN_POINT('Ctrl Pts',(3.1157850441026,-7.82090034106013,107.873410132177));
#46114=CARTESIAN_POINT('Ctrl Pts',(2.99180744823511,-7.81431108306405,107.835299676552));
#46115=CARTESIAN_POINT('Ctrl Pts',(2.84714699731501,-7.80772182506798,107.864414270924));
#46116=CARTESIAN_POINT('Ctrl Pts',(2.74757589287356,-7.8011325670719,107.947497824121));
#46117=CARTESIAN_POINT('Ctrl Pts',(2.65984969008155,-7.79532716211577,108.020697822025));
#46118=CARTESIAN_POINT('Ctrl Pts',(2.60712331889994,-7.78952175715963,108.135790298277));
#46119=CARTESIAN_POINT('Ctrl Pts',(2.60625649213161,-7.7837163522035,108.250229924968));
#46120=CARTESIAN_POINT('Ctrl Pts',(2.60668122837429,-7.76538364779651,108.250085965705));
#46121=CARTESIAN_POINT('Ctrl Pts',(2.60771778701373,-7.77120094785648,108.135216726595));
#46122=CARTESIAN_POINT('Ctrl Pts',(2.66025547383863,-7.77701824791646,108.020218501052));
#46123=CARTESIAN_POINT('Ctrl Pts',(2.74813923550879,-7.78283554797644,107.947123585965));
#46124=CARTESIAN_POINT('Ctrl Pts',(2.84768520586264,-7.78942480597251,107.864328947774));
#46125=CARTESIAN_POINT('Ctrl Pts',(2.99258054913982,-7.79601406396859,107.835296682375));
#46126=CARTESIAN_POINT('Ctrl Pts',(3.11653221376756,-7.80260332196466,107.873581317922));
#46127=CARTESIAN_POINT('Ctrl Pts',(3.2404838783953,-7.80919257996074,107.911865953469));
#46128=CARTESIAN_POINT('Ctrl Pts',(3.34349186437361,-7.81578183795681,108.017467489963));
#46129=CARTESIAN_POINT('Ctrl Pts',(3.37894041067353,-7.82237109595288,108.142241424483));
#46130=CARTESIAN_POINT('Ctrl Pts',(3.41438895697344,-7.82896035394896,108.267015359004));
#46131=CARTESIAN_POINT('Ctrl Pts',(3.38227806359496,-7.83554961194503,108.410961691551));
#46132=CARTESIAN_POINT('Ctrl Pts',(3.2971067528766,-7.8421388699411,108.508752957582));
#46133=CARTESIAN_POINT('Ctrl Pts',(3.21193544215825,-7.84872812793718,108.606544223614));
#46134=CARTESIAN_POINT('Ctrl Pts',(3.07370371410001,-7.85531738593325,108.65818042313));
#46135=CARTESIAN_POINT('Ctrl Pts',(2.94525789024272,-7.86190664392932,108.64016589163));
#46136=CARTESIAN_POINT('Ctrl Pts',(2.81681206638544,-7.8684959019254,108.622151360131));
#46137=CARTESIAN_POINT('Ctrl Pts',(2.69815214672911,-7.87508515992147,108.534486097616));
#46138=CARTESIAN_POINT('Ctrl Pts',(2.64317287905176,-7.88167441791754,108.417017045322));
#46139=CARTESIAN_POINT('Ctrl Pts',(2.61895026900654,-7.88457749454386,108.365262862949));
#46140=CARTESIAN_POINT('Ctrl Pts',(2.60708859829341,-7.88748057117018,108.307723519372));
#46141=CARTESIAN_POINT('Ctrl Pts',(2.60725049571743,-7.8903836477965,108.250120855519));
#46142=CARTESIAN_POINT('Origin',(3.,-8.675,108.25));
#46143=CARTESIAN_POINT('',(2.60665619608725,-8.03371635220349,108.249648010219));
#46144=CARTESIAN_POINT('',(2.60666319360669,-8.0153836477965,108.249647856379));
#46145=CARTESIAN_POINT('',(2.6067,-8.675,108.25));
#46146=CARTESIAN_POINT('Ctrl Pts',(2.60665619608725,-8.03371635220349,108.249648010219));
#46147=CARTESIAN_POINT('Ctrl Pts',(2.60755960895731,-8.02867026178311,108.349392781015));
#46148=CARTESIAN_POINT('Ctrl Pts',(2.64618731517242,-8.02362417136272,108.449760362024));
#46149=CARTESIAN_POINT('Ctrl Pts',(2.7146802163416,-8.01857808094234,108.521689468641));
#46150=CARTESIAN_POINT('Ctrl Pts',(2.80411923924929,-8.01198882294626,108.615615538418));
#46151=CARTESIAN_POINT('Ctrl Pts',(2.94448294371447,-8.00539956495019,108.661049701325));
#46152=CARTESIAN_POINT('Ctrl Pts',(3.07199651953032,-7.99881030695412,108.637348746016));
#46153=CARTESIAN_POINT('Ctrl Pts',(3.19951009534616,-7.99222104895804,108.613647790707));
#46154=CARTESIAN_POINT('Ctrl Pts',(3.31417354251268,-7.98563179096197,108.520811717183));
#46155=CARTESIAN_POINT('Ctrl Pts',(3.36388900806646,-7.97904253296589,108.401021004485));
#46156=CARTESIAN_POINT('Ctrl Pts',(3.41360447362024,-7.97245327496982,108.281230291786));
#46157=CARTESIAN_POINT('Ctrl Pts',(3.39837195756129,-7.96586401697375,108.134484939915));
#46158=CARTESIAN_POINT('Ctrl Pts',(3.32511250731495,-7.95927475897767,108.027459251154));
#46159=CARTESIAN_POINT('Ctrl Pts',(3.25185305706861,-7.9526855009816,107.920433562394));
#46160=CARTESIAN_POINT('Ctrl Pts',(3.12056667263489,-7.94609624298553,107.853127536745));
#46161=CARTESIAN_POINT('Ctrl Pts',(2.99090366781521,-7.93950698498945,107.856122064814));
#46162=CARTESIAN_POINT('Ctrl Pts',(2.86124066299552,-7.93291772699338,107.859116592884));
#46163=CARTESIAN_POINT('Ctrl Pts',(2.73320103778988,-7.9263284689973,107.932411674671));
#46164=CARTESIAN_POINT('Ctrl Pts',(2.66496055500299,-7.91973921100123,108.04270512638));
#46165=CARTESIAN_POINT('Ctrl Pts',(2.62690846039196,-7.91606492473532,108.104206696826));
#46166=CARTESIAN_POINT('Ctrl Pts',(2.60745015528707,-7.91239063846941,108.177212443997));
#46167=CARTESIAN_POINT('Ctrl Pts',(2.6072504675668,-7.9087163522035,108.250119138638));
#46168=CARTESIAN_POINT('Ctrl Pts',(2.60725049571743,-7.8903836477965,108.250120855519));
#46169=CARTESIAN_POINT('Ctrl Pts',(2.60745606496174,-7.89406982916626,108.176979876594));
#46170=CARTESIAN_POINT('Ctrl Pts',(2.62704681118361,-7.89775601053601,108.103736808611));
#46171=CARTESIAN_POINT('Ctrl Pts',(2.66533207709101,-7.90144219190577,108.042105251368));
#46172=CARTESIAN_POINT('Ctrl Pts',(2.73376915850596,-7.90803144990184,107.93193535178));
#46173=CARTESIAN_POINT('Ctrl Pts',(2.86194193703421,-7.91462070789791,107.858868394676));
#46174=CARTESIAN_POINT('Ctrl Pts',(2.99161061635252,-7.92120996589399,107.856106004432));
#46175=CARTESIAN_POINT('Ctrl Pts',(3.12127929567083,-7.92779922389006,107.853343614187));
#46176=CARTESIAN_POINT('Ctrl Pts',(3.2524438757792,-7.93438848188613,107.920885790802));
#46177=CARTESIAN_POINT('Ctrl Pts',(3.32551099973298,-7.94097773988221,108.028042927508));
#46178=CARTESIAN_POINT('Ctrl Pts',(3.39857812368676,-7.94756699787828,108.135200064214));
#46179=CARTESIAN_POINT('Ctrl Pts',(3.41354779148594,-7.95415625587435,108.28197216101));
#46180=CARTESIAN_POINT('Ctrl Pts',(3.3636176372969,-7.96074551387043,108.401673416381));
#46181=CARTESIAN_POINT('Ctrl Pts',(3.31368748310786,-7.9673347718665,108.521374671752));
#46182=CARTESIAN_POINT('Ctrl Pts',(3.1988575069306,-7.97392402986257,108.614005085698));
#46183=CARTESIAN_POINT('Ctrl Pts',(3.07130156624882,-7.98051328785865,108.637477321651));
#46184=CARTESIAN_POINT('Ctrl Pts',(2.94374562556704,-7.98710254585472,108.660949557605));
#46185=CARTESIAN_POINT('Ctrl Pts',(2.80346372038076,-7.9936918038508,108.615263615565));
#46186=CARTESIAN_POINT('Ctrl Pts',(2.71419333797958,-8.00028106184687,108.521177241524));
#46187=CARTESIAN_POINT('Ctrl Pts',(2.64599073591757,-8.00531525716341,108.449295220236));
#46188=CARTESIAN_POINT('Ctrl Pts',(2.60756338177261,-8.01034945247996,108.349162035613));
#46189=CARTESIAN_POINT('Ctrl Pts',(2.60666319360669,-8.0153836477965,108.249647856379));
#46190=CARTESIAN_POINT('Origin',(3.,-8.675,108.25));
#46191=CARTESIAN_POINT('',(2.60614453609637,-8.15871635220349,108.250198273635));
#46192=CARTESIAN_POINT('',(2.60613983983908,-8.1403836477965,108.250194790452));
#46193=CARTESIAN_POINT('',(2.6067,-8.675,108.25));
#46194=CARTESIAN_POINT('Ctrl Pts',(2.60614453609637,-8.15871635220349,108.250198273635));
#46195=CARTESIAN_POINT('Ctrl Pts',(2.60607281260588,-8.15812840108896,108.26178099959));
#46196=CARTESIAN_POINT('Ctrl Pts',(2.60653985332135,-8.15754044997442,108.273357861683));
#46197=CARTESIAN_POINT('Ctrl Pts',(2.60756455998777,-8.15695249885988,108.284885150627));
#46198=CARTESIAN_POINT('Ctrl Pts',(2.61904860420225,-8.15036324086381,108.414073239516));
#46199=CARTESIAN_POINT('Ctrl Pts',(2.70057564494174,-8.14377398286773,108.537034927215));
#46200=CARTESIAN_POINT('Ctrl Pts',(2.81510353413581,-8.13718472487166,108.597902062653));
#46201=CARTESIAN_POINT('Ctrl Pts',(2.92963142332987,-8.13059546687558,108.658769198092));
#46202=CARTESIAN_POINT('Ctrl Pts',(3.0771601609785,-8.12400620887951,108.657541781269));
#46203=CARTESIAN_POINT('Ctrl Pts',(3.19065945543724,-8.11741695088343,108.594777493984));
#46204=CARTESIAN_POINT('Ctrl Pts',(3.30415874989598,-8.11082769288736,108.532013206699));
#46205=CARTESIAN_POINT('Ctrl Pts',(3.38362860116483,-8.10423843489129,108.407712048951));
#46206=CARTESIAN_POINT('Ctrl Pts',(3.39296155340377,-8.09764917689522,108.278350765854));
#46207=CARTESIAN_POINT('Ctrl Pts',(3.4022945056427,-8.09105991889914,108.148989482756));
#46208=CARTESIAN_POINT('Ctrl Pts',(3.34149055885173,-8.08447066090307,108.01456807431));
#46209=CARTESIAN_POINT('Ctrl Pts',(3.23817623846969,-8.077881402907,107.936161462614));
#46210=CARTESIAN_POINT('Ctrl Pts',(3.13486191808765,-8.07129214491093,107.857754850918));
#46211=CARTESIAN_POINT('Ctrl Pts',(2.98903722411454,-8.06470288691485,107.835363035972));
#46212=CARTESIAN_POINT('Ctrl Pts',(2.86695820722666,-8.05811362891878,107.87915983259));
#46213=CARTESIAN_POINT('Ctrl Pts',(2.74487919033878,-8.0515243709227,107.922956629207));
#46214=CARTESIAN_POINT('Ctrl Pts',(2.64654585053613,-8.04493511292663,108.032942037388));
#46215=CARTESIAN_POINT('Ctrl Pts',(2.61663635130991,-8.03834585493055,108.159143729803));
#46216=CARTESIAN_POINT('Ctrl Pts',(2.6096317129366,-8.03680268735487,108.188699464279));
#46217=CARTESIAN_POINT('Ctrl Pts',(2.60637991933983,-8.03525951977918,108.219144613864));
#46218=CARTESIAN_POINT('Ctrl Pts',(2.60665619608725,-8.03371635220349,108.249648010219));
#46219=CARTESIAN_POINT('Ctrl Pts',(2.60666319360669,-8.0153836477965,108.249647856379));
#46220=CARTESIAN_POINT('Ctrl Pts',(2.60638512552761,-8.01693871047603,108.218907931429));
#46221=CARTESIAN_POINT('Ctrl Pts',(2.60968786881117,-8.01849377315556,108.188227071466));
#46222=CARTESIAN_POINT('Ctrl Pts',(2.61679991108365,-8.02004883583509,108.15845622412));
#46223=CARTESIAN_POINT('Ctrl Pts',(2.64693572620495,-8.02663809383116,108.0323083868));
#46224=CARTESIAN_POINT('Ctrl Pts',(2.74546621606361,-8.03322735182724,107.922499518203));
#46225=CARTESIAN_POINT('Ctrl Pts',(2.86762360807162,-8.03981660982331,107.878921763254));
#46226=CARTESIAN_POINT('Ctrl Pts',(2.98978100007963,-8.04640586781938,107.835344008305));
#46227=CARTESIAN_POINT('Ctrl Pts',(3.13556529423699,-8.05299512581546,107.857997367006));
#46228=CARTESIAN_POINT('Ctrl Pts',(3.23873881091994,-8.05958438381153,107.936589177691));
#46229=CARTESIAN_POINT('Ctrl Pts',(3.34191232760289,-8.06617364180761,108.015180988376));
#46230=CARTESIAN_POINT('Ctrl Pts',(3.40247506681144,-8.07276289980368,108.149711251046));
#46231=CARTESIAN_POINT('Ctrl Pts',(3.39291008976981,-8.07935215779975,108.279055591377));
#46232=CARTESIAN_POINT('Ctrl Pts',(3.38334511272818,-8.08594141579582,108.408399931707));
#46233=CARTESIAN_POINT('Ctrl Pts',(3.30365241943638,-8.0925306737919,108.532558349697));
#46234=CARTESIAN_POINT('Ctrl Pts',(3.19004071814446,-8.09911993178797,108.59511895181));
#46235=CARTESIAN_POINT('Ctrl Pts',(3.07642901685254,-8.10570918978405,108.657679553924));
#46236=CARTESIAN_POINT('Ctrl Pts',(2.9288983075605,-8.11229844778012,108.658642340161));
#46237=CARTESIAN_POINT('Ctrl Pts',(2.81447977625942,-8.11888770577619,108.597569866021));
#46238=CARTESIAN_POINT('Ctrl Pts',(2.70006124495835,-8.12547696377227,108.536497391881));
#46239=CARTESIAN_POINT('Ctrl Pts',(2.61875489164825,-8.13206622176834,108.413389657363));
#46240=CARTESIAN_POINT('Ctrl Pts',(2.60750259483268,-8.13865547976441,108.284181169919));
#46241=CARTESIAN_POINT('Ctrl Pts',(2.60651887963764,-8.13923153577511,108.272885311437));
#46242=CARTESIAN_POINT('Ctrl Pts',(2.60607057840048,-8.13980759178581,108.261542825702));
#46243=CARTESIAN_POINT('Ctrl Pts',(2.60613983983908,-8.1403836477965,108.250194790452));
#46244=CARTESIAN_POINT('Origin',(3.,-8.675,108.25));
#46245=CARTESIAN_POINT('',(2.60720600634845,-8.2837163522035,108.250176314706));
#46246=CARTESIAN_POINT('',(2.60720275092572,-8.2653836477965,108.250179618267));
#46247=CARTESIAN_POINT('',(2.6067,-8.675,108.25));
#46248=CARTESIAN_POINT('Ctrl Pts',(2.60720600634845,-8.2837163522035,108.250176314706));
#46249=CARTESIAN_POINT('Ctrl Pts',(2.60698604301128,-8.28099728239873,108.304114064676));
#46250=CARTESIAN_POINT('Ctrl Pts',(2.61733932470525,-8.27827821259397,108.357971006942));
#46251=CARTESIAN_POINT('Ctrl Pts',(2.63867414580283,-8.27555914278921,108.407054689178));
#46252=CARTESIAN_POINT('Ctrl Pts',(2.69037588595888,-8.26896988479313,108.526001633857));
#46253=CARTESIAN_POINT('Ctrl Pts',(2.8065680950138,-8.26238062679706,108.616917009719));
#46254=CARTESIAN_POINT('Ctrl Pts',(2.93445836245162,-8.25579136880098,108.638493039901));
#46255=CARTESIAN_POINT('Ctrl Pts',(3.06234862988944,-8.24920211080491,108.660069070083));
#46256=CARTESIAN_POINT('Ctrl Pts',(3.20193695571016,-8.24261285280884,108.612305754586));
#46257=CARTESIAN_POINT('Ctrl Pts',(3.28980080702969,-8.23602359481276,108.516904553256));
#46258=CARTESIAN_POINT('Ctrl Pts',(3.37766465834923,-8.22943433681669,108.421503351926));
#46259=CARTESIAN_POINT('Ctrl Pts',(3.41380403516758,-8.22284507882062,108.278464264762));
#46260=CARTESIAN_POINT('Ctrl Pts',(3.38179886222579,-8.21625582082454,108.152777692334));
#46261=CARTESIAN_POINT('Ctrl Pts',(3.34979368928399,-8.20966656282847,108.027091119906));
#46262=CARTESIAN_POINT('Ctrl Pts',(3.24964396658204,-8.2030773048324,107.918757062214));
#46263=CARTESIAN_POINT('Ctrl Pts',(3.12685313465012,-8.19648804683632,107.876997546212));
#46264=CARTESIAN_POINT('Ctrl Pts',(3.00406230271819,-8.18989878884025,107.835238030209));
#46265=CARTESIAN_POINT('Ctrl Pts',(2.85863036155628,-8.18330953084418,107.860053055896));
#46266=CARTESIAN_POINT('Ctrl Pts',(2.75663491482005,-8.1767202728481,107.940167813778));
#46267=CARTESIAN_POINT('Ctrl Pts',(2.6637403921366,-8.17071896596657,108.013134033659));
#46268=CARTESIAN_POINT('Ctrl Pts',(2.60687662872517,-8.16471765908503,108.131971619654));
#46269=CARTESIAN_POINT('Ctrl Pts',(2.60614453609637,-8.15871635220349,108.250198273635));
#46270=CARTESIAN_POINT('Ctrl Pts',(2.60613983983908,-8.1403836477965,108.250194790452));
#46271=CARTESIAN_POINT('Ctrl Pts',(2.60686283033371,-8.14639684978188,108.131737510561));
#46272=CARTESIAN_POINT('Ctrl Pts',(2.66398140619207,-8.15241005176726,108.012675534682));
#46273=CARTESIAN_POINT('Ctrl Pts',(2.75719105092667,-8.15842325375264,107.939731761829));
#46274=CARTESIAN_POINT('Ctrl Pts',(2.85933004415725,-8.16501251174871,107.859800081552));
#46275=CARTESIAN_POINT('Ctrl Pts',(3.00480627093945,-8.17160176974478,107.835245961367));
#46276=CARTESIAN_POINT('Ctrl Pts',(3.1275220064063,-8.17819102774086,107.87722566715));
#46277=CARTESIAN_POINT('Ctrl Pts',(3.25023774187315,-8.18478028573693,107.919205372932));
#46278=CARTESIAN_POINT('Ctrl Pts',(3.35019298602466,-8.191369543733,108.027718904682));
#46279=CARTESIAN_POINT('Ctrl Pts',(3.38197266039813,-8.19795880172908,108.153462690723));
#46280=CARTESIAN_POINT('Ctrl Pts',(3.4137523347716,-8.20454805972515,108.279206476764));
#46281=CARTESIAN_POINT('Ctrl Pts',(3.37735643936704,-8.21113731772122,108.422180517097));
#46282=CARTESIAN_POINT('Ctrl Pts',(3.28932159975375,-8.2177265757173,108.517423965421));
#46283=CARTESIAN_POINT('Ctrl Pts',(3.20128676014047,-8.22431583371337,108.612667413746));
#46284=CARTESIAN_POINT('Ctrl Pts',(3.06161297631846,-8.23090509170945,108.660180270062));
#46285=CARTESIAN_POINT('Ctrl Pts',(2.93376160935407,-8.23749434970552,108.638374871702));
#46286=CARTESIAN_POINT('Ctrl Pts',(2.80591024238967,-8.24408360770159,108.616569473341));
#46287=CARTESIAN_POINT('Ctrl Pts',(2.6898812922829,-8.25067286569767,108.525445820303));
#46288=CARTESIAN_POINT('Ctrl Pts',(2.63839299217811,-8.25726212369374,108.406406321039));
#46289=CARTESIAN_POINT('Ctrl Pts',(2.61723919557154,-8.25996929839466,108.35749933925));
#46290=CARTESIAN_POINT('Ctrl Pts',(2.60697953705813,-8.26267647309558,108.303880302597));
#46291=CARTESIAN_POINT('Ctrl Pts',(2.60720275092572,-8.2653836477965,108.250179618267));
#46292=CARTESIAN_POINT('Origin',(3.,-8.675,108.25));
#46293=CARTESIAN_POINT('',(2.60677025899564,-8.40871635220349,108.249651168915));
#46294=CARTESIAN_POINT('',(2.60677702480763,-8.3903836477965,108.249651743722));
#46295=CARTESIAN_POINT('',(2.6067,-8.675,108.25));
#46296=CARTESIAN_POINT('Ctrl Pts',(2.60677025899564,-8.40871635220349,108.249651168915));
#46297=CARTESIAN_POINT('Ctrl Pts',(2.60760908356072,-8.40386616370851,108.345594615925));
#46298=CARTESIAN_POINT('Ctrl Pts',(2.64301678385761,-8.39901597521352,108.442092426262));
#46299=CARTESIAN_POINT('Ctrl Pts',(2.70677980611443,-8.39416578671853,108.513143432754));
#46300=CARTESIAN_POINT('Ctrl Pts',(2.79340551245423,-8.38757652872246,108.609670281791));
#46301=CARTESIAN_POINT('Ctrl Pts',(2.93236599521414,-8.38098727072638,108.659230540508));
#46302=CARTESIAN_POINT('Ctrl Pts',(3.06052398459853,-8.37439801273031,108.639306300479));
#46303=CARTESIAN_POINT('Ctrl Pts',(3.18868197398291,-8.36780875473423,108.619382060449));
#46304=CARTESIAN_POINT('Ctrl Pts',(3.30603746999177,-8.36121949673816,108.529973321673));
#46305=CARTESIAN_POINT('Ctrl Pts',(3.35926951787344,-8.35463023874209,108.411703314224));
#46306=CARTESIAN_POINT('Ctrl Pts',(3.41250156575511,-8.34804098074602,108.293433306774));
#46307=CARTESIAN_POINT('Ctrl Pts',(3.40161016550959,-8.34145172274994,108.146302030651));
#46308=CARTESIAN_POINT('Ctrl Pts',(3.33154386986275,-8.33486246475387,108.037159189392));
#46309=CARTESIAN_POINT('Ctrl Pts',(3.26147757421591,-8.3282732067578,107.928016348133));
#46310=CARTESIAN_POINT('Ctrl Pts',(3.13223638316774,-8.32168394876172,107.856861941737));
#46311=CARTESIAN_POINT('Ctrl Pts',(3.0025415661458,-8.31509469076565,107.8560252689));
#46312=CARTESIAN_POINT('Ctrl Pts',(2.87284674912387,-8.30850543276957,107.855188596062));
#46313=CARTESIAN_POINT('Ctrl Pts',(2.74269830612817,-8.3019161747735,107.924669656782));
#46314=CARTESIAN_POINT('Ctrl Pts',(2.6712297202589,-8.29532691677743,108.032899443891));
#46315=CARTESIAN_POINT('Ctrl Pts',(2.62925278184706,-8.29145672858612,108.096468004155));
#46316=CARTESIAN_POINT('Ctrl Pts',(2.60751909117935,-8.28758654039481,108.173404014622));
#46317=CARTESIAN_POINT('Ctrl Pts',(2.60720600634845,-8.2837163522035,108.250176314706));
#46318=CARTESIAN_POINT('Ctrl Pts',(2.60720275092572,-8.2653836477965,108.250179618267));
#46319=CARTESIAN_POINT('Ctrl Pts',(2.60752283918096,-8.26926573109165,108.173172940604));
#46320=CARTESIAN_POINT('Ctrl Pts',(2.62939938691649,-8.27314781438681,108.095998366703));
#46321=CARTESIAN_POINT('Ctrl Pts',(2.67161965273307,-8.27702989768196,108.032310053299));
#46322=CARTESIAN_POINT('Ctrl Pts',(2.74328226349561,-8.28361915567803,107.924208630312));
#46323=CARTESIAN_POINT('Ctrl Pts',(2.87355513512348,-8.29020841367411,107.85496112983));
#46324=CARTESIAN_POINT('Ctrl Pts',(3.00324824985443,-8.29679767167018,107.856030439959));
#46325=CARTESIAN_POINT('Ctrl Pts',(3.13294136458537,-8.30338692966625,107.857099750088));
#46326=CARTESIAN_POINT('Ctrl Pts',(3.26205472241938,-8.30997618766233,107.928485870829));
#46327=CARTESIAN_POINT('Ctrl Pts',(3.3319251354776,-8.3165654456584,108.037754223118));
#46328=CARTESIAN_POINT('Ctrl Pts',(3.40179554853582,-8.32315470365447,108.147022575406));
#46329=CARTESIAN_POINT('Ctrl Pts',(3.41242301681823,-8.32974396165055,108.294173159243));
#46330=CARTESIAN_POINT('Ctrl Pts',(3.35897890617778,-8.33633321964662,108.41234749855));
#46331=CARTESIAN_POINT('Ctrl Pts',(3.30553479553734,-8.3429224776427,108.530521837857));
#46332=CARTESIAN_POINT('Ctrl Pts',(3.18801910597402,-8.34951173563877,108.619719932635));
#46333=CARTESIAN_POINT('Ctrl Pts',(3.05982557684307,-8.35610099363485,108.639414259782));
#46334=CARTESIAN_POINT('Ctrl Pts',(2.93163204771212,-8.36269025163092,108.659108586929));
#46335=CARTESIAN_POINT('Ctrl Pts',(2.79276067901352,-8.36927950962699,108.609299146445));
#46336=CARTESIAN_POINT('Ctrl Pts',(2.70630825120084,-8.37586876762306,108.512617063523));
#46337=CARTESIAN_POINT('Ctrl Pts',(2.64282884116956,-8.38070706101421,108.441626326308));
#46338=CARTESIAN_POINT('Ctrl Pts',(2.6076112180575,-8.38554535440536,108.345364101143));
#46339=CARTESIAN_POINT('Ctrl Pts',(2.60677702480763,-8.3903836477965,108.249651743722));
#46340=CARTESIAN_POINT('Origin',(3.,-8.675,108.25));
#46341=CARTESIAN_POINT('',(2.60607704946663,-8.53371635220349,108.250137347263));
#46342=CARTESIAN_POINT('',(2.60607363302738,-8.5153836477965,108.250133427664));
#46343=CARTESIAN_POINT('',(2.6067,-8.675,108.25));
#46344=CARTESIAN_POINT('Ctrl Pts',(2.60607704946663,-8.53371635220349,108.250137347263));
#46345=CARTESIAN_POINT('Ctrl Pts',(2.6060419851575,-8.53332430301436,108.257857266924));
#46346=CARTESIAN_POINT('Ctrl Pts',(2.60624943432723,-8.53293225382521,108.265575266175));
#46347=CARTESIAN_POINT('Ctrl Pts',(2.60670538132437,-8.53254020463607,108.273278557188));
#46348=CARTESIAN_POINT('Ctrl Pts',(2.61436858400385,-8.52595094664,108.402749484073));
#46349=CARTESIAN_POINT('Ctrl Pts',(2.69222813183566,-8.51936168864393,108.528065587685));
#46350=CARTESIAN_POINT('Ctrl Pts',(2.80490821739606,-8.51277243064786,108.592288978298));
#46351=CARTESIAN_POINT('Ctrl Pts',(2.91758830295647,-8.50618317265178,108.656512368912));
#46352=CARTESIAN_POINT('Ctrl Pts',(3.06508892624547,-8.49959391465571,108.659643046527));
#46353=CARTESIAN_POINT('Ctrl Pts',(3.18039256931364,-8.49300465665963,108.600258574828));
#46354=CARTESIAN_POINT('Ctrl Pts',(3.29569621238182,-8.48641539866356,108.540874103128));
#46355=CARTESIAN_POINT('Ctrl Pts',(3.37880287522917,-8.47982614066749,108.418974482114));
#46356=CARTESIAN_POINT('Ctrl Pts',(3.39195270203343,-8.47323688267141,108.289945308519));
#46357=CARTESIAN_POINT('Ctrl Pts',(3.40510252883768,-8.46664762467534,108.160916134923));
#46358=CARTESIAN_POINT('Ctrl Pts',(3.34829551959883,-8.46005836667926,108.024757408745));
#46359=CARTESIAN_POINT('Ctrl Pts',(3.24734217380106,-8.45346910868319,107.943333410096));
#46360=CARTESIAN_POINT('Ctrl Pts',(3.14638882800329,-8.44687985068712,107.861909411447));
#46361=CARTESIAN_POINT('Ctrl Pts',(3.0012891456466,-8.44029059269105,107.835220140326));
#46362=CARTESIAN_POINT('Ctrl Pts',(2.87796976724249,-8.43370133469497,107.875391977399));
#46363=CARTESIAN_POINT('Ctrl Pts',(2.75465038883837,-8.4271120766989,107.915563814472));
#46364=CARTESIAN_POINT('Ctrl Pts',(2.65311131438682,-8.42052281870282,108.022596759739));
#46365=CARTESIAN_POINT('Ctrl Pts',(2.61948724212089,-8.41393356070675,108.14785995205));
#46366=CARTESIAN_POINT('Ctrl Pts',(2.61061301096849,-8.41219449120566,108.180920032182));
#46367=CARTESIAN_POINT('Ctrl Pts',(2.60646949249566,-8.41045542170458,108.215249965189));
#46368=CARTESIAN_POINT('Ctrl Pts',(2.60677025899564,-8.40871635220349,108.249651168915));
#46369=CARTESIAN_POINT('Ctrl Pts',(2.60677702480763,-8.3903836477965,108.249651743722));
#46370=CARTESIAN_POINT('Ctrl Pts',(2.60647513264523,-8.39213461240143,108.215013714039));
#46371=CARTESIAN_POINT('Ctrl Pts',(2.61067642280362,-8.39388557700636,108.180447700287));
#46372=CARTESIAN_POINT('Ctrl Pts',(2.61967104589793,-8.39563654161128,108.147177570357));
#46373=CARTESIAN_POINT('Ctrl Pts',(2.65351975533446,-8.40222579960736,108.021974885472));
#46374=CARTESIAN_POINT('Ctrl Pts',(2.75525066113429,-8.40881505760343,107.915124241063));
#46375=CARTESIAN_POINT('Ctrl Pts',(2.87864190569828,-8.4154043155995,107.87517366913));
#46376=CARTESIAN_POINT('Ctrl Pts',(3.00203315026227,-8.42199357359558,107.835223097197));
#46377=CARTESIAN_POINT('Ctrl Pts',(3.14708473359041,-8.42858283159165,107.86217259774));
#46378=CARTESIAN_POINT('Ctrl Pts',(3.24789186916368,-8.43517208958773,107.94377755378));
#46379=CARTESIAN_POINT('Ctrl Pts',(3.34869900473694,-8.4417613475838,108.025382509821));
#46380=CARTESIAN_POINT('Ctrl Pts',(3.40526169255533,-8.44835060557987,108.161642921358));
#46381=CARTESIAN_POINT('Ctrl Pts',(3.39188044158204,-8.45493986357595,108.290648307118));
#46382=CARTESIAN_POINT('Ctrl Pts',(3.37849919060876,-8.46152912157202,108.419653692879));
#46383=CARTESIAN_POINT('Ctrl Pts',(3.29517400084382,-8.4681183795681,108.541404052863));
#46384=CARTESIAN_POINT('Ctrl Pts',(3.17976401671787,-8.47470763756417,108.600581607703));
#46385=CARTESIAN_POINT('Ctrl Pts',(3.06435403259193,-8.48129689556024,108.659759162543));
#46386=CARTESIAN_POINT('Ctrl Pts',(2.91685925410498,-8.48788615355631,108.65636391224));
#46387=CARTESIAN_POINT('Ctrl Pts',(2.80429454359648,-8.49447541155238,108.591938502804));
#46388=CARTESIAN_POINT('Ctrl Pts',(2.69172983308797,-8.50106466954846,108.527513093369));
#46389=CARTESIAN_POINT('Ctrl Pts',(2.6140951905579,-8.50765392754453,108.4020575248));
#46390=CARTESIAN_POINT('Ctrl Pts',(2.60666423677642,-8.51424318554061,108.272573053304));
#46391=CARTESIAN_POINT('Ctrl Pts',(2.60623552273314,-8.51462333962591,108.265102705224));
#46392=CARTESIAN_POINT('Ctrl Pts',(2.60604048045085,-8.51500349371121,108.25761894701));
#46393=CARTESIAN_POINT('Ctrl Pts',(2.60607363302738,-8.5153836477965,108.250133427664));
#46394=CARTESIAN_POINT('Origin',(3.,-8.675,108.25));
#46395=CARTESIAN_POINT('',(2.60714512931118,-8.6587163522035,108.250227864382));
#46396=CARTESIAN_POINT('',(2.60714090487912,-8.6403836477965,108.250230780684));
#46397=CARTESIAN_POINT('',(2.6067,-8.675,108.25));
#46398=CARTESIAN_POINT('Ctrl Pts',(2.60714512931118,-8.6587163522035,108.250227864382));
#46399=CARTESIAN_POINT('Ctrl Pts',(2.60687884329338,-8.65619318432413,108.300260095951));
#46400=CARTESIAN_POINT('Ctrl Pts',(2.61574913749029,-8.65367001644477,108.350201453516));
#46401=CARTESIAN_POINT('Ctrl Pts',(2.63419286977669,-8.6511468485654,108.39631367599));
#46402=CARTESIAN_POINT('Ctrl Pts',(2.68235871376967,-8.64455759056933,108.516735837805));
#46403=CARTESIAN_POINT('Ctrl Pts',(2.79581485758624,-8.63796833257325,108.611043517467));
#46404=CARTESIAN_POINT('Ctrl Pts',(2.92301203326297,-8.63137907457718,108.63638763086));
#46405=CARTESIAN_POINT('Ctrl Pts',(3.05020920893969,-8.6247898165811,108.661731744253));
#46406=CARTESIAN_POINT('Ctrl Pts',(3.19114741647657,-8.61820055858503,108.618112291376));
#46407=CARTESIAN_POINT('Ctrl Pts',(3.28179079864977,-8.61161130058896,108.525347950964));
#46408=CARTESIAN_POINT('Ctrl Pts',(3.37243418082296,-8.60502204259289,108.432583610553));
#46409=CARTESIAN_POINT('Ctrl Pts',(3.41278273763247,-8.59843278459681,108.290674382606));
#46410=CARTESIAN_POINT('Ctrl Pts',(3.38450393549355,-8.59184352660074,108.164097311486));
#46411=CARTESIAN_POINT('Ctrl Pts',(3.35622513335464,-8.58525426860466,108.037520240366));
#46412=CARTESIAN_POINT('Ctrl Pts',(3.25931897226731,-8.57866501060859,107.926275326072));
#46413=CARTESIAN_POINT('Ctrl Pts',(3.13781516712542,-8.57207575261252,107.880907155293));
#46414=CARTESIAN_POINT('Ctrl Pts',(3.01631136198352,-8.56548649461644,107.835538984514));
#46415=CARTESIAN_POINT('Ctrl Pts',(2.87020991278705,-8.55889723662037,107.85604755725));
#46416=CARTESIAN_POINT('Ctrl Pts',(2.76589261695239,-8.5523079786243,107.933114718697));
#46417=CARTESIAN_POINT('Ctrl Pts',(2.66778201559982,-8.54611076981736,108.005596520431));
#46418=CARTESIAN_POINT('Ctrl Pts',(2.60663131880675,-8.53991356101043,108.128106858646));
#46419=CARTESIAN_POINT('Ctrl Pts',(2.60607704946663,-8.53371635220349,108.250137347263));
#46420=CARTESIAN_POINT('Ctrl Pts',(2.60607363302738,-8.5153836477965,108.250133427664));
#46421=CARTESIAN_POINT('Ctrl Pts',(2.60661511817905,-8.52159275170728,108.127871510083));
#46422=CARTESIAN_POINT('Ctrl Pts',(2.66803236211992,-8.52780185561805,108.005139773665));
#46423=CARTESIAN_POINT('Ctrl Pts',(2.76646139004698,-8.53401095952883,107.932695283635));
#46424=CARTESIAN_POINT('Ctrl Pts',(2.87091676213192,-8.54060021752491,107.855815359888));
#46425=CARTESIAN_POINT('Ctrl Pts',(3.01705477133471,-8.54718947552098,107.835568886818));
#46426=CARTESIAN_POINT('Ctrl Pts',(3.13847700904895,-8.55377873351705,107.881154933162));
#46427=CARTESIAN_POINT('Ctrl Pts',(3.25989924676319,-8.56036799151313,107.926740979506));
#46428=CARTESIAN_POINT('Ctrl Pts',(3.35660571298888,-8.5669572495092,108.038159545264));
#46429=CARTESIAN_POINT('Ctrl Pts',(3.38465742501809,-8.57354650750527,108.164787144488));
#46430=CARTESIAN_POINT('Ctrl Pts',(3.4127091370473,-8.58013576550134,108.291414743711));
#46431=CARTESIAN_POINT('Ctrl Pts',(3.37210609488002,-8.58672502349742,108.433251376399));
#46432=CARTESIAN_POINT('Ctrl Pts',(3.28129645857532,-8.59331428149349,108.525852982146));
#46433=CARTESIAN_POINT('Ctrl Pts',(3.19048682227062,-8.59990353948957,108.618454587894));
#46434=CARTESIAN_POINT('Ctrl Pts',(3.0494705918285,-8.60649279748564,108.661821166701));
#46435=CARTESIAN_POINT('Ctrl Pts',(2.92231907450233,-8.61308205548171,108.636248934212));
#46436=CARTESIAN_POINT('Ctrl Pts',(2.79516755717617,-8.61967131347779,108.610676701723));
#46437=CARTESIAN_POINT('Ctrl Pts',(2.68188075296595,-8.62626057147386,108.516165657938));
#46438=CARTESIAN_POINT('Ctrl Pts',(2.63393098968494,-8.63284982946993,108.395657286303));
#46439=CARTESIAN_POINT('Ctrl Pts',(2.61565655951509,-8.63536110224546,108.349729597162));
#46440=CARTESIAN_POINT('Ctrl Pts',(2.60687230419797,-8.63787237502098,108.300025808225));
#46441=CARTESIAN_POINT('Ctrl Pts',(2.60714090487912,-8.6403836477965,108.250230780684));
#46442=CARTESIAN_POINT('Origin',(3.,-8.675,108.25));
#46443=CARTESIAN_POINT('',(2.60687901882508,-8.78371635220349,108.249666035988));
#46444=CARTESIAN_POINT('',(2.60688536129284,-8.7653836477965,108.249667300834));
#46445=CARTESIAN_POINT('',(2.6067,-8.675,108.25));
#46446=CARTESIAN_POINT('Ctrl Pts',(2.60687901882508,-8.78371635220349,108.249666035988));
#46447=CARTESIAN_POINT('Ctrl Pts',(2.6076329537605,-8.7790620656339,108.341799007699));
#46448=CARTESIAN_POINT('Ctrl Pts',(2.63998823948557,-8.77440777906431,108.434409003843));
#46449=CARTESIAN_POINT('Ctrl Pts',(2.69913526959871,-8.76975349249472,108.504367769783));
#46450=CARTESIAN_POINT('Ctrl Pts',(2.78287206476371,-8.76316423449865,108.603411167944));
#46451=CARTESIAN_POINT('Ctrl Pts',(2.92030805502711,-8.75657497650258,108.65705428114));
#46452=CARTESIAN_POINT('Ctrl Pts',(3.0489986300612,-8.7499857185065,108.640924139132));
#46453=CARTESIAN_POINT('Ctrl Pts',(3.1776892050953,-8.74339646051043,108.624793997124));
#46454=CARTESIAN_POINT('Ctrl Pts',(3.2976343649001,-8.73680720251436,108.538890599913));
#46455=CARTESIAN_POINT('Ctrl Pts',(3.35433653027273,-8.73021794451828,108.422244511141));
#46456=CARTESIAN_POINT('Ctrl Pts',(3.41103869564537,-8.72362868652221,108.305598422369));
#46457=CARTESIAN_POINT('Ctrl Pts',(3.40449786658584,-8.71703942852613,108.158209642035));
#46458=CARTESIAN_POINT('Ctrl Pts',(3.33768589581671,-8.71045017053006,108.047044871781));
#46459=CARTESIAN_POINT('Ctrl Pts',(3.27087392504758,-8.70386091253399,107.935880101526));
#46460=CARTESIAN_POINT('Ctrl Pts',(3.14379081256885,-8.69727165453792,107.860939341351));
#46461=CARTESIAN_POINT('Ctrl Pts',(3.01417729588862,-8.69068239654184,107.85627223544));
#46462=CARTESIAN_POINT('Ctrl Pts',(2.8845637792084,-8.68409313854577,107.85160512953));
#46463=CARTESIAN_POINT('Ctrl Pts',(2.75241985832666,-8.6775038805497,107.917211677884));
#46464=CARTESIAN_POINT('Ctrl Pts',(2.67778566997049,-8.67091462255362,108.023283274045));
#46465=CARTESIAN_POINT('Ctrl Pts',(2.63173050930985,-8.66684853243691,108.088737786385));
#46466=CARTESIAN_POINT('Ctrl Pts',(2.6075742497649,-8.66278244232021,108.169600822494));
#46467=CARTESIAN_POINT('Ctrl Pts',(2.60714512931118,-8.6587163522035,108.250227864382));
#46468=CARTESIAN_POINT('Ctrl Pts',(2.60714090487912,-8.6403836477965,108.250230780684));
#46469=CARTESIAN_POINT('Ctrl Pts',(2.60757707796976,-8.64446163301706,108.169370036145));
#46470=CARTESIAN_POINT('Ctrl Pts',(2.63188526888634,-8.64853961823761,108.088268699072));
#46471=CARTESIAN_POINT('Ctrl Pts',(2.67819284115219,-8.65261760345816,108.022705658054));
#46472=CARTESIAN_POINT('Ctrl Pts',(2.75301717825226,-8.65920686145423,107.916768100926));
#46473=CARTESIAN_POINT('Ctrl Pts',(2.88527857480418,-8.6657961194503,107.851398686154));
#46474=CARTESIAN_POINT('Ctrl Pts',(3.01488351852452,-8.67238537744638,107.856298277572));
#46475=CARTESIAN_POINT('Ctrl Pts',(3.14448846224486,-8.67897463544245,107.861197868991));
#46476=CARTESIAN_POINT('Ctrl Pts',(3.27143695313361,-8.68556389343853,107.936366466601));
#46477=CARTESIAN_POINT('Ctrl Pts',(3.33804941955861,-8.6921531514346,108.047650907335));
#46478=CARTESIAN_POINT('Ctrl Pts',(3.4046618859836,-8.69874240943067,108.15893534807));
#46479=CARTESIAN_POINT('Ctrl Pts',(3.41093832794482,-8.70533166742674,108.306335631929));
#46480=CARTESIAN_POINT('Ctrl Pts',(3.3540270180908,-8.71192092542282,108.422879830599));
#46481=CARTESIAN_POINT('Ctrl Pts',(3.29711570823677,-8.71851018341889,108.539424029268));
#46482=CARTESIAN_POINT('Ctrl Pts',(3.17701664656749,-8.72509944141497,108.625112142748));
#46483=CARTESIAN_POINT('Ctrl Pts',(3.04829733823417,-8.73168869941104,108.641011422449));
#46484=CARTESIAN_POINT('Ctrl Pts',(2.91957802990085,-8.73827795740711,108.65691070215));
#46485=CARTESIAN_POINT('Ctrl Pts',(2.78223847490348,-8.74486721540318,108.603021148073));
#46486=CARTESIAN_POINT('Ctrl Pts',(2.69867946780799,-8.75145647339926,108.503827701888));
#46487=CARTESIAN_POINT('Ctrl Pts',(2.63980886027409,-8.75609886486501,108.43394201699));
#46488=CARTESIAN_POINT('Ctrl Pts',(2.6076336087024,-8.76074125633075,108.341568581902));
#46489=CARTESIAN_POINT('Ctrl Pts',(2.60688536129284,-8.7653836477965,108.249667300834));
#46490=CARTESIAN_POINT('Origin',(3.,-8.675,108.25));
#46491=CARTESIAN_POINT('',(2.60603291882732,-8.9087163522035,108.250070364255));
#46492=CARTESIAN_POINT('',(2.60603107819738,-8.8903836477965,108.250066160239));
#46493=CARTESIAN_POINT('',(2.6067,-8.675,108.25));
#46494=CARTESIAN_POINT('Ctrl Pts',(2.60603291882732,-8.9087163522035,108.250070364255));
#46495=CARTESIAN_POINT('Ctrl Pts',(2.60602332688793,-8.90852020493976,108.253931583289));
#46496=CARTESIAN_POINT('Ctrl Pts',(2.60607522236371,-8.90832405767601,108.257792538181));
#46497=CARTESIAN_POINT('Ctrl Pts',(2.60618940167944,-8.90812791041227,108.261651650285));
#46498=CARTESIAN_POINT('Ctrl Pts',(2.61002507572765,-8.9015386524162,108.391292435489));
#46499=CARTESIAN_POINT('Ctrl Pts',(2.6841491884467,-8.89494939442012,108.518853600922));
#46500=CARTESIAN_POINT('Ctrl Pts',(2.79488314279838,-8.88836013642405,108.58637720374));
#46501=CARTESIAN_POINT('Ctrl Pts',(2.90561709715007,-8.88177087842798,108.653900806557));
#46502=CARTESIAN_POINT('Ctrl Pts',(3.0529608931344,-8.8751816204319,108.661386846759));
#46503=CARTESIAN_POINT('Ctrl Pts',(3.16996826793614,-8.86859236243583,108.605434011033));
#46504=CARTESIAN_POINT('Ctrl Pts',(3.28697564273788,-8.86200310443976,108.549481175306));
#46505=CARTESIAN_POINT('Ctrl Pts',(3.37364659635704,-8.85541384644368,108.430089463652));
#46506=CARTESIAN_POINT('Ctrl Pts',(3.39060182272462,-8.84882458844761,108.301504993818));
#46507=CARTESIAN_POINT('Ctrl Pts',(3.40755704909219,-8.84223533045154,108.172920523983));
#46508=CARTESIAN_POINT('Ctrl Pts',(3.35479654820819,-8.83564607245546,108.035143295968));
#46509=CARTESIAN_POINT('Ctrl Pts',(3.25629227175775,-8.82905681445939,107.950772962884));
#46510=CARTESIAN_POINT('Ctrl Pts',(3.15778799530732,-8.82246755646331,107.8664026298));
#46511=CARTESIAN_POINT('Ctrl Pts',(3.01353994329047,-8.81587829846724,107.835439191646));
#46512=CARTESIAN_POINT('Ctrl Pts',(2.88908781445318,-8.80928904047117,107.871951014548));
#46513=CARTESIAN_POINT('Ctrl Pts',(2.7646356856159,-8.80269978247509,107.908462837451));
#46514=CARTESIAN_POINT('Ctrl Pts',(2.65997947995819,-8.79611052447902,108.01244992141));
#46515=CARTESIAN_POINT('Ctrl Pts',(2.62267017716264,-8.78952126648294,108.136665304953));
#46516=CARTESIAN_POINT('Ctrl Pts',(2.61171409760188,-8.78758629505646,108.173141827503));
#46517=CARTESIAN_POINT('Ctrl Pts',(2.60656557818587,-8.78565132362998,108.211362707425));
#46518=CARTESIAN_POINT('Ctrl Pts',(2.60687901882508,-8.78371635220349,108.249666035988));
#46519=CARTESIAN_POINT('Ctrl Pts',(2.60688536129284,-8.7653836477965,108.249667300834));
#46520=CARTESIAN_POINT('Ctrl Pts',(2.60657157090079,-8.76733051432683,108.21112692148));
#46521=CARTESIAN_POINT('Ctrl Pts',(2.61178481051869,-8.76927738085715,108.172669579293));
#46522=CARTESIAN_POINT('Ctrl Pts',(2.62287405626398,-8.77122424738748,108.135988650006));
#46523=CARTESIAN_POINT('Ctrl Pts',(2.66040611100908,-8.77781350538355,108.011840382602));
#46524=CARTESIAN_POINT('Ctrl Pts',(2.7652486796929,-8.78440276337963,107.908041186087));
#46525=CARTESIAN_POINT('Ctrl Pts',(2.88976610782154,-8.7909920213757,107.871752654495));
#46526=CARTESIAN_POINT('Ctrl Pts',(3.01428353595017,-8.79758127937177,107.835464122904));
#46527=CARTESIAN_POINT('Ctrl Pts',(3.15847582352362,-8.80417053736785,107.866686256237));
#46528=CARTESIAN_POINT('Ctrl Pts',(3.25682860860126,-8.81075979536392,107.951233149145));
#46529=CARTESIAN_POINT('Ctrl Pts',(3.35518139367891,-8.81734905335999,108.035780042052));
#46530=CARTESIAN_POINT('Ctrl Pts',(3.40769467626076,-8.82393831135607,108.173651694534));
#46531=CARTESIAN_POINT('Ctrl Pts',(3.39050882931922,-8.83052756935214,108.302205551332));
#46532=CARTESIAN_POINT('Ctrl Pts',(3.37332298237768,-8.83711682734822,108.43075940813));
#46533=CARTESIAN_POINT('Ctrl Pts',(3.28643800591276,-8.84370608534429,108.549995469245));
#46534=CARTESIAN_POINT('Ctrl Pts',(3.16933044815818,-8.85029534334036,108.605738337395));
#46535=CARTESIAN_POINT('Ctrl Pts',(3.0522228904036,-8.85688460133643,108.661481205545));
#46536=CARTESIAN_POINT('Ctrl Pts',(2.90489275135936,-8.86347385933251,108.65373088073));
#46537=CARTESIAN_POINT('Ctrl Pts',(2.7942800887535,-8.87006311732858,108.586008755069));
#46538=CARTESIAN_POINT('Ctrl Pts',(2.68366742614764,-8.87665237532465,108.518286629408));
#46539=CARTESIAN_POINT('Ctrl Pts',(2.60977223998017,-8.88324163332073,108.3905927029));
#46540=CARTESIAN_POINT('Ctrl Pts',(2.6061691135642,-8.8898308913168,108.260945238934));
#46541=CARTESIAN_POINT('Ctrl Pts',(2.60606836112365,-8.8900151434767,108.25731997107));
#46542=CARTESIAN_POINT('Ctrl Pts',(2.60602257016326,-8.8901993956366,108.253693175732));
#46543=CARTESIAN_POINT('Ctrl Pts',(2.60603107819738,-8.8903836477965,108.250066160239));
#46544=CARTESIAN_POINT('Origin',(3.,-8.675,108.25));
#46545=CARTESIAN_POINT('',(2.60706905675086,-9.03371635220349,108.250272277881));
#46546=CARTESIAN_POINT('',(2.60706396640167,-9.0153836477965,108.250274710706));
#46547=CARTESIAN_POINT('',(2.6067,-8.675,108.25));
#46548=CARTESIAN_POINT('Ctrl Pts',(2.60706905675086,-9.03371635220349,108.250272277881));
#46549=CARTESIAN_POINT('Ctrl Pts',(2.60677194109989,-9.03138908624953,108.296397492467));
#46550=CARTESIAN_POINT('Ctrl Pts',(2.61428275998129,-9.02906182029556,108.342429055414));
#46551=CARTESIAN_POINT('Ctrl Pts',(2.63003080648701,-9.02673455434159,108.385444985715));
#46552=CARTESIAN_POINT('Ctrl Pts',(2.67461872355916,-9.02014529634552,108.507237281181));
#46553=CARTESIAN_POINT('Ctrl Pts',(2.78523979738068,-9.01355603834945,108.604854969331));
#46554=CARTESIAN_POINT('Ctrl Pts',(2.91163288575999,-9.00696678035337,108.633945050007));
#46555=CARTESIAN_POINT('Ctrl Pts',(3.0380259741393,-9.0003775223573,108.663035130683));
#46556=CARTESIAN_POINT('Ctrl Pts',(3.18019107707638,-8.99378826436123,108.623597603887));
#46557=CARTESIAN_POINT('Ctrl Pts',(3.27353489235059,-8.98719900636515,108.533551072949));
#46558=CARTESIAN_POINT('Ctrl Pts',(3.36687870762481,-8.98060974836908,108.443504542012));
#46559=CARTESIAN_POINT('Ctrl Pts',(3.41140123523617,-8.97402049037301,108.302849006934));
#46560=CARTESIAN_POINT('Ctrl Pts',(3.3868734807111,-8.96743123237693,108.175491891539));
#46561=CARTESIAN_POINT('Ctrl Pts',(3.36234572618602,-8.96084197438086,108.048134776144));
#46562=CARTESIAN_POINT('Ctrl Pts',(3.26876768952452,-8.95425271638479,107.934076080432));
#46563=CARTESIAN_POINT('Ctrl Pts',(3.14865693852936,-8.94766345838871,107.885138844311));
#46564=CARTESIAN_POINT('Ctrl Pts',(3.02854618753419,-8.94107420039264,107.836201608189));
#46565=CARTESIAN_POINT('Ctrl Pts',(2.88190272220536,-8.93448494239657,107.852385831659));
#46566=CARTESIAN_POINT('Ctrl Pts',(2.77535460722962,-8.92789568440049,107.926338145882));
#46567=CARTESIAN_POINT('Ctrl Pts',(2.67197818794736,-8.92150257366816,107.998089067461));
#46568=CARTESIAN_POINT('Ctrl Pts',(2.60634555296498,-8.91510946293583,108.124220019083));
#46569=CARTESIAN_POINT('Ctrl Pts',(2.60603291882732,-8.9087163522035,108.250070364255));
#46570=CARTESIAN_POINT('Ctrl Pts',(2.60603107819738,-8.8903836477965,108.250066160239));
#46571=CARTESIAN_POINT('Ctrl Pts',(2.60632683596882,-8.89678865363268,108.12398321277));
#46572=CARTESIAN_POINT('Ctrl Pts',(2.67223797731359,-8.90319365946885,107.997634228976));
#46573=CARTESIAN_POINT('Ctrl Pts',(2.77593552102208,-8.90959866530503,107.925935693686));
#46574=CARTESIAN_POINT('Ctrl Pts',(2.88261612156037,-8.9161879233011,107.85217461383));
#46575=CARTESIAN_POINT('Ctrl Pts',(3.02928838930142,-8.92277718129717,107.836253455542));
#46576=CARTESIAN_POINT('Ctrl Pts',(3.14931117306339,-8.92936643929325,107.885406062908));
#46577=CARTESIAN_POINT('Ctrl Pts',(3.26933395682536,-8.93595569728932,107.934558670273));
#46578=CARTESIAN_POINT('Ctrl Pts',(3.36270725660825,-8.94254495528539,108.048785043293));
#46579=CARTESIAN_POINT('Ctrl Pts',(3.38700652765649,-8.94913421328147,108.17618595718));
#46580=CARTESIAN_POINT('Ctrl Pts',(3.41130579870474,-8.95572347127754,108.303586871068));
#46581=CARTESIAN_POINT('Ctrl Pts',(3.36653104101834,-8.96231272927362,108.444162325823));
#46582=CARTESIAN_POINT('Ctrl Pts',(3.27302585084809,-8.96890198726969,108.534041282448));
#46583=CARTESIAN_POINT('Ctrl Pts',(3.17952066067784,-8.97549124526576,108.623920239073));
#46584=CARTESIAN_POINT('Ctrl Pts',(3.03728503802373,-8.98208050326183,108.663102697569));
#46585=CARTESIAN_POINT('Ctrl Pts',(2.91094432603153,-8.98866976125791,108.633785945939));
#46586=CARTESIAN_POINT('Ctrl Pts',(2.78460361403932,-8.99525901925398,108.604469194309));
#46587=CARTESIAN_POINT('Ctrl Pts',(2.67415781270903,-9.00184827725005,108.506653232554));
#46588=CARTESIAN_POINT('Ctrl Pts',(2.62978842845092,-9.00843753524613,108.384781147262));
#46589=CARTESIAN_POINT('Ctrl Pts',(2.61419766253913,-9.01075290609625,108.341957042652));
#46590=CARTESIAN_POINT('Ctrl Pts',(2.60676547676824,-9.01306827694638,108.296162682987));
#46591=CARTESIAN_POINT('Ctrl Pts',(2.60706396640167,-9.0153836477965,108.250274710706));
#46592=CARTESIAN_POINT('Origin',(3.,-8.675,108.25));
#46593=CARTESIAN_POINT('',(2.60697943945107,-9.1587163522035,108.24969186562));
#46594=CARTESIAN_POINT('',(2.60698518571652,-9.1403836477965,108.249693765459));
#46595=CARTESIAN_POINT('',(2.6067,-8.675,108.25));
#46596=CARTESIAN_POINT('Ctrl Pts',(2.60697943945107,-9.1587163522035,108.24969186562));
#46597=CARTESIAN_POINT('Ctrl Pts',(2.60763355898486,-9.1542579675593,108.338003969973));
#46598=CARTESIAN_POINT('Ctrl Pts',(2.63709990068649,-9.14979958291511,108.426711728349));
#46599=CARTESIAN_POINT('Ctrl Pts',(2.69175327539567,-9.14534119827092,108.495370138938));
#46600=CARTESIAN_POINT('Ctrl Pts',(2.77252808848497,-9.13875194027485,108.596843658403));
#46601=CARTESIAN_POINT('Ctrl Pts',(2.90831965608537,-9.13216268227877,108.654522815708));
#46602=CARTESIAN_POINT('Ctrl Pts',(3.03743051806054,-9.1255734242827,108.642200847298));
#46603=CARTESIAN_POINT('Ctrl Pts',(3.16654138003572,-9.11898416628663,108.629878878888));
#46604=CARTESIAN_POINT('Ctrl Pts',(3.28897153638567,-9.11239490829055,108.547555784765));
#46605=CARTESIAN_POINT('Ctrl Pts',(3.34909433947442,-9.10580565029448,108.432635403056));
#46606=CARTESIAN_POINT('Ctrl Pts',(3.40921714256317,-9.09921639229841,108.317715021347));
#46607=CARTESIAN_POINT('Ctrl Pts',(3.40703259239072,-9.09262713430233,108.170197352054));
#46608=CARTESIAN_POINT('Ctrl Pts',(3.34353324834952,-9.08603787630626,108.057107658049));
#46609=CARTESIAN_POINT('Ctrl Pts',(3.28003390430832,-9.07944861831018,107.944017964045));
#46610=CARTESIAN_POINT('Ctrl Pts',(3.15521976639838,-9.07285936031411,107.865356245329));
#46611=CARTESIAN_POINT('Ctrl Pts',(3.02580065415689,-9.06627010231804,107.856862778983));
#46612=CARTESIAN_POINT('Ctrl Pts',(2.8963815419154,-9.05968084432196,107.848369312637));
#46613=CARTESIAN_POINT('Ctrl Pts',(2.76235745534236,-9.05309158632589,107.910044098659));
#46614=CARTESIAN_POINT('Ctrl Pts',(2.68462279221722,-9.04650232832981,108.013864943062));
#46615=CARTESIAN_POINT('Ctrl Pts',(2.63434330462809,-9.04224033628771,108.081017210118));
#46616=CARTESIAN_POINT('Ctrl Pts',(2.60761317356649,-9.0379783442456,108.165801787015));
#46617=CARTESIAN_POINT('Ctrl Pts',(2.60706905675086,-9.03371635220349,108.250272277881));
#46618=CARTESIAN_POINT('Ctrl Pts',(2.60706396640167,-9.0153836477965,108.250274710706));
#46619=CARTESIAN_POINT('Ctrl Pts',(2.60761494120877,-9.01965753494245,108.165571210669));
#46620=CARTESIAN_POINT('Ctrl Pts',(2.63450631907698,-9.0239314220884,108.080548748322));
#46621=CARTESIAN_POINT('Ctrl Pts',(2.68504684679851,-9.02820530923435,108.013299605715));
#46622=CARTESIAN_POINT('Ctrl Pts',(2.76296761659014,-9.03479456723042,107.909618358289));
#46623=CARTESIAN_POINT('Ctrl Pts',(2.89710212335932,-9.0413838252265,107.848184072265));
#46624=CARTESIAN_POINT('Ctrl Pts',(3.02650579945226,-9.04797308322257,107.856909669463));
#46625=CARTESIAN_POINT('Ctrl Pts',(3.15590947554519,-9.05456234121864,107.865635266662));
#46626=CARTESIAN_POINT('Ctrl Pts',(3.28058232096189,-9.06115159921472,107.944520747083));
#46627=CARTESIAN_POINT('Ctrl Pts',(3.34387871299737,-9.06774085721079,108.05772416659));
#46628=CARTESIAN_POINT('Ctrl Pts',(3.40717510503286,-9.07433011520686,108.170927586097));
#46629=CARTESIAN_POINT('Ctrl Pts',(3.40909504368714,-9.08091937320294,108.31844894469));
#46630=CARTESIAN_POINT('Ctrl Pts',(3.34876619689658,-9.08750863119901,108.433261303248));
#46631=CARTESIAN_POINT('Ctrl Pts',(3.28843735010602,-9.09409788919509,108.548073661807));
#46632=CARTESIAN_POINT('Ctrl Pts',(3.16585971787063,-9.10068714719116,108.63017702033));
#46633=CARTESIAN_POINT('Ctrl Pts',(3.03672695412273,-9.10727640518723,108.642267378464));
#46634=CARTESIAN_POINT('Ctrl Pts',(2.90759419037484,-9.11386566318331,108.654357736598));
#46635=CARTESIAN_POINT('Ctrl Pts',(2.77190629511443,-9.12045492117938,108.596435094343));
#46636=CARTESIAN_POINT('Ctrl Pts',(2.69131362448212,-9.12704417917545,108.494816843654));
#46637=CARTESIAN_POINT('Ctrl Pts',(2.63692897795453,-9.1314906687158,108.426243949852));
#46638=CARTESIAN_POINT('Ctrl Pts',(2.60763287690707,-9.13593715825616,108.337773519252));
#46639=CARTESIAN_POINT('Ctrl Pts',(2.60698518571652,-9.1403836477965,108.249693765459));
#46640=CARTESIAN_POINT('Origin',(3.,-8.675,108.25));
#46641=CARTESIAN_POINT('',(2.60601707190308,-9.2837163522035,108.250000088186));
#46642=CARTESIAN_POINT('',(2.60601708531384,-9.26538364779651,108.249995786147));
#46643=CARTESIAN_POINT('',(2.6067,-8.675,108.25));
#46644=CARTESIAN_POINT('Ctrl Pts',(2.60601707359714,-9.2837163522035,108.250000088186));
#46645=CARTESIAN_POINT('Ctrl Pts',(2.60601663870951,-9.27712684886908,108.379702432267));
#46646=CARTESIAN_POINT('Ctrl Pts',(2.67634181801385,-9.27053734553466,108.509404370714));
#46647=CARTESIAN_POINT('Ctrl Pts',(2.78503705730119,-9.26394784220024,108.580171898013));
#46648=CARTESIAN_POINT('Ctrl Pts',(2.8937282496811,-9.25735858420417,108.650936790518));
#46649=CARTESIAN_POINT('Ctrl Pts',(3.04078664484427,-9.2507693262081,108.662771660248));
#46650=CARTESIAN_POINT('Ctrl Pts',(3.15939564839677,-9.24418006821202,108.610299286235));
#46651=CARTESIAN_POINT('Ctrl Pts',(3.27800465194927,-9.23759081021595,108.557826912222));
#46652=CARTESIAN_POINT('Ctrl Pts',(3.36816426389111,-9.23100155221988,108.441047294465));
#46653=CARTESIAN_POINT('Ctrl Pts',(3.38891009394621,-9.2244122942238,108.313019734585));
#46654=CARTESIAN_POINT('Ctrl Pts',(3.40965592400131,-9.21782303622773,108.184992174704));
#46655=CARTESIAN_POINT('Ctrl Pts',(3.36098797216966,-9.21123377823166,108.045716672699));
#46656=CARTESIAN_POINT('Ctrl Pts',(3.26501872258032,-9.20464452023558,107.958473628877));
#46657=CARTESIAN_POINT('Ctrl Pts',(3.16904947299098,-9.19805526223951,107.871230585055));
#46658=CARTESIAN_POINT('Ctrl Pts',(3.02577892564394,-9.19146600424344,107.836019999416));
#46659=CARTESIAN_POINT('Ctrl Pts',(2.90030264644593,-9.18487674624736,107.868839947004));
#46660=CARTESIAN_POINT('Ctrl Pts',(2.77482636724793,-9.17828748825129,107.901659894592));
#46661=CARTESIAN_POINT('Ctrl Pts',(2.66714435619896,-9.17169823025521,108.002510375407));
#46662=CARTESIAN_POINT('Ctrl Pts',(2.62618237996357,-9.16510897225914,108.125569556628));
#46663=CARTESIAN_POINT('Ctrl Pts',(2.61293585301738,-9.16297809890726,108.165365164892));
#46664=CARTESIAN_POINT('Ctrl Pts',(2.60666680472018,-9.16084722555538,108.207483324896));
#46665=CARTESIAN_POINT('Ctrl Pts',(2.60697943945107,-9.1587163522035,108.24969186562));
#46666=CARTESIAN_POINT('Ctrl Pts',(2.60698518571652,-9.1403836477965,108.249693765459));
#46667=CARTESIAN_POINT('Ctrl Pts',(2.60667306258218,-9.14252641625223,108.207248030166));
#46668=CARTESIAN_POINT('Ctrl Pts',(2.61301392315575,-9.14466918470795,108.16489302125));
#46669=CARTESIAN_POINT('Ctrl Pts',(2.62640615645749,-9.14681195316367,108.1248992189));
#46670=CARTESIAN_POINT('Ctrl Pts',(2.66758880506941,-9.15340121115974,108.001913703958));
#46671=CARTESIAN_POINT('Ctrl Pts',(2.77545154829749,-9.15999046915582,107.901256533195));
#46672=CARTESIAN_POINT('Ctrl Pts',(2.90098650287746,-9.16657972715189,107.868661708252));
#46673=CARTESIAN_POINT('Ctrl Pts',(3.02652145745744,-9.17316898514797,107.836066883309));
#46674=CARTESIAN_POINT('Ctrl Pts',(3.1697286233893,-9.17975824314404,107.871534404184));
#46675=CARTESIAN_POINT('Ctrl Pts',(3.2655412327813,-9.18634750114011,107.958949456164));
#46676=CARTESIAN_POINT('Ctrl Pts',(3.3613538421733,-9.19293675913618,108.046364508145));
#46677=CARTESIAN_POINT('Ctrl Pts',(3.40977189502544,-9.19952601713226,108.18572709123));
#46678=CARTESIAN_POINT('Ctrl Pts',(3.38879644895739,-9.20611527512833,108.313717239644));
#46679=CARTESIAN_POINT('Ctrl Pts',(3.36782100288935,-9.21270453312441,108.441707388058));
#46680=CARTESIAN_POINT('Ctrl Pts',(3.27745205790112,-9.21929379112049,108.5583251018));
#46681=CARTESIAN_POINT('Ctrl Pts',(3.15874911753129,-9.22588304911656,108.61058464062));
#46682=CARTESIAN_POINT('Ctrl Pts',(3.04004617716147,-9.23247230711263,108.662844179439));
#46683=CARTESIAN_POINT('Ctrl Pts',(2.89300924141004,-9.2390615651087,108.650745543336));
#46684=CARTESIAN_POINT('Ctrl Pts',(2.78444515030389,-9.24565082310478,108.57978579747));
#46685=CARTESIAN_POINT('Ctrl Pts',(2.6760729998083,-9.25222843133535,108.508951507975));
#46686=CARTESIAN_POINT('Ctrl Pts',(2.6060377747357,-9.25880603956593,108.379464056852));
#46687=CARTESIAN_POINT('Ctrl Pts',(2.60601710832407,-9.26538364779651,108.249995786289));
#46688=CARTESIAN_POINT('Origin',(3.,-8.675,108.25));
#46689=CARTESIAN_POINT('',(2.60697942739454,-9.4087163522035,108.250308115953));
#46690=CARTESIAN_POINT('',(2.60697382714618,-9.3903836477965,108.250309930203));
#46691=CARTESIAN_POINT('',(2.6067,-8.675,108.25));
#46692=CARTESIAN_POINT('Ctrl Pts',(2.60697942739454,-9.4087163522035,108.250308115953));
#46693=CARTESIAN_POINT('Ctrl Pts',(2.60666701491607,-9.40658498817493,108.292526395753));
#46694=CARTESIAN_POINT('Ctrl Pts',(2.61293922160114,-9.40445362414636,108.334654279803));
#46695=CARTESIAN_POINT('Ctrl Pts',(2.62619185344577,-9.40232226011779,108.374458046898));
#46696=CARTESIAN_POINT('Ctrl Pts',(2.66716327324111,-9.39573300212172,108.497514121361));
#46697=CARTESIAN_POINT('Ctrl Pts',(2.7748521733323,-9.38914374412564,108.598356759879));
#46698=CARTESIAN_POINT('Ctrl Pts',(2.90033072587369,-9.38255448612957,108.631167456806));
#46699=CARTESIAN_POINT('Ctrl Pts',(3.02580927841509,-9.3759652281335,108.663978153734));
#46700=CARTESIAN_POINT('Ctrl Pts',(3.16907748340668,-9.36937597013742,108.628756909072));
#46701=CARTESIAN_POINT('Ctrl Pts',(3.26504034884136,-9.36278671214135,108.541506748758));
#46702=CARTESIAN_POINT('Ctrl Pts',(3.36100321427603,-9.35619745414527,108.454256588444));
#46703=CARTESIAN_POINT('Ctrl Pts',(3.40966074015377,-9.3496081961492,108.314977512479));
#46704=CARTESIAN_POINT('Ctrl Pts',(3.38890540409867,-9.34301893815313,108.186951495083));
#46705=CARTESIAN_POINT('Ctrl Pts',(3.36815006804357,-9.33642968015705,108.058925477687));
#46706=CARTESIAN_POINT('Ctrl Pts',(3.27798187005562,-9.32984042216098,107.94215251886));
#46707=CARTESIAN_POINT('Ctrl Pts',(3.15936899998641,-9.32325116416491,107.889688917974));
#46708=CARTESIAN_POINT('Ctrl Pts',(3.04075612991719,-9.31666190616883,107.837225317089));
#46709=CARTESIAN_POINT('Ctrl Pts',(2.8936985877667,-9.31007264817276,107.849071074143));
#46710=CARTESIAN_POINT('Ctrl Pts',(2.78501262337676,-9.30348339017669,107.919844009963));
#46711=CARTESIAN_POINT('Ctrl Pts',(2.67633070569959,-9.29689437751896,107.990614310688));
#46712=CARTESIAN_POINT('Ctrl Pts',(2.6060175084524,-9.29030536486123,108.12030740218));
#46713=CARTESIAN_POINT('Ctrl Pts',(2.60601707359714,-9.2837163522035,108.250000088186));
#46714=CARTESIAN_POINT('Ctrl Pts',(2.60601710832407,-9.26538364779651,108.249995786289));
#46715=CARTESIAN_POINT('Ctrl Pts',(2.60599636870685,-9.27198455555808,108.120068906779));
#46716=CARTESIAN_POINT('Ctrl Pts',(2.67660005833137,-9.27858546331965,107.990161542424));
#46717=CARTESIAN_POINT('Ctrl Pts',(2.78560517593341,-9.28518637108122,107.919458890809));
#46718=CARTESIAN_POINT('Ctrl Pts',(2.89441791331987,-9.29177562907729,107.848881020413));
#46719=CARTESIAN_POINT('Ctrl Pts',(3.04149645195734,-9.29836488707337,107.837299069189));
#46720=CARTESIAN_POINT('Ctrl Pts',(3.16001504540131,-9.30495414506944,107.889975346291));
#46721=CARTESIAN_POINT('Ctrl Pts',(3.27853363884528,-9.31154340306551,107.942651623393));
#46722=CARTESIAN_POINT('Ctrl Pts',(3.36849228709577,-9.31813266106159,108.05958612882));
#46723=CARTESIAN_POINT('Ctrl Pts',(3.38901791601593,-9.32472191905766,108.187649182856));
#46724=CARTESIAN_POINT('Ctrl Pts',(3.40954354493609,-9.33131117705373,108.315712236891));
#46725=CARTESIAN_POINT('Ctrl Pts',(3.36063615452594,-9.33790043504981,108.454903839535));
#46726=CARTESIAN_POINT('Ctrl Pts',(3.26451699895289,-9.34448969304588,108.541981718934));
#46727=CARTESIAN_POINT('Ctrl Pts',(3.16839784337984,-9.35107895104196,108.629059598332));
#46728=CARTESIAN_POINT('Ctrl Pts',(3.0250669226439,-9.35766820903803,108.664023754484));
#46729=CARTESIAN_POINT('Ctrl Pts',(2.89964727847269,-9.3642574670341,108.630988060613));
#46730=CARTESIAN_POINT('Ctrl Pts',(2.77422763430147,-9.37084672503017,108.597952366742));
#46731=CARTESIAN_POINT('Ctrl Pts',(2.66671926669498,-9.37743598302625,108.496916822849));
#46732=CARTESIAN_POINT('Ctrl Pts',(2.62596894818531,-9.38402524102232,108.373787384875));
#46733=CARTESIAN_POINT('Ctrl Pts',(2.61286139741018,-9.38614470994705,108.334182164127));
#46734=CARTESIAN_POINT('Ctrl Pts',(2.60666077129626,-9.38826417887178,108.292291063789));
#46735=CARTESIAN_POINT('Ctrl Pts',(2.60697382714618,-9.3903836477965,108.250309930203));
#46736=CARTESIAN_POINT('Origin',(3.,-8.675,108.25));
#46737=CARTESIAN_POINT('',(2.60697877099099,-9.5337163522035,108.249759674367));
#46738=CARTESIAN_POINT('',(2.60706672186757,-9.51538364779651,108.249732606859));
#46739=CARTESIAN_POINT('',(2.6067,-8.675,108.25));
#46740=CARTESIAN_POINT('Ctrl Pts',(2.60697877099099,-9.5337163522035,108.249759674367));
#46741=CARTESIAN_POINT('Ctrl Pts',(2.60754699255653,-9.52945386948471,108.334231172059));
#46742=CARTESIAN_POINT('Ctrl Pts',(2.63434920343294,-9.52519138676591,108.419009166244));
#46743=CARTESIAN_POINT('Ctrl Pts',(2.68466392975194,-9.52092890404712,108.486158593116));
#46744=CARTESIAN_POINT('Ctrl Pts',(2.762444119043,-9.51433964605104,108.589963095596));
#46745=CARTESIAN_POINT('Ctrl Pts',(2.89641273295953,-9.50775038805497,108.651640186054));
#46746=CARTESIAN_POINT('Ctrl Pts',(3.02581531647536,-9.50116113005889,108.643140007765));
#46747=CARTESIAN_POINT('Ctrl Pts',(3.1552178999912,-9.49457187206282,108.634639829476));
#46748=CARTESIAN_POINT('Ctrl Pts',(3.28005445310634,-9.48798261406675,108.555962382439));
#46749=CARTESIAN_POINT('Ctrl Pts',(3.3435531514507,-9.48139335607067,108.442866111883));
#46750=CARTESIAN_POINT('Ctrl Pts',(3.40705184979507,-9.4748040980746,108.329769841328));
#46751=CARTESIAN_POINT('Ctrl Pts',(3.40921269336866,-9.46821484007852,108.182254747253));
#46752=CARTESIAN_POINT('Ctrl Pts',(3.34907795614323,-9.46162558208245,108.067339519195));
#46753=CARTESIAN_POINT('Ctrl Pts',(3.2889432189178,-9.45503632408638,107.952424291138));
#46754=CARTESIAN_POINT('Ctrl Pts',(3.16651290089336,-9.4484470660903,107.870108929098));
#46755=CARTESIAN_POINT('Ctrl Pts',(3.03740273717822,-9.44185780809423,107.857796145506));
#46756=CARTESIAN_POINT('Ctrl Pts',(2.90829257346308,-9.43526855009816,107.845483361913));
#46757=CARTESIAN_POINT('Ctrl Pts',(2.77250256405724,-9.42867929210209,107.903173156768));
#46758=CARTESIAN_POINT('Ctrl Pts',(2.69173452910408,-9.42209003410601,108.004652809398));
#46759=CARTESIAN_POINT('Ctrl Pts',(2.63709175506193,-9.41763214013851,108.073307812975));
#46760=CARTESIAN_POINT('Ctrl Pts',(2.60763285950868,-9.413174246171,108.162005689753));
#46761=CARTESIAN_POINT('Ctrl Pts',(2.60697942739454,-9.4087163522035,108.250308115953));
#46762=CARTESIAN_POINT('Ctrl Pts',(2.60697382714618,-9.3903836477965,108.250309930203));
#46763=CARTESIAN_POINT('Ctrl Pts',(2.60763403669223,-9.39485343686785,108.161775104372));
#46764=CARTESIAN_POINT('Ctrl Pts',(2.63726411326604,-9.3993232259392,108.072839851989));
#46765=CARTESIAN_POINT('Ctrl Pts',(2.69217563494894,-9.40379301501054,108.004100125204));
#46766=CARTESIAN_POINT('Ctrl Pts',(2.77312490963509,-9.41038227300661,107.902765635559));
#46767=CARTESIAN_POINT('Ctrl Pts',(2.90901572842025,-9.41697153100269,107.845319988321));
#46768=CARTESIAN_POINT('Ctrl Pts',(3.03810506853297,-9.42356078899876,107.857864034878));
#46769=CARTESIAN_POINT('Ctrl Pts',(3.1671944086457,-9.43015004699484,107.870408081435));
#46770=CARTESIAN_POINT('Ctrl Pts',(3.28948227008599,-9.43673930499091,107.952941821786));
#46771=CARTESIAN_POINT('Ctrl Pts',(3.34940767562958,-9.44332856298699,108.067965307736));
#46772=CARTESIAN_POINT('Ctrl Pts',(3.40933308117317,-9.44991782098306,108.182988793687));
#46773=CARTESIAN_POINT('Ctrl Pts',(3.40689603082006,-9.45650707897913,108.330502025238));
#46774=CARTESIAN_POINT('Ctrl Pts',(3.34320159534457,-9.46309633697521,108.443482625721));
#46775=CARTESIAN_POINT('Ctrl Pts',(3.27950715986907,-9.46968559497128,108.556463226204));
#46776=CARTESIAN_POINT('Ctrl Pts',(3.15455533927118,-9.47627485296735,108.634911195619));
#46777=CARTESIAN_POINT('Ctrl Pts',(3.0251233356586,-9.48286411096342,108.643181463371));
#46778=CARTESIAN_POINT('Ctrl Pts',(2.89569133204601,-9.4894533689595,108.651451731123));
#46779=CARTESIAN_POINT('Ctrl Pts',(2.76177914541873,-9.49604262695558,108.589544297211));
#46780=CARTESIAN_POINT('Ctrl Pts',(2.68421986242852,-9.50263188495165,108.485591155156));
#46781=CARTESIAN_POINT('Ctrl Pts',(2.6341880488466,-9.5068824725666,108.418533234762));
#46782=CARTESIAN_POINT('Ctrl Pts',(2.60760614734699,-9.51113306018155,108.333978999258));
#46783=CARTESIAN_POINT('Ctrl Pts',(2.60706672186757,-9.51538364779651,108.249732606859));
#46784=CARTESIAN_POINT('Origin',(3.,-7.51222265507269,108.25));
#46785=CARTESIAN_POINT('',(2.67795342847984,-9.57472265507269,108.249803074133));
#46786=CARTESIAN_POINT('',(2.67772883664542,-9.59937734492731,108.249997529819));
#46787=CARTESIAN_POINT('',(2.677725,-7.51222265507269,108.25));
#46788=CARTESIAN_POINT('',(2.90469398989908,-9.6,107.942139739389));
#46789=CARTESIAN_POINT('Ctrl Pts',(2.67795342847984,-9.57472265507269,108.249803074133));
#46790=CARTESIAN_POINT('Ctrl Pts',(2.67769926555923,-9.57704943034997,108.212019357596));
#46791=CARTESIAN_POINT('Ctrl Pts',(2.69997452530982,-9.58547521199241,108.07546693902));
#46792=CARTESIAN_POINT('Ctrl Pts',(2.81100303866955,-9.59390099363485,107.971242620752));
#46793=CARTESIAN_POINT('Ctrl Pts',(2.90476631137571,-9.6,107.941669514675));
#46794=CARTESIAN_POINT('',(2.67788283232033,-9.6,108.239915065145));
#46795=CARTESIAN_POINT('Origin',(3.,-9.6,108.25));
#46796=CARTESIAN_POINT('Ctrl Pts',(2.67772883664542,-9.59937734492731,108.249997529819));
#46797=CARTESIAN_POINT('Ctrl Pts',(2.67772642548982,-9.59958489661821,108.246636930255));
#46798=CARTESIAN_POINT('Ctrl Pts',(2.67777761936289,-9.5997924483091,108.243275612371));
#46799=CARTESIAN_POINT('Ctrl Pts',(2.67788283232033,-9.6,108.239915065145));
#46800=CARTESIAN_POINT('Origin',(3.,-7.51222265507269,108.25));
#46801=CARTESIAN_POINT('',(2.67795396634523,-9.44972265507269,108.250252474113));
#46802=CARTESIAN_POINT('',(2.67802549654176,-9.47437734492731,108.249780894675));
#46803=CARTESIAN_POINT('',(2.677725,-7.51222265507269,108.25));
#46804=CARTESIAN_POINT('Ctrl Pts',(2.67795396634523,-9.44972265507269,108.250252474113));
#46805=CARTESIAN_POINT('Ctrl Pts',(2.67848939689337,-9.4541805490402,108.177896347992));
#46806=CARTESIAN_POINT('Ctrl Pts',(2.73830847628814,-9.46522770100378,107.997786902831));
#46807=CARTESIAN_POINT('Ctrl Pts',(3.03612182658042,-9.48286411096343,107.871262196348));
#46808=CARTESIAN_POINT('Ctrl Pts',(3.33708468501923,-9.50263188495165,108.073612946168));
#46809=CARTESIAN_POINT('Ctrl Pts',(3.33177281726424,-9.52239965893987,108.436240153971));
#46810=CARTESIAN_POINT('Ctrl Pts',(3.02489486032158,-9.54216743292809,108.629648042939));
#46811=CARTESIAN_POINT('Ctrl Pts',(2.73433168531756,-9.55960843163903,108.495877223755));
#46812=CARTESIAN_POINT('Ctrl Pts',(2.67841903642552,-9.5704601723539,108.319020088928));
#46813=CARTESIAN_POINT('Ctrl Pts',(2.67795342847984,-9.57472265507269,108.249803074133));
#46814=CARTESIAN_POINT('Ctrl Pts',(2.67802549654176,-9.47437734492731,108.249780894675));
#46815=CARTESIAN_POINT('Ctrl Pts',(2.67778230180603,-9.47671601530843,108.211799227294));
#46816=CARTESIAN_POINT('Ctrl Pts',(2.701514674746,-9.48564394368563,108.067094842141));
#46817=CARTESIAN_POINT('Ctrl Pts',(2.91535037624978,-9.50116113005889,107.879072987278));
#46818=CARTESIAN_POINT('Ctrl Pts',(3.26451785003709,-9.52092890404712,107.976673691963));
#46819=CARTESIAN_POINT('Ctrl Pts',(3.37368648223413,-9.54069667803533,108.322492331795));
#46820=CARTESIAN_POINT('Ctrl Pts',(3.1425103302508,-9.56046445202356,108.602707172509));
#46821=CARTESIAN_POINT('Ctrl Pts',(2.84350450152926,-9.57693759701374,108.568400494187));
#46822=CARTESIAN_POINT('Ctrl Pts',(2.7023541417074,-9.58990856131499,108.402984030974));
#46823=CARTESIAN_POINT('Ctrl Pts',(2.67776469963313,-9.59629026762017,108.299982334113));
#46824=CARTESIAN_POINT('Ctrl Pts',(2.67772883664542,-9.59937734492731,108.249997529819));
#46825=CARTESIAN_POINT('Origin',(3.,-7.51222265507269,108.25));
#46826=CARTESIAN_POINT('',(2.677165376484,-9.32472265507269,108.250000072264));
#46827=CARTESIAN_POINT('',(2.6779493774308,-9.34937734492731,108.250253960733));
#46828=CARTESIAN_POINT('',(2.677725,-7.51222265507269,108.25));
#46829=CARTESIAN_POINT('Ctrl Pts',(2.67716540145823,-9.32472265507269,108.250000072261));
#46830=CARTESIAN_POINT('Ctrl Pts',(2.67716575778413,-9.33131166773042,108.143728243167));
#46831=CARTESIAN_POINT('Ctrl Pts',(2.79239895133995,-9.34448993838423,107.931179963473));
#46832=CARTESIAN_POINT('Ctrl Pts',(3.15389690100588,-9.3642574670341,107.902060634909));
#46833=CARTESIAN_POINT('Ctrl Pts',(3.37555179045336,-9.38402524102232,108.189116358066));
#46834=CARTESIAN_POINT('Ctrl Pts',(3.25594001202276,-9.40379301501054,108.531497473297));
#46835=CARTESIAN_POINT('Ctrl Pts',(2.9037526682877,-9.42356078899877,108.618079674849));
#46836=CARTESIAN_POINT('Ctrl Pts',(2.69872669280949,-9.43887066901948,108.426088111054));
#46837=CARTESIAN_POINT('Ctrl Pts',(2.67769797160457,-9.44759129104412,108.284846667153));
#46838=CARTESIAN_POINT('Ctrl Pts',(2.67795396634523,-9.44972265507269,108.250252474113));
#46839=CARTESIAN_POINT('Ctrl Pts',(2.6779493774308,-9.34937734492731,108.250253960733));
#46840=CARTESIAN_POINT('Ctrl Pts',(2.67849036149248,-9.35384713399866,108.177707403411));
#46841=CARTESIAN_POINT('Ctrl Pts',(2.73856153576217,-9.36490618106608,107.997402602939));
#46842=CARTESIAN_POINT('Ctrl Pts',(3.03679699339086,-9.38255448612957,107.871328383607));
#46843=CARTESIAN_POINT('Ctrl Pts',(3.3374096596431,-9.40232226011779,108.074215959287));
#46844=CARTESIAN_POINT('Ctrl Pts',(3.33141880989063,-9.42209003410602,108.436838588562));
#46845=CARTESIAN_POINT('Ctrl Pts',(3.0242574980433,-9.44185780809423,108.629682366924));
#46846=CARTESIAN_POINT('Ctrl Pts',(2.73401479394391,-9.45928691170134,108.495503533206));
#46847=CARTESIAN_POINT('Ctrl Pts',(2.67846750860984,-9.47012675731236,108.318813455342));
#46848=CARTESIAN_POINT('Ctrl Pts',(2.67802549654176,-9.47437734492731,108.249780894675));
#46849=CARTESIAN_POINT('Origin',(3.,-7.51222265507269,108.25));
#46850=CARTESIAN_POINT('',(2.6779539762245,-9.19972265507269,108.249747510787));
#46851=CARTESIAN_POINT('',(2.67716540814336,-9.22437734492731,108.249996547097));
#46852=CARTESIAN_POINT('',(2.677725,-7.51222265507269,108.25));
#46853=CARTESIAN_POINT('Ctrl Pts',(2.6779539762245,-9.19972265507269,108.249747510787));
#46854=CARTESIAN_POINT('Ctrl Pts',(2.67769779936739,-9.20185352842457,108.21516129807));
#46855=CARTESIAN_POINT('Ctrl Pts',(2.69871958846501,-9.21057365977253,108.073927886744));
#46856=CARTESIAN_POINT('Ctrl Pts',(2.90372587748699,-9.22588304911656,107.881927545957));
#46857=CARTESIAN_POINT('Ctrl Pts',(3.25591897928919,-9.24565082310478,107.968483545095));
#46858=CARTESIAN_POINT('Ctrl Pts',(3.37555638719568,-9.265418597093,108.310855874679));
#46859=CARTESIAN_POINT('Ctrl Pts',(3.15392260429289,-9.28518637108122,108.597927967071));
#46860=CARTESIAN_POINT('Ctrl Pts',(2.79241807110289,-9.30495414506944,108.568835040736));
#46861=CARTESIAN_POINT('Ctrl Pts',(2.67716719052207,-9.31813290639993,108.356283772265));
#46862=CARTESIAN_POINT('Ctrl Pts',(2.67716540144496,-9.32472240973435,108.250004029235));
#46863=CARTESIAN_POINT('Ctrl Pts',(2.67716540145823,-9.32472265507269,108.250000072261));
#46864=CARTESIAN_POINT('Ctrl Pts',(2.67716542991391,-9.22437734492731,108.249996547232));
#46865=CARTESIAN_POINT('Ctrl Pts',(2.67716539992112,-9.22438899469281,108.249808652243));
#46866=CARTESIAN_POINT('Ctrl Pts',(2.67725037642591,-9.23098990245438,108.143344949962));
#46867=CARTESIAN_POINT('Ctrl Pts',(2.7929666844032,-9.24418006821203,107.930808426606));
#46868=CARTESIAN_POINT('Ctrl Pts',(3.15452073504689,-9.26394784220025,107.902337234153));
#46869=CARTESIAN_POINT('Ctrl Pts',(3.37566050136972,-9.28371561618847,108.1897900773));
#46870=CARTESIAN_POINT('Ctrl Pts',(3.25543449645413,-9.30348339017669,108.531956162289));
#46871=CARTESIAN_POINT('Ctrl Pts',(2.90309298249399,-9.32325116416491,108.617906379101));
#46872=CARTESIAN_POINT('Ctrl Pts',(2.6985697470388,-9.33854914908178,108.42569700235));
#46873=CARTESIAN_POINT('Ctrl Pts',(2.67769285550344,-9.34725787600258,108.284653833162));
#46874=CARTESIAN_POINT('Ctrl Pts',(2.6779493774308,-9.34937734492731,108.250253960733));
#46875=CARTESIAN_POINT('Origin',(3.,-7.51222265507269,108.25));
#46876=CARTESIAN_POINT('',(2.67802740977468,-9.07472265507269,108.250223107943));
#46877=CARTESIAN_POINT('',(2.67795868478717,-9.09937734492731,108.24974906754));
#46878=CARTESIAN_POINT('',(2.677725,-7.51222265507269,108.25));
#46879=CARTESIAN_POINT('Ctrl Pts',(2.67802740977468,-9.07472265507269,108.250223107943));
#46880=CARTESIAN_POINT('Ctrl Pts',(2.67847326598307,-9.0789846471148,108.181006918155));
#46881=CARTESIAN_POINT('Ctrl Pts',(2.73423944584299,-9.08983589715298,108.004123686505));
#46882=CARTESIAN_POINT('Ctrl Pts',(3.02491475698223,-9.10727640518723,107.870361628692));
#46883=CARTESIAN_POINT('Ctrl Pts',(3.331737612016,-9.12704417917545,108.063730853703));
#46884=CARTESIAN_POINT('Ctrl Pts',(3.33710775623283,-9.14681195316367,108.426364392007));
#46885=CARTESIAN_POINT('Ctrl Pts',(3.0361452952284,-9.1665797271519,108.628734149129));
#46886=CARTESIAN_POINT('Ctrl Pts',(2.73832024171984,-9.18421662778823,108.502229253324));
#46887=CARTESIAN_POINT('Ctrl Pts',(2.678489970053,-9.1952642704285,108.32211156731));
#46888=CARTESIAN_POINT('Ctrl Pts',(2.6779539762245,-9.19972265507269,108.249747510787));
#46889=CARTESIAN_POINT('Ctrl Pts',(2.67795868478717,-9.09937734492731,108.24974906754));
#46890=CARTESIAN_POINT('Ctrl Pts',(2.67770292713876,-9.10152011338304,108.214968494589));
#46891=CARTESIAN_POINT('Ctrl Pts',(2.69887633057988,-9.11025213983483,108.073536636701));
#46892=CARTESIAN_POINT('Ctrl Pts',(2.90438625299112,-9.1255734242827,107.881755427227));
#46893=CARTESIAN_POINT('Ctrl Pts',(3.2564235481909,-9.14534119827092,107.968943034321));
#46894=CARTESIAN_POINT('Ctrl Pts',(3.37544664493324,-9.16510897225914,108.311529429926));
#46895=CARTESIAN_POINT('Ctrl Pts',(3.15329827158403,-9.18487674624737,108.59820352372));
#46896=CARTESIAN_POINT('Ctrl Pts',(2.79205950553832,-9.20463287047008,108.568479724359));
#46897=CARTESIAN_POINT('Ctrl Pts',(2.67718236423328,-9.21779973669674,108.35608448747));
#46898=CARTESIAN_POINT('Ctrl Pts',(2.67716542991391,-9.22437734492731,108.249996547232));
#46899=CARTESIAN_POINT('Origin',(3.,-7.51222265507269,108.25));
#46900=CARTESIAN_POINT('',(2.67717838524047,-8.94972265507269,108.250057657362));
#46901=CARTESIAN_POINT('',(2.67802323867811,-8.97437734492731,108.25022510143));
#46902=CARTESIAN_POINT('',(2.677725,-7.51222265507269,108.25));
#46903=CARTESIAN_POINT('Ctrl Pts',(2.67717838524047,-8.94972265507269,108.250057657362));
#46904=CARTESIAN_POINT('Ctrl Pts',(2.67743456161147,-8.95611576580502,108.146934290999));
#46905=CARTESIAN_POINT('Ctrl Pts',(2.78664501856536,-8.96909813453343,107.937056706984));
#46906=CARTESIAN_POINT('Ctrl Pts',(3.14355261982312,-8.9886697612579,107.897666800561));
#46907=CARTESIAN_POINT('Ctrl Pts',(3.37358970422498,-9.00843753524613,108.178050219025));
#46908=CARTESIAN_POINT('Ctrl Pts',(3.26414273560599,-9.02820530923435,108.523814998333));
#46909=CARTESIAN_POINT('Ctrl Pts',(2.91466707924407,-9.04797308322257,108.620761824788));
#46910=CARTESIAN_POINT('Ctrl Pts',(2.70136371725896,-9.06347886516868,108.432532038618));
#46911=CARTESIAN_POINT('Ctrl Pts',(2.67778394944817,-9.07239538911873,108.288018692817));
#46912=CARTESIAN_POINT('Ctrl Pts',(2.67802740977468,-9.07472265507269,108.250223107943));
#46913=CARTESIAN_POINT('Ctrl Pts',(2.67802323867811,-8.97437734492731,108.25022510143));
#46914=CARTESIAN_POINT('Ctrl Pts',(2.67847471441155,-8.97865123207326,108.180817980977));
#46915=CARTESIAN_POINT('Ctrl Pts',(2.73448248140951,-8.98951437721528,108.003738238763));
#46916=CARTESIAN_POINT('Ctrl Pts',(3.02559569024832,-9.00696678035338,107.87040690913));
#46917=CARTESIAN_POINT('Ctrl Pts',(3.332071214708,-9.02673455434159,108.064326193666));
#46918=CARTESIAN_POINT('Ctrl Pts',(3.33679088083925,-9.04650232832982,108.426968801146));
#46919=CARTESIAN_POINT('Ctrl Pts',(3.03546588901117,-9.06627010231804,108.628798395868));
#46920=CARTESIAN_POINT('Ctrl Pts',(2.73806892801327,-9.08389510785053,108.501845156991));
#46921=CARTESIAN_POINT('Ctrl Pts',(2.67848941114982,-9.09493085538696,108.321922733071));
#46922=CARTESIAN_POINT('Ctrl Pts',(2.67795868478717,-9.09937734492731,108.24974906754));
#46923=CARTESIAN_POINT('Origin',(3.,-7.51222265507269,108.25));
#46924=CARTESIAN_POINT('',(2.67787169029203,-8.82472265507269,108.249726345659));
#46925=CARTESIAN_POINT('',(2.67717687700499,-8.84937734492731,108.250054212538));
#46926=CARTESIAN_POINT('',(2.677725,-7.51222265507269,108.25));
#46927=CARTESIAN_POINT('Ctrl Pts',(2.67787169029203,-8.82472265507269,108.249726345659));
#46928=CARTESIAN_POINT('Ctrl Pts',(2.67761485306344,-8.82665762649918,108.218340113235));
#46929=CARTESIAN_POINT('Ctrl Pts',(2.69619998288975,-8.83518185592173,108.080370347943));
#46930=CARTESIAN_POINT('Ctrl Pts',(2.89289612067176,-8.85029534334036,107.884931791143));
#46931=CARTESIAN_POINT('Ctrl Pts',(3.24749216158505,-8.87006311732858,107.961047290999));
#46932=CARTESIAN_POINT('Ctrl Pts',(3.37719002903275,-8.88983089131681,108.299736506548));
#46933=CARTESIAN_POINT('Ctrl Pts',(3.16413219853988,-8.90959866530502,108.593229747382));
#46934=CARTESIAN_POINT('Ctrl Pts',(2.80192608220999,-8.92936643929325,108.574827278991));
#46935=CARTESIAN_POINT('Ctrl Pts',(2.67864156962831,-8.94274110254913,108.362665331578));
#46936=CARTESIAN_POINT('Ctrl Pts',(2.67717052548388,-8.94952650780894,108.253221589129));
#46937=CARTESIAN_POINT('Ctrl Pts',(2.67717838524047,-8.94972265507269,108.250057657362));
#46938=CARTESIAN_POINT('Ctrl Pts',(2.67717687700499,-8.84937734492731,108.250054212538));
#46939=CARTESIAN_POINT('Ctrl Pts',(2.67741922466783,-8.85578235076348,108.146740248908));
#46940=CARTESIAN_POINT('Ctrl Pts',(2.78698972715461,-8.86877661459573,107.936698041163));
#46941=CARTESIAN_POINT('Ctrl Pts',(3.14418439041029,-8.88836013642405,107.897924843879));
#46942=CARTESIAN_POINT('Ctrl Pts',(3.37371818283995,-8.90812791041227,108.178720453069));
#46943=CARTESIAN_POINT('Ctrl Pts',(3.26365117266921,-8.9278956844005,108.524288375886));
#46944=CARTESIAN_POINT('Ctrl Pts',(2.91400216206011,-8.94766345838871,108.620608183754));
#46945=CARTESIAN_POINT('Ctrl Pts',(2.70120014077517,-8.96315734523099,108.432140771461));
#46946=CARTESIAN_POINT('Ctrl Pts',(2.67777865249297,-8.97206197407719,108.287826286956));
#46947=CARTESIAN_POINT('Ctrl Pts',(2.67802323867811,-8.97437734492731,108.25022510143));
#46948=CARTESIAN_POINT('Origin',(3.,-7.51222265507269,108.25));
#46949=CARTESIAN_POINT('',(2.67808974459385,-8.69972265507269,108.25018671496));
#46950=CARTESIAN_POINT('',(2.67787688739042,-8.72437734492731,108.249727382091));
#46951=CARTESIAN_POINT('',(2.677725,-7.51222265507269,108.25));
#46952=CARTESIAN_POINT('Ctrl Pts',(2.67808974459385,-8.69972265507269,108.25018671496));
#46953=CARTESIAN_POINT('Ctrl Pts',(2.67844137132719,-8.7037887451894,108.18411989593));
#46954=CARTESIAN_POINT('Ctrl Pts',(2.73031217787741,-8.71444409330218,108.010482462731));
#46955=CARTESIAN_POINT('Ctrl Pts',(3.01369050100825,-8.73168869941104,107.869791362187));
#46956=CARTESIAN_POINT('Ctrl Pts',(3.32609103551689,-8.75145647339926,108.054013585571));
#46957=CARTESIAN_POINT('Ctrl Pts',(3.34216994997271,-8.77122424738748,108.416330284137));
#46958=CARTESIAN_POINT('Ctrl Pts',(3.04731620187133,-8.7909920213757,108.62750127831));
#46959=CARTESIAN_POINT('Ctrl Pts',(2.74253636262819,-8.80882482393743,108.508541612906));
#46960=CARTESIAN_POINT('Ctrl Pts',(2.6784894741245,-8.8200683685031,108.325221269276));
#46961=CARTESIAN_POINT('Ctrl Pts',(2.67787169029203,-8.82472265507269,108.249726345659));
#46962=CARTESIAN_POINT('Ctrl Pts',(2.67787688739042,-8.72437734492731,108.249727382091));
#46963=CARTESIAN_POINT('Ctrl Pts',(2.67761976356994,-8.72632421145764,108.218146907246));
#46964=CARTESIAN_POINT('Ctrl Pts',(2.69634964036998,-8.73486033598403,108.079979216136));
#46965=CARTESIAN_POINT('Ctrl Pts',(2.89355112400359,-8.7499857185065,107.884740242026));
#46966=CARTESIAN_POINT('Ctrl Pts',(3.2480100826438,-8.76975349249473,107.961491676198));
#46967=CARTESIAN_POINT('Ctrl Pts',(3.37710022867022,-8.78952126648294,108.300413009558));
#46968=CARTESIAN_POINT('Ctrl Pts',(3.16351627908797,-8.80928904047117,108.593523624325));
#46969=CARTESIAN_POINT('Ctrl Pts',(2.80134373476698,-8.82905681445938,108.574471481458));
#46970=CARTESIAN_POINT('Ctrl Pts',(2.67854928445123,-8.84241958261143,108.362277611636));
#46971=CARTESIAN_POINT('Ctrl Pts',(2.6771699054141,-8.84919309276741,108.253026234958));
#46972=CARTESIAN_POINT('Ctrl Pts',(2.67717687700499,-8.84937734492731,108.250054212538));
#46973=CARTESIAN_POINT('Origin',(3.,-7.51222265507269,108.25));
#46974=CARTESIAN_POINT('',(2.6772145464451,-8.5747226550727,108.250112544086));
#46975=CARTESIAN_POINT('',(2.67808628304073,-8.59937734492731,108.250189104615));
#46976=CARTESIAN_POINT('',(2.677725,-7.51222265507269,108.25));
#46977=CARTESIAN_POINT('Ctrl Pts',(2.6772145464451,-8.5747226550727,108.250112544086));
#46978=CARTESIAN_POINT('Ctrl Pts',(2.67766872176062,-8.58091986387963,108.150119216553));
#46979=CARTESIAN_POINT('Ctrl Pts',(2.78105395378419,-8.59370633068263,107.942995497513));
#46980=CARTESIAN_POINT('Ctrl Pts',(3.13308311396652,-8.61308205548171,107.893580411787));
#46981=CARTESIAN_POINT('Ctrl Pts',(3.37130152025498,-8.63284982946993,108.167046885883));
#46982=CARTESIAN_POINT('Ctrl Pts',(3.27211516521468,-8.65261760345815,108.515893540624));
#46983=CARTESIAN_POINT('Ctrl Pts',(2.92565550973071,-8.67238537744637,108.623120536626));
#46984=CARTESIAN_POINT('Ctrl Pts',(2.70412150102437,-8.68808706131789,108.438975741778));
#46985=CARTESIAN_POINT('Ctrl Pts',(2.67787154645913,-8.69719948719333,108.29118375902));
#46986=CARTESIAN_POINT('Ctrl Pts',(2.67808974459385,-8.69972265507269,108.25018671496));
#46987=CARTESIAN_POINT('Ctrl Pts',(2.67808628304073,-8.59937734492731,108.250189104615));
#46988=CARTESIAN_POINT('Ctrl Pts',(2.67844368879407,-8.60345533014786,108.183930786673));
#46989=CARTESIAN_POINT('Ctrl Pts',(2.73054658431704,-8.61412257336448,108.01009578156));
#46990=CARTESIAN_POINT('Ctrl Pts',(3.01437247462189,-8.63137907457718,107.869816510131));
#46991=CARTESIAN_POINT('Ctrl Pts',(3.32644207722428,-8.6511468485654,108.05459881215));
#46992=CARTESIAN_POINT('Ctrl Pts',(3.34187106527198,-8.67091462255362,108.41694378912));
#46993=CARTESIAN_POINT('Ctrl Pts',(3.04663898976117,-8.69068239654184,108.627585564647));
#46994=CARTESIAN_POINT('Ctrl Pts',(2.74227616279518,-8.70850330399974,108.508159103543));
#46995=CARTESIAN_POINT('Ctrl Pts',(2.67849001079218,-8.71973495346156,108.32503245546));
#46996=CARTESIAN_POINT('Ctrl Pts',(2.67787688739042,-8.72437734492731,108.249727382091));
#46997=CARTESIAN_POINT('Origin',(3.,-7.51222265507269,108.25));
#46998=CARTESIAN_POINT('',(2.67778257111066,-8.44972265507269,108.249714163392));
#46999=CARTESIAN_POINT('',(2.67721174697152,-8.47437734492731,108.250109332317));
#47000=CARTESIAN_POINT('',(2.677725,-7.51222265507269,108.25));
#47001=CARTESIAN_POINT('Ctrl Pts',(2.67778257111066,-8.44972265507269,108.249714163392));
#47002=CARTESIAN_POINT('Ctrl Pts',(2.67753611923224,-8.45146172457378,108.221525381468));
#47003=CARTESIAN_POINT('Ctrl Pts',(2.69379582962807,-8.45979005207093,108.086810217949));
#47004=CARTESIAN_POINT('Ctrl Pts',(2.8821598252778,-8.47470763756417,107.888254604305));
#47005=CARTESIAN_POINT('Ctrl Pts',(3.23884937624272,-8.49447541155238,107.9538631844));
#47006=CARTESIAN_POINT('Ctrl Pts',(3.37849452424005,-8.51424318554061,108.288573737252));
#47007=CARTESIAN_POINT('Ctrl Pts',(3.17419856871655,-8.53401095952883,108.58823201614));
#47008=CARTESIAN_POINT('Ctrl Pts',(2.81160693354902,-8.55377873351705,108.580536065503));
#47009=CARTESIAN_POINT('Ctrl Pts',(2.68021280133249,-8.56734929869834,108.369055249787));
#47010=CARTESIAN_POINT('Ctrl Pts',(2.67718581430621,-8.57433060588355,108.256438344007));
#47011=CARTESIAN_POINT('Ctrl Pts',(2.6772145464451,-8.5747226550727,108.250112544086));
#47012=CARTESIAN_POINT('Ctrl Pts',(2.67721174697152,-8.47437734492731,108.250109332317));
#47013=CARTESIAN_POINT('Ctrl Pts',(2.67765544676115,-8.48058644883809,108.14992636896));
#47014=CARTESIAN_POINT('Ctrl Pts',(2.78138880871222,-8.49338481074494,107.942633191673));
#47015=CARTESIAN_POINT('Ctrl Pts',(3.1337222307341,-8.51277243064786,107.893819681898));
#47016=CARTESIAN_POINT('Ctrl Pts',(3.37144973952803,-8.53254020463607,108.167713032621));
#47017=CARTESIAN_POINT('Ctrl Pts',(3.27163779891431,-8.5523079786243,108.51638123094));
#47018=CARTESIAN_POINT('Ctrl Pts',(2.92498634456088,-8.57207575261252,108.622986602298));
#47019=CARTESIAN_POINT('Ctrl Pts',(2.70395056442066,-8.58776554138019,108.438584522633));
#47020=CARTESIAN_POINT('Ctrl Pts',(2.67786618824155,-8.59686607215179,108.290991780691));
#47021=CARTESIAN_POINT('Ctrl Pts',(2.67808628304073,-8.59937734492731,108.250189104615));
#47022=CARTESIAN_POINT('Origin',(3.,-7.51222265507269,108.25));
#47023=CARTESIAN_POINT('',(2.67813962800902,-8.32472265507269,108.250144474503));
#47024=CARTESIAN_POINT('',(2.67778811510267,-8.34937734492731,108.249714634396));
#47025=CARTESIAN_POINT('',(2.677725,-7.51222265507269,108.25));
#47026=CARTESIAN_POINT('Ctrl Pts',(2.67813962800902,-8.32472265507269,108.250144474503));
#47027=CARTESIAN_POINT('Ctrl Pts',(2.67839617368377,-8.328592843264,108.187236279716));
#47028=CARTESIAN_POINT('Ctrl Pts',(2.72652582978869,-8.33905228945139,108.01686007521));
#47029=CARTESIAN_POINT('Ctrl Pts',(3.00245429834817,-8.35610099363484,107.869552875547));
#47030=CARTESIAN_POINT('Ctrl Pts',(3.32015990357356,-8.37586876762306,108.044467340237));
#47031=CARTESIAN_POINT('Ctrl Pts',(3.34693355738075,-8.39563654161128,108.406151032172));
#47032=CARTESIAN_POINT('Ctrl Pts',(3.05844581919422,-8.4154043155995,108.625938990135));
#47033=CARTESIAN_POINT('Ctrl Pts',(2.74689995323773,-8.43343302008664,108.514826151346));
#47034=CARTESIAN_POINT('Ctrl Pts',(2.67846991458055,-8.4448724665777,108.328331438717));
#47035=CARTESIAN_POINT('Ctrl Pts',(2.67778257111066,-8.44972265507269,108.249714163392));
#47036=CARTESIAN_POINT('Ctrl Pts',(2.67778811510267,-8.34937734492731,108.249714634396));
#47037=CARTESIAN_POINT('Ctrl Pts',(2.67754074084222,-8.35112830953224,108.221331794284));
#47038=CARTESIAN_POINT('Ctrl Pts',(2.69393854225206,-8.35946853213323,108.086419277493));
#47039=CARTESIAN_POINT('Ctrl Pts',(2.88280888503356,-8.37439801273031,107.888043791918));
#47040=CARTESIAN_POINT('Ctrl Pts',(3.23938019713941,-8.39416578671853,107.954292077865));
#47041=CARTESIAN_POINT('Ctrl Pts',(3.37842474494008,-8.41393356070675,108.289252597531));
#47042=CARTESIAN_POINT('Ctrl Pts',(3.17359159824674,-8.43370133469497,108.588543957285));
#47043=CARTESIAN_POINT('Ctrl Pts',(2.81101433099364,-8.45346910868319,108.580197624016));
#47044=CARTESIAN_POINT('Ctrl Pts',(2.68011458337086,-8.46702777876064,108.368667027259));
#47045=CARTESIAN_POINT('Ctrl Pts',(2.67718458133054,-8.47399719084201,108.256243061651));
#47046=CARTESIAN_POINT('Ctrl Pts',(2.67721174697152,-8.47437734492731,108.250109332317));
#47047=CARTESIAN_POINT('Origin',(3.,-7.51222265507269,108.25));
#47048=CARTESIAN_POINT('',(2.67726984584404,-8.19972265507269,108.250162467927));
#47049=CARTESIAN_POINT('',(2.67813696047442,-8.22437734492731,108.250147181483));
#47050=CARTESIAN_POINT('',(2.677725,-7.51222265507269,108.25));
#47051=CARTESIAN_POINT('Ctrl Pts',(2.67726984584404,-8.19972265507269,108.250162467927));
#47052=CARTESIAN_POINT('Ctrl Pts',(2.6778697318139,-8.20572396195423,108.153286050659));
#47053=CARTESIAN_POINT('Ctrl Pts',(2.77562443238243,-8.21831452683184,107.948991928386));
#47054=CARTESIAN_POINT('Ctrl Pts',(3.12249747634493,-8.23749434970551,107.889805043942));
#47055=CARTESIAN_POINT('Ctrl Pts',(3.36868932900526,-8.25726212369374,108.156115939767));
#47056=CARTESIAN_POINT('Ctrl Pts',(3.27985014011025,-8.27702989768196,108.507740057355));
#47057=CARTESIAN_POINT('Ctrl Pts',(2.93670881513792,-8.29679767167018,108.625153653859));
#47058=CARTESIAN_POINT('Ctrl Pts',(2.70700175452616,-8.31269525746709,108.445417818528));
#47059=CARTESIAN_POINT('Ctrl Pts',(2.67795938726534,-8.32200358526793,108.294341749793));
#47060=CARTESIAN_POINT('Ctrl Pts',(2.67813962800902,-8.32472265507269,108.250144474503));
#47061=CARTESIAN_POINT('Ctrl Pts',(2.67813696047442,-8.22437734492731,108.250147181483));
#47062=CARTESIAN_POINT('Ctrl Pts',(2.67839924484375,-8.22825942822246,108.187046934739));
#47063=CARTESIAN_POINT('Ctrl Pts',(2.72675174382006,-8.23873076951369,108.016472328973));
#47064=CARTESIAN_POINT('Ctrl Pts',(3.00313671720263,-8.25579136880099,107.869557869052));
#47065=CARTESIAN_POINT('Ctrl Pts',(3.32052807796508,-8.2755591427892,108.045041942749));
#47066=CARTESIAN_POINT('Ctrl Pts',(3.34665292419479,-8.29532691677743,108.406773097638));
#47067=CARTESIAN_POINT('Ctrl Pts',(3.05777139212753,-8.31509469076565,108.626043242523));
#47068=CARTESIAN_POINT('Ctrl Pts',(2.74663073970376,-8.33311150014894,108.51444542395));
#47069=CARTESIAN_POINT('Ctrl Pts',(2.67847166361423,-8.34453905153616,108.328142551985));
#47070=CARTESIAN_POINT('Ctrl Pts',(2.67778811510267,-8.34937734492731,108.249714634396));
#47071=CARTESIAN_POINT('Origin',(3.,-7.51222265507269,108.25));
#47072=CARTESIAN_POINT('',(2.67768910651924,-8.07472265507269,108.249711575117));
#47073=CARTESIAN_POINT('',(2.67726599767135,-8.09937734492731,108.250159613763));
#47074=CARTESIAN_POINT('',(2.677725,-7.51222265507269,108.25));
#47075=CARTESIAN_POINT('Ctrl Pts',(2.67768910651924,-8.07472265507269,108.249711575117));
#47076=CARTESIAN_POINT('Ctrl Pts',(2.67746272185417,-8.07626582264838,108.224716705907));
#47077=CARTESIAN_POINT('Ctrl Pts',(2.6915048408805,-8.08439824822013,108.093246364532));
#47078=CARTESIAN_POINT('Ctrl Pts',(2.87152636194084,-8.09911993178797,107.891893084811));
#47079=CARTESIAN_POINT('Ctrl Pts',(3.22999816400173,-8.11888770577619,107.946937494892));
#47080=CARTESIAN_POINT('Ctrl Pts',(3.37946873571844,-8.13865547976441,108.277377307303));
#47081=CARTESIAN_POINT('Ctrl Pts',(3.18411292856613,-8.15842325375263,108.582939135017));
#47082=CARTESIAN_POINT('Ctrl Pts',(2.8214521816118,-8.17819102774085,108.585956417675));
#47083=CARTESIAN_POINT('Ctrl Pts',(2.68188274081524,-8.19195749484754,108.375453327707));
#47084=CARTESIAN_POINT('Ctrl Pts',(2.67721107470776,-8.19913470395815,108.259653500236));
#47085=CARTESIAN_POINT('Ctrl Pts',(2.67726984584404,-8.19972265507269,108.250162467927));
#47086=CARTESIAN_POINT('Ctrl Pts',(2.67726599767135,-8.09937734492731,108.250159613763));
#47087=CARTESIAN_POINT('Ctrl Pts',(2.67785842523723,-8.10539054691269,108.153094218703));
#47088=CARTESIAN_POINT('Ctrl Pts',(2.77594951876704,-8.11799300689414,107.94862624596));
#47089=CARTESIAN_POINT('Ctrl Pts',(3.12314338152363,-8.13718472487166,107.890025332106));
#47090=CARTESIAN_POINT('Ctrl Pts',(3.36885715962375,-8.15695249885988,108.156777417877));
#47091=CARTESIAN_POINT('Ctrl Pts',(3.27938738699594,-8.1767202728481,108.508241634873));
#47092=CARTESIAN_POINT('Ctrl Pts',(2.93603598591862,-8.19648804683633,108.625039543106));
#47093=CARTESIAN_POINT('Ctrl Pts',(2.70682331429706,-8.2123737375294,108.445026745081));
#47094=CARTESIAN_POINT('Ctrl Pts',(2.67795405620495,-8.22167017022639,108.294150202185));
#47095=CARTESIAN_POINT('Ctrl Pts',(2.67813696047442,-8.22437734492731,108.250147181483));
#47096=CARTESIAN_POINT('Origin',(3.,-7.51222265507269,108.25));
#47097=CARTESIAN_POINT('',(2.67817606009431,-7.94972265507269,108.250097623709));
#47098=CARTESIAN_POINT('',(2.67769484037528,-7.97437734492731,108.249711449058));
#47099=CARTESIAN_POINT('',(2.677725,-7.51222265507269,108.25));
#47100=CARTESIAN_POINT('Ctrl Pts',(2.67817606009431,-7.94972265507269,108.250097623709));
#47101=CARTESIAN_POINT('Ctrl Pts',(2.67833968674077,-7.9533969413386,108.190356954968));
#47102=CARTESIAN_POINT('Ctrl Pts',(2.7228778240257,-7.96366048560059,108.023254014987));
#47103=CARTESIAN_POINT('Ctrl Pts',(2.99121613241808,-7.98051328785865,107.869646268722));
#47104=CARTESIAN_POINT('Ctrl Pts',(3.31394930971311,-8.00028106184687,108.035100497677));
#47105=CARTESIAN_POINT('Ctrl Pts',(3.35139445931568,-8.02004883583509,108.395835495957));
#47106=CARTESIAN_POINT('Ctrl Pts',(3.0695244178543,-8.03981660982331,108.624048658391));
#47107=CARTESIAN_POINT('Ctrl Pts',(2.75141308756519,-8.05804121623585,108.521079574909));
#47108=CARTESIAN_POINT('Ctrl Pts',(2.67842937446406,-8.0696765646523,108.331443703284));
#47109=CARTESIAN_POINT('Ctrl Pts',(2.67768910651924,-8.07472265507269,108.249711575117));
#47110=CARTESIAN_POINT('Ctrl Pts',(2.67769484037528,-7.97437734492731,108.249711449058));
#47111=CARTESIAN_POINT('Ctrl Pts',(2.67746698787036,-7.97593240760684,108.224522765322));
#47112=CARTESIAN_POINT('Ctrl Pts',(2.69164072765528,-7.98407672828244,108.09285569702));
#47113=CARTESIAN_POINT('Ctrl Pts',(2.87216892550497,-7.99881030695412,107.891663181036));
#47114=CARTESIAN_POINT('Ctrl Pts',(3.23054141520414,-8.01857808094234,107.94735052791));
#47115=CARTESIAN_POINT('Ctrl Pts',(3.37941904127915,-8.03834585493056,108.278057929909));
#47116=CARTESIAN_POINT('Ctrl Pts',(3.18351543540106,-8.05811362891878,108.583268869327));
#47117=CARTESIAN_POINT('Ctrl Pts',(2.82084984167802,-8.07788140290699,108.585635627028));
#47118=CARTESIAN_POINT('Ctrl Pts',(2.68177847505825,-8.09163597490984,108.375064617705));
#47119=CARTESIAN_POINT('Ctrl Pts',(2.67720924397156,-8.09880128891661,108.259458337536));
#47120=CARTESIAN_POINT('Ctrl Pts',(2.67726599767135,-8.09937734492731,108.250159613763));
#47121=CARTESIAN_POINT('Origin',(3.,-7.51222265507269,108.25));
#47122=CARTESIAN_POINT('',(2.67736158403691,-7.82472265507269,108.25018840343));
#47123=CARTESIAN_POINT('',(2.6781760831613,-7.84937734492731,108.250099030543));
#47124=CARTESIAN_POINT('',(2.677725,-7.51222265507269,108.25));
#47125=CARTESIAN_POINT('Ctrl Pts',(2.67736158403691,-7.82472265507269,108.25018840343));
#47126=CARTESIAN_POINT('Ctrl Pts',(2.67807187286672,-7.83052806002883,108.156415124274));
#47127=CARTESIAN_POINT('Ctrl Pts',(2.77031473193814,-7.84292272298104,107.955065044056));
#47128=CARTESIAN_POINT('Ctrl Pts',(3.1118235245366,-7.86190664392932,107.886332436713));
#47129=CARTESIAN_POINT('Ctrl Pts',(3.3657465801897,-7.88167441791754,108.145272177939));
#47130=CARTESIAN_POINT('Ctrl Pts',(3.28734488563378,-7.90144219190576,108.499359232776));
#47131=CARTESIAN_POINT('Ctrl Pts',(2.94781550033985,-7.92120996589399,108.626860515219));
#47132=CARTESIAN_POINT('Ctrl Pts',(2.71000718921594,-7.93730345361629,108.451856374517));
#47133=CARTESIAN_POINT('Ctrl Pts',(2.67804624793102,-7.94680768334253,108.297492504759));
#47134=CARTESIAN_POINT('Ctrl Pts',(2.67817606009431,-7.94972265507269,108.250097623709));
#47135=CARTESIAN_POINT('Ctrl Pts',(2.6781760831613,-7.84937734492731,108.250099030543));
#47136=CARTESIAN_POINT('Ctrl Pts',(2.67834452920302,-7.85306352629706,108.190166386294));
#47137=CARTESIAN_POINT('Ctrl Pts',(2.72309291261354,-7.86333896566289,108.022867558002));
#47138=CARTESIAN_POINT('Ctrl Pts',(2.99189987276353,-7.88020366302479,107.869629820223));
#47139=CARTESIAN_POINT('Ctrl Pts',(3.31433362603907,-7.89997143701301,108.035664564453));
#47140=CARTESIAN_POINT('Ctrl Pts',(3.35113263206487,-7.91973921100123,108.396465308122));
#47141=CARTESIAN_POINT('Ctrl Pts',(3.06885322266343,-7.93950698498945,108.624172910368));
#47142=CARTESIAN_POINT('Ctrl Pts',(2.75113478560957,-7.95771969629815,108.520700790562));
#47143=CARTESIAN_POINT('Ctrl Pts',(2.67843246595669,-7.96934314961076,108.33125462758));
#47144=CARTESIAN_POINT('Ctrl Pts',(2.67769484037528,-7.97437734492731,108.249711449058));
#47145=CARTESIAN_POINT('Origin',(3.78136533198136,-11.25,107.59435663812));
#47146=CARTESIAN_POINT('',(3.78136533198136,-11.16,107.59435663812));
#47147=CARTESIAN_POINT('',(3.88624986816126,-11.,107.598416412742));
#47148=CARTESIAN_POINT('Ctrl Pts',(3.78136533198136,-11.16,107.59435663812));
#47149=CARTESIAN_POINT('Ctrl Pts',(3.83182864655857,-11.0851968149525,107.59630992591));
#47150=CARTESIAN_POINT('Ctrl Pts',(3.88624986816125,-11.,107.598416412742));
#47151=CARTESIAN_POINT('',(3.78136533198136,-9.9,107.59435663812));
#47152=CARTESIAN_POINT('',(3.78136533198136,-11.25,107.59435663812));
#47153=CARTESIAN_POINT('',(3.88624986816126,-9.9,107.598416412742));
#47154=CARTESIAN_POINT('',(3.78136533198136,-9.9,107.59435663812));
#47155=CARTESIAN_POINT('',(3.88624986816126,-10.4,107.598416412742));
#47156=CARTESIAN_POINT('Origin',(3.8715244580726,-9.9,107.508451031791));
#47157=CARTESIAN_POINT('',(3.79558024303105,-9.9,107.490360561254));
#47158=CARTESIAN_POINT('Origin',(3.,-9.9,108.25));
#47159=CARTESIAN_POINT('',(3.80580370973244,-9.9,107.415565831607));
#47160=CARTESIAN_POINT('Origin',(3.80580370973244,-11.25,107.415565831607));
#47161=CARTESIAN_POINT('',(3.79558024303105,-11.,107.490360561254));
#47162=CARTESIAN_POINT('Ctrl Pts',(3.79558024303106,-11.,107.490360561254));
#47163=CARTESIAN_POINT('Ctrl Pts',(3.78820458163732,-11.085196814953,107.544320789817));
#47164=CARTESIAN_POINT('Ctrl Pts',(3.78136533198136,-11.16,107.59435663812));
#47165=CARTESIAN_POINT('',(3.79558024303105,-10.4,107.490360561254));
#47166=CARTESIAN_POINT('Origin',(3.17712114122027,-11.25,107.245496091928));
#47167=CARTESIAN_POINT('',(3.17712114122027,-11.16,107.245496091928));
#47168=CARTESIAN_POINT('',(3.26007693015524,-11.,107.181187579413));
#47169=CARTESIAN_POINT('Ctrl Pts',(3.17712114122027,-11.16,107.245496091928));
#47170=CARTESIAN_POINT('Ctrl Pts',(3.21703383212295,-11.0851968149527,107.214555203831));
#47171=CARTESIAN_POINT('Ctrl Pts',(3.26007693015524,-11.,107.181187579413));
#47172=CARTESIAN_POINT('',(3.17712114122027,-9.9,107.245496091928));
#47173=CARTESIAN_POINT('',(3.17712114122027,-11.25,107.245496091928));
#47174=CARTESIAN_POINT('',(3.26007693015524,-9.9,107.181187579413));
#47175=CARTESIAN_POINT('',(3.17712114122027,-9.9,107.245496091928));
#47176=CARTESIAN_POINT('',(3.26007693015524,-10.4,107.181187579413));
#47177=CARTESIAN_POINT('Origin',(3.20032842114545,-9.9,107.169160896813));
#47178=CARTESIAN_POINT('',(3.12116300517389,-9.9,107.156693306443));
#47179=CARTESIAN_POINT('Origin',(3.,-9.9,108.25));
#47180=CARTESIAN_POINT('',(3.08091750954319,-9.9,107.092825701699));
#47181=CARTESIAN_POINT('Origin',(3.08091750954319,-11.25,107.092825701699));
#47182=CARTESIAN_POINT('',(3.12116300517389,-11.,107.156693306443));
#47183=CARTESIAN_POINT('Ctrl Pts',(3.12116300517389,-11.,107.156693306443));
#47184=CARTESIAN_POINT('Ctrl Pts',(3.15019788708483,-11.0851968149529,107.20277022344));
#47185=CARTESIAN_POINT('Ctrl Pts',(3.17712114122027,-11.16,107.245496091928));
#47186=CARTESIAN_POINT('',(3.12116300517389,-10.4,107.156693306443));
#47187=CARTESIAN_POINT('Origin',(2.49,-11.25,107.36665408814));
#47188=CARTESIAN_POINT('',(2.49,-11.16,107.36665408814));
#47189=CARTESIAN_POINT('',(2.51221110609647,-11.,107.264067956204));
#47190=CARTESIAN_POINT('Ctrl Pts',(2.49,-11.16,107.36665408814));
#47191=CARTESIAN_POINT('Ctrl Pts',(2.50068647557472,-11.0851968149526,107.317296609567));
#47192=CARTESIAN_POINT('Ctrl Pts',(2.51221110609647,-11.,107.264067956204));
#47193=CARTESIAN_POINT('',(2.49,-9.9,107.36665408814));
#47194=CARTESIAN_POINT('',(2.49,-11.25,107.36665408814));
#47195=CARTESIAN_POINT('',(2.51221110609646,-9.9,107.264067956204));
#47196=CARTESIAN_POINT('',(2.49,-9.9,107.36665408814));
#47197=CARTESIAN_POINT('',(2.51221110609647,-10.4,107.264067956204));
#47198=CARTESIAN_POINT('Origin',(2.4231773006864,-9.9,107.278470678637));
#47199=CARTESIAN_POINT('',(2.39005225061905,-9.9,107.334596404297));
#47200=CARTESIAN_POINT('Origin',(3.,-9.9,108.25));
#47201=CARTESIAN_POINT('',(2.31816910734073,-9.9,107.311540286525));
#47202=CARTESIAN_POINT('Origin',(2.31816910734073,-11.25,107.311540286525));
#47203=CARTESIAN_POINT('',(2.39005225061905,-11.,107.334596404297));
#47204=CARTESIAN_POINT('Ctrl Pts',(2.39005225061905,-11.,107.334596404297));
#47205=CARTESIAN_POINT('Ctrl Pts',(2.44191193190111,-11.0851968149519,107.351230108178));
#47206=CARTESIAN_POINT('Ctrl Pts',(2.49,-11.16,107.36665408814));
#47207=CARTESIAN_POINT('',(2.39005225061905,-10.4,107.334596404297));
#47208=CARTESIAN_POINT('Origin',(2.04151352679837,-11.25,107.901139453808));
#47209=CARTESIAN_POINT('',(2.04151352679837,-11.16,107.901139453808));
#47210=CARTESIAN_POINT('',(1.99258712666485,-11.,107.808276893701));
#47211=CARTESIAN_POINT('Ctrl Pts',(2.04151352679837,-11.16,107.901139453808));
#47212=CARTESIAN_POINT('Ctrl Pts',(2.01797346635675,-11.0851968149526,107.85646029753));
#47213=CARTESIAN_POINT('Ctrl Pts',(1.99258712666485,-11.,107.808276893701));
#47214=CARTESIAN_POINT('',(2.04151352679837,-9.9,107.901139453808));
#47215=CARTESIAN_POINT('',(2.04151352679837,-11.25,107.901139453808));
#47216=CARTESIAN_POINT('',(1.99258712666485,-9.9,107.808276893701));
#47217=CARTESIAN_POINT('',(2.04151352679837,-9.9,107.901139453808));
#47218=CARTESIAN_POINT('',(1.99258712666485,-10.4,107.808276893701));
#47219=CARTESIAN_POINT('Origin',(1.95798524215911,-9.9,107.855430035415));
#47220=CARTESIAN_POINT('',(1.94434282681371,-9.9,107.940827018159));
#47221=CARTESIAN_POINT('Origin',(3.,-9.9,108.25));
#47222=CARTESIAN_POINT('',(1.87445695751984,-9.9,107.969370601104));
#47223=CARTESIAN_POINT('Origin',(1.87445695751984,-11.25,107.969370601104));
#47224=CARTESIAN_POINT('',(1.94434282681371,-11.,107.940827018159));
#47225=CARTESIAN_POINT('Ctrl Pts',(1.94434282681371,-11.,107.940827018159));
#47226=CARTESIAN_POINT('Ctrl Pts',(1.99476158623952,-11.0851968149524,107.920234414015));
#47227=CARTESIAN_POINT('Ctrl Pts',(2.04151352679837,-11.16,107.901139453808));
#47228=CARTESIAN_POINT('',(1.94434282681371,-10.4,107.940827018159));
#47229=CARTESIAN_POINT('Origin',(4.02,-11.25,108.25));
#47230=CARTESIAN_POINT('',(4.02,-11.16,108.25));
#47231=CARTESIAN_POINT('',(4.09773664328448,-11.,108.320528448094));
#47232=CARTESIAN_POINT('Ctrl Pts',(4.02,-11.16,108.25));
#47233=CARTESIAN_POINT('Ctrl Pts',(4.05740159252348,-11.0851968149531,108.283933498611));
#47234=CARTESIAN_POINT('Ctrl Pts',(4.09773664328448,-11.,108.320528448094));
#47235=CARTESIAN_POINT('',(4.02,-9.9,108.25));
#47236=CARTESIAN_POINT('',(4.02,-11.25,108.25));
#47237=CARTESIAN_POINT('',(4.09773664328448,-9.9,108.320528448094));
#47238=CARTESIAN_POINT('',(4.02,-9.9,108.25));
#47239=CARTESIAN_POINT('',(4.09773664328448,-10.4,108.320528448094));
#47240=CARTESIAN_POINT('Origin',(4.0868226993136,-9.9,108.25));
#47241=CARTESIAN_POINT('',(4.09773664328448,-9.9,108.179471551906));
#47242=CARTESIAN_POINT('Origin',(3.,-9.9,108.25));
#47243=CARTESIAN_POINT('',(4.1536453986272,-9.9,108.12874698261));
#47244=CARTESIAN_POINT('Origin',(4.1536453986272,-11.25,108.12874698261));
#47245=CARTESIAN_POINT('',(4.09773664328448,-11.,108.179471551906));
#47246=CARTESIAN_POINT('Ctrl Pts',(4.09773664328448,-11.,108.179471551906));
#47247=CARTESIAN_POINT('Ctrl Pts',(4.05740159252348,-11.0851968149531,108.216066501389));
#47248=CARTESIAN_POINT('Ctrl Pts',(4.02,-11.16,108.25));
#47249=CARTESIAN_POINT('',(4.09773664328448,-10.4,108.179471551906));
#47250=CARTESIAN_POINT('Origin',(2.21863466801864,-11.25,108.90564336188));
#47251=CARTESIAN_POINT('',(2.21863466801864,-11.16,108.90564336188));
#47252=CARTESIAN_POINT('',(2.11375013183874,-11.,108.901583587258));
#47253=CARTESIAN_POINT('Ctrl Pts',(2.21863466801864,-11.16,108.90564336188));
#47254=CARTESIAN_POINT('Ctrl Pts',(2.16817135344143,-11.0851968149525,108.90369007409));
#47255=CARTESIAN_POINT('Ctrl Pts',(2.11375013183875,-11.,108.901583587258));
#47256=CARTESIAN_POINT('',(2.21863466801864,-9.9,108.90564336188));
#47257=CARTESIAN_POINT('',(2.21863466801864,-11.25,108.90564336188));
#47258=CARTESIAN_POINT('',(2.11375013183874,-9.9,108.901583587258));
#47259=CARTESIAN_POINT('',(2.21863466801864,-9.9,108.90564336188));
#47260=CARTESIAN_POINT('',(2.11375013183874,-10.4,108.901583587258));
#47261=CARTESIAN_POINT('Origin',(2.1284755419274,-9.9,108.991548968209));
#47262=CARTESIAN_POINT('',(2.20441975696894,-9.9,109.009639438746));
#47263=CARTESIAN_POINT('Origin',(3.,-9.9,108.25));
#47264=CARTESIAN_POINT('',(2.19419629026756,-9.9,109.084434168393));
#47265=CARTESIAN_POINT('Origin',(2.19419629026756,-11.25,109.084434168393));
#47266=CARTESIAN_POINT('',(2.20441975696894,-11.,109.009639438746));
#47267=CARTESIAN_POINT('Ctrl Pts',(2.20441975696894,-11.,109.009639438746));
#47268=CARTESIAN_POINT('Ctrl Pts',(2.21179541836267,-11.0851968149528,108.955679210184));
#47269=CARTESIAN_POINT('Ctrl Pts',(2.21863466801864,-11.16,108.90564336188));
#47270=CARTESIAN_POINT('',(2.20441975696894,-10.4,109.009639438746));
#47271=CARTESIAN_POINT('Origin',(2.82287885877973,-11.25,109.254503908072));
#47272=CARTESIAN_POINT('',(2.82287885877973,-11.16,109.254503908072));
#47273=CARTESIAN_POINT('',(2.73992306984476,-11.,109.318812420587));
#47274=CARTESIAN_POINT('Ctrl Pts',(2.82287885877973,-11.16,109.254503908072));
#47275=CARTESIAN_POINT('Ctrl Pts',(2.78296616787725,-11.0851968149531,109.285444796169));
#47276=CARTESIAN_POINT('Ctrl Pts',(2.73992306984476,-11.,109.318812420587));
#47277=CARTESIAN_POINT('',(2.82287885877973,-9.9,109.254503908072));
#47278=CARTESIAN_POINT('',(2.82287885877973,-11.25,109.254503908072));
#47279=CARTESIAN_POINT('',(2.73992306984476,-9.9,109.318812420587));
#47280=CARTESIAN_POINT('',(2.82287885877973,-9.9,109.254503908072));
#47281=CARTESIAN_POINT('',(2.73992306984476,-10.4,109.318812420587));
#47282=CARTESIAN_POINT('Origin',(2.79967157885455,-9.9,109.330839103187));
#47283=CARTESIAN_POINT('',(2.87883699482611,-9.9,109.343306693557));
#47284=CARTESIAN_POINT('Origin',(3.,-9.9,108.25));
#47285=CARTESIAN_POINT('',(2.91908249045681,-9.9,109.407174298301));
#47286=CARTESIAN_POINT('Origin',(2.91908249045681,-11.25,109.407174298301));
#47287=CARTESIAN_POINT('',(2.87883699482611,-11.,109.343306693557));
#47288=CARTESIAN_POINT('Ctrl Pts',(2.87883699482611,-11.,109.343306693557));
#47289=CARTESIAN_POINT('Ctrl Pts',(2.84980211291528,-11.0851968149526,109.29722977656));
#47290=CARTESIAN_POINT('Ctrl Pts',(2.82287885877973,-11.16,109.254503908072));
#47291=CARTESIAN_POINT('',(2.87883699482611,-10.4,109.343306693557));
#47292=CARTESIAN_POINT('Origin',(3.51,-11.25,109.13334591186));
#47293=CARTESIAN_POINT('',(3.51,-11.16,109.13334591186));
#47294=CARTESIAN_POINT('',(3.48778889390354,-11.,109.235932043796));
#47295=CARTESIAN_POINT('Ctrl Pts',(3.51,-11.16,109.13334591186));
#47296=CARTESIAN_POINT('Ctrl Pts',(3.49931352442526,-11.0851968149525,109.182703390433));
#47297=CARTESIAN_POINT('Ctrl Pts',(3.48778889390353,-11.,109.235932043796));
#47298=CARTESIAN_POINT('',(3.51,-9.9,109.13334591186));
#47299=CARTESIAN_POINT('',(3.51,-11.25,109.13334591186));
#47300=CARTESIAN_POINT('',(3.48778889390354,-9.9,109.235932043796));
#47301=CARTESIAN_POINT('',(3.51,-9.9,109.13334591186));
#47302=CARTESIAN_POINT('',(3.48778889390354,-10.4,109.235932043796));
#47303=CARTESIAN_POINT('Origin',(3.5768226993136,-9.9,109.221529321363));
#47304=CARTESIAN_POINT('',(3.60994774938095,-9.9,109.165403595703));
#47305=CARTESIAN_POINT('Origin',(3.,-9.9,108.25));
#47306=CARTESIAN_POINT('',(3.68183089265927,-9.9,109.188459713475));
#47307=CARTESIAN_POINT('Origin',(3.68183089265927,-11.25,109.188459713475));
#47308=CARTESIAN_POINT('',(3.60994774938095,-11.,109.165403595703));
#47309=CARTESIAN_POINT('Ctrl Pts',(3.60994774938095,-11.,109.165403595703));
#47310=CARTESIAN_POINT('Ctrl Pts',(3.55808806809889,-11.0851968149519,109.148769891822));
#47311=CARTESIAN_POINT('Ctrl Pts',(3.51,-11.16,109.13334591186));
#47312=CARTESIAN_POINT('',(3.60994774938095,-10.4,109.165403595703));
#47313=CARTESIAN_POINT('Origin',(3.95848647320163,-11.25,108.598860546192));
#47314=CARTESIAN_POINT('',(3.95848647320163,-11.16,108.598860546192));
#47315=CARTESIAN_POINT('',(4.00741287333515,-11.,108.691723106299));
#47316=CARTESIAN_POINT('Ctrl Pts',(3.95848647320162,-11.16,108.598860546192));
#47317=CARTESIAN_POINT('Ctrl Pts',(3.98202653364333,-11.0851968149524,108.64353970247));
#47318=CARTESIAN_POINT('Ctrl Pts',(4.00741287333515,-11.,108.691723106299));
#47319=CARTESIAN_POINT('',(3.95848647320163,-9.9,108.598860546192));
#47320=CARTESIAN_POINT('',(3.95848647320163,-11.25,108.598860546192));
#47321=CARTESIAN_POINT('',(4.00741287333515,-9.9,108.691723106299));
#47322=CARTESIAN_POINT('',(3.95848647320163,-9.9,108.598860546192));
#47323=CARTESIAN_POINT('',(4.00741287333515,-10.4,108.691723106299));
#47324=CARTESIAN_POINT('Origin',(4.04201475784089,-9.9,108.644569964585));
#47325=CARTESIAN_POINT('',(4.05565717318629,-9.9,108.559172981841));
#47326=CARTESIAN_POINT('Origin',(3.,-9.9,108.25));
#47327=CARTESIAN_POINT('',(4.12554304248016,-9.9,108.530629398896));
#47328=CARTESIAN_POINT('Origin',(4.12554304248016,-11.25,108.530629398896));
#47329=CARTESIAN_POINT('',(4.05565717318629,-11.,108.559172981841));
#47330=CARTESIAN_POINT('Ctrl Pts',(4.05565717318629,-11.,108.559172981841));
#47331=CARTESIAN_POINT('Ctrl Pts',(4.00523841376048,-11.0851968149523,108.579765585985));
#47332=CARTESIAN_POINT('Ctrl Pts',(3.95848647320163,-11.16,108.598860546192));
#47333=CARTESIAN_POINT('',(4.05565717318629,-10.4,108.559172981841));
#47334=CARTESIAN_POINT('Origin',(3.78136533198136,-11.25,108.90564336188));
#47335=CARTESIAN_POINT('',(3.78136533198136,-11.16,108.90564336188));
#47336=CARTESIAN_POINT('',(3.79558024303105,-11.,109.009639438746));
#47337=CARTESIAN_POINT('Ctrl Pts',(3.78136533198136,-11.16,108.90564336188));
#47338=CARTESIAN_POINT('Ctrl Pts',(3.78820458163732,-11.085196814953,108.955679210183));
#47339=CARTESIAN_POINT('Ctrl Pts',(3.79558024303106,-11.,109.009639438746));
#47340=CARTESIAN_POINT('',(3.78136533198136,-9.9,108.90564336188));
#47341=CARTESIAN_POINT('',(3.78136533198136,-11.25,108.90564336188));
#47342=CARTESIAN_POINT('',(3.79558024303105,-9.9,109.009639438746));
#47343=CARTESIAN_POINT('',(3.78136533198136,-9.9,108.90564336188));
#47344=CARTESIAN_POINT('',(3.79558024303105,-10.4,109.009639438746));
#47345=CARTESIAN_POINT('Origin',(3.8715244580726,-9.9,108.991548968209));
#47346=CARTESIAN_POINT('',(3.88624986816126,-9.9,108.901583587258));
#47347=CARTESIAN_POINT('Origin',(3.,-9.9,108.25));
#47348=CARTESIAN_POINT('',(3.96168358416385,-9.9,108.898663768026));
#47349=CARTESIAN_POINT('Origin',(3.96168358416385,-11.25,108.898663768026));
#47350=CARTESIAN_POINT('',(3.88624986816126,-11.,108.901583587258));
#47351=CARTESIAN_POINT('Ctrl Pts',(3.88624986816126,-11.,108.901583587258));
#47352=CARTESIAN_POINT('Ctrl Pts',(3.83182864655864,-11.0851968149524,108.90369007409));
#47353=CARTESIAN_POINT('Ctrl Pts',(3.78136533198136,-11.16,108.90564336188));
#47354=CARTESIAN_POINT('',(3.88624986816126,-10.4,108.901583587258));
#47355=CARTESIAN_POINT('Origin',(3.17712114122027,-11.25,109.254503908072));
#47356=CARTESIAN_POINT('',(3.17712114122027,-11.16,109.254503908072));
#47357=CARTESIAN_POINT('',(3.12116300517389,-11.,109.343306693557));
#47358=CARTESIAN_POINT('Ctrl Pts',(3.17712114122027,-11.16,109.254503908072));
#47359=CARTESIAN_POINT('Ctrl Pts',(3.15019788708492,-11.0851968149532,109.29722977656));
#47360=CARTESIAN_POINT('Ctrl Pts',(3.12116300517389,-11.,109.343306693557));
#47361=CARTESIAN_POINT('',(3.17712114122027,-9.9,109.254503908072));
#47362=CARTESIAN_POINT('',(3.17712114122027,-11.25,109.254503908072));
#47363=CARTESIAN_POINT('',(3.12116300517389,-9.9,109.343306693557));
#47364=CARTESIAN_POINT('',(3.17712114122027,-9.9,109.254503908072));
#47365=CARTESIAN_POINT('',(3.12116300517389,-10.4,109.343306693557));
#47366=CARTESIAN_POINT('Origin',(3.20032842114545,-9.9,109.330839103187));
#47367=CARTESIAN_POINT('',(3.26007693015523,-9.9,109.318812420587));
#47368=CARTESIAN_POINT('Origin',(3.,-9.9,108.25));
#47369=CARTESIAN_POINT('',(3.31973933274772,-9.9,109.365063567288));
#47370=CARTESIAN_POINT('Origin',(3.31973933274772,-11.25,109.365063567288));
#47371=CARTESIAN_POINT('',(3.26007693015523,-11.,109.318812420587));
#47372=CARTESIAN_POINT('Ctrl Pts',(3.26007693015523,-11.,109.318812420587));
#47373=CARTESIAN_POINT('Ctrl Pts',(3.2170338321225,-11.0851968149535,109.285444796169));
#47374=CARTESIAN_POINT('Ctrl Pts',(3.17712114122027,-11.16,109.254503908072));
#47375=CARTESIAN_POINT('',(3.26007693015523,-10.4,109.318812420587));
#47376=CARTESIAN_POINT('Origin',(2.49,-11.25,109.13334591186));
#47377=CARTESIAN_POINT('',(2.49,-11.16,109.13334591186));
#47378=CARTESIAN_POINT('',(2.39005225061905,-11.,109.165403595703));
#47379=CARTESIAN_POINT('Ctrl Pts',(2.49,-11.16,109.13334591186));
#47380=CARTESIAN_POINT('Ctrl Pts',(2.4419119319011,-11.0851968149518,109.148769891822));
#47381=CARTESIAN_POINT('Ctrl Pts',(2.39005225061905,-11.,109.165403595703));
#47382=CARTESIAN_POINT('',(2.49,-9.9,109.13334591186));
#47383=CARTESIAN_POINT('',(2.49,-11.25,109.13334591186));
#47384=CARTESIAN_POINT('',(2.39005225061905,-9.9,109.165403595703));
#47385=CARTESIAN_POINT('',(2.49,-9.9,109.13334591186));
#47386=CARTESIAN_POINT('',(2.39005225061905,-10.4,109.165403595703));
#47387=CARTESIAN_POINT('Origin',(2.4231773006864,-9.9,109.221529321363));
#47388=CARTESIAN_POINT('',(2.51221110609646,-9.9,109.235932043796));
#47389=CARTESIAN_POINT('Origin',(3.,-9.9,108.25));
#47390=CARTESIAN_POINT('',(2.52818549403207,-9.9,109.309712730865));
#47391=CARTESIAN_POINT('Origin',(2.52818549403207,-11.25,109.309712730865));
#47392=CARTESIAN_POINT('',(2.51221110609646,-11.,109.235932043796));
#47393=CARTESIAN_POINT('Ctrl Pts',(2.51221110609647,-11.,109.235932043796));
#47394=CARTESIAN_POINT('Ctrl Pts',(2.5006864755747,-11.0851968149528,109.182703390433));
#47395=CARTESIAN_POINT('Ctrl Pts',(2.49,-11.16,109.13334591186));
#47396=CARTESIAN_POINT('',(2.51221110609646,-10.4,109.235932043796));
#47397=CARTESIAN_POINT('Origin',(2.04151352679837,-11.25,108.598860546192));
#47398=CARTESIAN_POINT('',(2.04151352679837,-11.16,108.598860546192));
#47399=CARTESIAN_POINT('',(1.94434282681371,-11.,108.559172981841));
#47400=CARTESIAN_POINT('Ctrl Pts',(2.04151352679837,-11.16,108.598860546192));
#47401=CARTESIAN_POINT('Ctrl Pts',(1.99476158623951,-11.0851968149523,108.579765585985));
#47402=CARTESIAN_POINT('Ctrl Pts',(1.94434282681371,-11.,108.559172981841));
#47403=CARTESIAN_POINT('',(2.04151352679837,-9.9,108.598860546192));
#47404=CARTESIAN_POINT('',(2.04151352679837,-11.25,108.598860546192));
#47405=CARTESIAN_POINT('',(1.94434282681371,-9.9,108.559172981841));
#47406=CARTESIAN_POINT('',(2.04151352679837,-9.9,108.598860546192));
#47407=CARTESIAN_POINT('',(1.94434282681371,-10.4,108.559172981841));
#47408=CARTESIAN_POINT('Origin',(1.95798524215911,-9.9,108.644569964585));
#47409=CARTESIAN_POINT('',(1.99258712666485,-9.9,108.691723106299));
#47410=CARTESIAN_POINT('Origin',(3.,-9.9,108.25));
#47411=CARTESIAN_POINT('',(1.95739890629297,-9.9,108.758510530275));
#47412=CARTESIAN_POINT('Origin',(1.95739890629297,-11.25,108.758510530275));
#47413=CARTESIAN_POINT('',(1.99258712666485,-11.,108.691723106299));
#47414=CARTESIAN_POINT('Ctrl Pts',(1.99258712666485,-11.,108.691723106299));
#47415=CARTESIAN_POINT('Ctrl Pts',(2.01797346635666,-11.0851968149523,108.64353970247));
#47416=CARTESIAN_POINT('Ctrl Pts',(2.04151352679837,-11.16,108.598860546192));
#47417=CARTESIAN_POINT('',(1.99258712666485,-10.4,108.691723106299));
#47418=CARTESIAN_POINT('Origin',(1.98,-11.25,108.25));
#47419=CARTESIAN_POINT('',(1.98,-11.16,108.25));
#47420=CARTESIAN_POINT('',(1.90226335671552,-11.,108.179471551906));
#47421=CARTESIAN_POINT('Ctrl Pts',(1.98,-11.16,108.25));
#47422=CARTESIAN_POINT('Ctrl Pts',(1.94259840747653,-11.0851968149531,108.216066501389));
#47423=CARTESIAN_POINT('Ctrl Pts',(1.90226335671552,-11.,108.179471551906));
#47424=CARTESIAN_POINT('',(1.98,-9.9,108.25));
#47425=CARTESIAN_POINT('',(1.98,-11.25,108.25));
#47426=CARTESIAN_POINT('',(1.90226335671552,-9.9,108.179471551906));
#47427=CARTESIAN_POINT('',(1.98,-9.9,108.25));
#47428=CARTESIAN_POINT('',(1.90226335671552,-10.4,108.179471551906));
#47429=CARTESIAN_POINT('Origin',(1.9131773006864,-9.9,108.25));
#47430=CARTESIAN_POINT('',(1.9,-9.9,108.25));
#47431=CARTESIAN_POINT('Origin',(3.,-9.9,108.25));
#47432=CARTESIAN_POINT('',(1.90226335671552,-9.9,108.320528448094));
#47433=CARTESIAN_POINT('',(1.8463546013728,-9.9,108.37125301739));
#47434=CARTESIAN_POINT('Origin',(3.,-9.9,108.25));
#47435=CARTESIAN_POINT('Origin',(1.8463546013728,-11.25,108.37125301739));
#47436=CARTESIAN_POINT('',(1.90226335671552,-11.,108.320528448094));
#47437=CARTESIAN_POINT('Ctrl Pts',(1.90226335671552,-11.,108.320528448094));
#47438=CARTESIAN_POINT('Ctrl Pts',(1.94259840747628,-11.0851968149526,108.283933498611));
#47439=CARTESIAN_POINT('Ctrl Pts',(1.98,-11.16,108.25));
#47440=CARTESIAN_POINT('',(1.90226335671552,-10.4,108.320528448094));
#47441=CARTESIAN_POINT('Origin',(2.21863466801864,-11.25,107.59435663812));
#47442=CARTESIAN_POINT('',(2.21863466801864,-11.16,107.59435663812));
#47443=CARTESIAN_POINT('',(2.20441975696895,-11.,107.490360561254));
#47444=CARTESIAN_POINT('Ctrl Pts',(2.21863466801864,-11.16,107.59435663812));
#47445=CARTESIAN_POINT('Ctrl Pts',(2.21179541836268,-11.085196814953,107.544320789817));
#47446=CARTESIAN_POINT('Ctrl Pts',(2.20441975696894,-11.,107.490360561254));
#47447=CARTESIAN_POINT('',(2.21863466801864,-9.9,107.59435663812));
#47448=CARTESIAN_POINT('',(2.21863466801864,-11.25,107.59435663812));
#47449=CARTESIAN_POINT('',(2.20441975696895,-9.9,107.490360561254));
#47450=CARTESIAN_POINT('',(2.21863466801864,-9.9,107.59435663812));
#47451=CARTESIAN_POINT('',(2.20441975696895,-10.4,107.490360561254));
#47452=CARTESIAN_POINT('Origin',(2.1284755419274,-9.9,107.508451031791));
#47453=CARTESIAN_POINT('',(2.11375013183874,-9.9,107.598416412742));
#47454=CARTESIAN_POINT('Origin',(3.,-9.9,108.25));
#47455=CARTESIAN_POINT('',(2.03831641583615,-9.9,107.601336231974));
#47456=CARTESIAN_POINT('Origin',(2.03831641583615,-11.25,107.601336231974));
#47457=CARTESIAN_POINT('',(2.11375013183874,-11.,107.598416412742));
#47458=CARTESIAN_POINT('Ctrl Pts',(2.11375013183874,-11.,107.598416412742));
#47459=CARTESIAN_POINT('Ctrl Pts',(2.16817135344136,-11.0851968149524,107.59630992591));
#47460=CARTESIAN_POINT('Ctrl Pts',(2.21863466801864,-11.16,107.59435663812));
#47461=CARTESIAN_POINT('',(2.11375013183874,-10.4,107.598416412742));
#47462=CARTESIAN_POINT('Origin',(2.82287885877973,-11.25,107.245496091928));
#47463=CARTESIAN_POINT('',(2.82287885877973,-11.16,107.245496091928));
#47464=CARTESIAN_POINT('',(2.87883699482611,-11.,107.156693306443));
#47465=CARTESIAN_POINT('Ctrl Pts',(2.82287885877973,-11.16,107.245496091928));
#47466=CARTESIAN_POINT('Ctrl Pts',(2.84980211291508,-11.0851968149532,107.20277022344));
#47467=CARTESIAN_POINT('Ctrl Pts',(2.87883699482611,-11.,107.156693306443));
#47468=CARTESIAN_POINT('',(2.82287885877973,-9.9,107.245496091928));
#47469=CARTESIAN_POINT('',(2.82287885877973,-11.25,107.245496091928));
#47470=CARTESIAN_POINT('',(2.87883699482611,-9.9,107.156693306443));
#47471=CARTESIAN_POINT('',(2.82287885877973,-9.9,107.245496091928));
#47472=CARTESIAN_POINT('',(2.87883699482611,-10.4,107.156693306443));
#47473=CARTESIAN_POINT('Origin',(2.79967157885455,-9.9,107.169160896813));
#47474=CARTESIAN_POINT('',(2.73992306984477,-9.9,107.181187579413));
#47475=CARTESIAN_POINT('Origin',(3.,-9.9,108.25));
#47476=CARTESIAN_POINT('',(2.68026066725228,-9.9,107.134936432712));
#47477=CARTESIAN_POINT('Origin',(2.68026066725228,-11.25,107.134936432712));
#47478=CARTESIAN_POINT('',(2.73992306984477,-11.,107.181187579413));
#47479=CARTESIAN_POINT('Ctrl Pts',(2.73992306984477,-11.,107.181187579413));
#47480=CARTESIAN_POINT('Ctrl Pts',(2.7829661678775,-11.0851968149535,107.214555203831));
#47481=CARTESIAN_POINT('Ctrl Pts',(2.82287885877973,-11.16,107.245496091928));
#47482=CARTESIAN_POINT('',(2.73992306984477,-10.4,107.181187579413));
#47483=CARTESIAN_POINT('Origin',(3.51,-11.25,107.36665408814));
#47484=CARTESIAN_POINT('',(3.51,-11.16,107.36665408814));
#47485=CARTESIAN_POINT('',(3.60994774938095,-11.,107.334596404297));
#47486=CARTESIAN_POINT('Ctrl Pts',(3.51,-11.16,107.36665408814));
#47487=CARTESIAN_POINT('Ctrl Pts',(3.55808806809884,-11.0851968149519,107.351230108178));
#47488=CARTESIAN_POINT('Ctrl Pts',(3.60994774938095,-11.,107.334596404297));
#47489=CARTESIAN_POINT('',(3.51,-9.9,107.36665408814));
#47490=CARTESIAN_POINT('',(3.51,-11.25,107.36665408814));
#47491=CARTESIAN_POINT('',(3.60994774938095,-9.9,107.334596404297));
#47492=CARTESIAN_POINT('',(3.51,-9.9,107.36665408814));
#47493=CARTESIAN_POINT('',(3.60994774938095,-10.4,107.334596404297));
#47494=CARTESIAN_POINT('Origin',(3.5768226993136,-9.9,107.278470678637));
#47495=CARTESIAN_POINT('',(3.48778889390353,-9.9,107.264067956204));
#47496=CARTESIAN_POINT('Origin',(3.,-9.9,108.25));
#47497=CARTESIAN_POINT('',(3.47181450596793,-9.9,107.190287269135));
#47498=CARTESIAN_POINT('Origin',(3.47181450596793,-11.25,107.190287269135));
#47499=CARTESIAN_POINT('',(3.48778889390353,-11.,107.264067956204));
#47500=CARTESIAN_POINT('Ctrl Pts',(3.48778889390353,-11.,107.264067956204));
#47501=CARTESIAN_POINT('Ctrl Pts',(3.49931352442529,-11.0851968149527,107.317296609567));
#47502=CARTESIAN_POINT('Ctrl Pts',(3.51,-11.16,107.36665408814));
#47503=CARTESIAN_POINT('',(3.48778889390353,-10.4,107.264067956204));
#47504=CARTESIAN_POINT('Origin',(3.95848647320163,-11.25,107.901139453808));
#47505=CARTESIAN_POINT('',(3.95848647320163,-11.16,107.901139453808));
#47506=CARTESIAN_POINT('',(4.05565717318629,-11.,107.940827018159));
#47507=CARTESIAN_POINT('Ctrl Pts',(3.95848647320163,-11.16,107.901139453808));
#47508=CARTESIAN_POINT('Ctrl Pts',(4.00523841376049,-11.0851968149523,107.920234414015));
#47509=CARTESIAN_POINT('Ctrl Pts',(4.05565717318629,-11.,107.940827018159));
#47510=CARTESIAN_POINT('',(3.95848647320163,-9.9,107.901139453808));
#47511=CARTESIAN_POINT('',(3.95848647320163,-11.25,107.901139453808));
#47512=CARTESIAN_POINT('',(4.05565717318629,-9.9,107.940827018159));
#47513=CARTESIAN_POINT('',(3.95848647320163,-9.9,107.901139453808));
#47514=CARTESIAN_POINT('',(4.05565717318629,-10.4,107.940827018159));
#47515=CARTESIAN_POINT('Origin',(4.04201475784089,-9.9,107.855430035415));
#47516=CARTESIAN_POINT('',(4.00741287333515,-9.9,107.808276893701));
#47517=CARTESIAN_POINT('Origin',(3.,-9.9,108.25));
#47518=CARTESIAN_POINT('',(4.04260109370703,-9.9,107.741489469725));
#47519=CARTESIAN_POINT('Origin',(4.04260109370703,-11.25,107.741489469725));
#47520=CARTESIAN_POINT('',(4.00741287333515,-11.,107.808276893701));
#47521=CARTESIAN_POINT('Ctrl Pts',(4.00741287333515,-11.,107.808276893701));
#47522=CARTESIAN_POINT('Ctrl Pts',(3.98202653364324,-11.0851968149526,107.85646029753));
#47523=CARTESIAN_POINT('Ctrl Pts',(3.95848647320163,-11.16,107.901139453808));
#47524=CARTESIAN_POINT('',(4.00741287333515,-10.4,107.808276893701));
#47525=CARTESIAN_POINT('Origin',(3.,-10.4,108.25));
#47526=CARTESIAN_POINT('Origin',(3.,-11.,108.25));
#47527=CARTESIAN_POINT('Origin',(3.,-11.,108.25));
#47528=CARTESIAN_POINT('Origin',(3.,-11.,108.25));
#47529=CARTESIAN_POINT('Origin',(3.,-11.,108.25));
#47530=CARTESIAN_POINT('Origin',(3.,-11.,108.25));
#47531=CARTESIAN_POINT('Origin',(3.,-11.,108.25));
#47532=CARTESIAN_POINT('Origin',(3.,-11.,108.25));
#47533=CARTESIAN_POINT('',(1.9,-9.8,108.25));
#47534=CARTESIAN_POINT('',(1.9,-10.4,108.25));
#47535=CARTESIAN_POINT('Origin',(3.,-9.8,108.25));
#47536=CARTESIAN_POINT('Origin',(3.,-11.,108.25));
#47537=CARTESIAN_POINT('Origin',(3.,-11.,108.25));
#47538=CARTESIAN_POINT('Origin',(3.,-11.,108.25));
#47539=CARTESIAN_POINT('Origin',(3.,-11.,108.25));
#47540=CARTESIAN_POINT('Origin',(3.,-11.,108.25));
#47541=CARTESIAN_POINT('Origin',(3.,-11.,108.25));
#47542=CARTESIAN_POINT('Origin',(3.,-11.,108.25));
#47543=CARTESIAN_POINT('Origin',(3.,-11.,108.25));
#47544=CARTESIAN_POINT('Origin',(3.,-11.,108.25));
#47545=CARTESIAN_POINT('Origin',(3.,-11.,108.25));
#47546=CARTESIAN_POINT('Origin',(3.,-11.,108.25));
#47547=CARTESIAN_POINT('Ctrl Pts',(2.85670976047873,-7.7022936971308,108.538667772505));
#47548=CARTESIAN_POINT('Ctrl Pts',(2.80890461182963,-7.70558832612884,108.514938032462));
#47549=CARTESIAN_POINT('Ctrl Pts',(2.72581310601332,-7.71217758412491,108.443301532936));
#47550=CARTESIAN_POINT('Ctrl Pts',(2.64543880465911,-7.72535610011706,108.237507022022));
#47551=CARTESIAN_POINT('Ctrl Pts',(2.75646225010103,-7.74182924510724,107.957765662282));
#47552=CARTESIAN_POINT('Ctrl Pts',(3.11264948697861,-7.76159701909547,107.88639744465));
#47553=CARTESIAN_POINT('Ctrl Pts',(3.36586763099966,-7.78136479308369,108.145991153067));
#47554=CARTESIAN_POINT('Ctrl Pts',(3.2869314131236,-7.80113256707191,108.499845495719));
#47555=CARTESIAN_POINT('Ctrl Pts',(2.9471249283031,-7.82090034106013,108.626779562835));
#47556=CARTESIAN_POINT('Ctrl Pts',(2.65543060635616,-7.84066811504835,108.411277484445));
#47557=CARTESIAN_POINT('Ctrl Pts',(2.67682067977961,-7.86043588903657,108.049245789717));
#47558=CARTESIAN_POINT('Ctrl Pts',(2.99189987276353,-7.88020366302479,107.869629820223));
#47559=CARTESIAN_POINT('Ctrl Pts',(3.31433362603907,-7.89997143701301,108.035664564453));
#47560=CARTESIAN_POINT('Ctrl Pts',(3.35113263206487,-7.91973921100123,108.396465308122));
#47561=CARTESIAN_POINT('Ctrl Pts',(3.06885322266343,-7.93950698498945,108.624172910368));
#47562=CARTESIAN_POINT('Ctrl Pts',(2.72400691454818,-7.95927475897767,108.511865992208));
#47563=CARTESIAN_POINT('Ctrl Pts',(2.62995753252861,-7.9790425329659,108.161599513052));
#47564=CARTESIAN_POINT('Ctrl Pts',(2.87216892550497,-7.99881030695412,107.891663181036));
#47565=CARTESIAN_POINT('Ctrl Pts',(3.23054141520414,-8.01857808094234,107.94735052791));
#47566=CARTESIAN_POINT('Ctrl Pts',(3.37941904127915,-8.03834585493056,108.278057929909));
#47567=CARTESIAN_POINT('Ctrl Pts',(3.18351543540106,-8.05811362891878,108.583268869327));
#47568=CARTESIAN_POINT('Ctrl Pts',(2.82084984167802,-8.07788140290699,108.585635627028));
#47569=CARTESIAN_POINT('Ctrl Pts',(2.62097947544604,-8.09764917689522,108.283007517633));
#47570=CARTESIAN_POINT('Ctrl Pts',(2.7655281947484,-8.11741695088344,107.950385203063));
#47571=CARTESIAN_POINT('Ctrl Pts',(3.12314338152363,-8.13718472487166,107.890025332106));
#47572=CARTESIAN_POINT('Ctrl Pts',(3.36885715962375,-8.15695249885988,108.156777417877));
#47573=CARTESIAN_POINT('Ctrl Pts',(3.27938738699594,-8.1767202728481,108.508241634873));
#47574=CARTESIAN_POINT('Ctrl Pts',(2.93603598591862,-8.19648804683633,108.625039543106));
#47575=CARTESIAN_POINT('Ctrl Pts',(2.65080921325911,-8.21625582082455,108.401035917761));
#47576=CARTESIAN_POINT('Ctrl Pts',(2.68289499558652,-8.23602359481276,108.039784705191));
#47577=CARTESIAN_POINT('Ctrl Pts',(3.00313671720263,-8.25579136880099,107.869557869052));
#47578=CARTESIAN_POINT('Ctrl Pts',(3.32052807796508,-8.2755591427892,108.045041942749));
#47579=CARTESIAN_POINT('Ctrl Pts',(3.34665292419479,-8.29532691677743,108.406773097638));
#47580=CARTESIAN_POINT('Ctrl Pts',(3.05777139212753,-8.31509469076565,108.626043242523));
#47581=CARTESIAN_POINT('Ctrl Pts',(2.71639251838735,-8.33486246475387,108.503599783851));
#47582=CARTESIAN_POINT('Ctrl Pts',(2.63273010801875,-8.35463023874209,108.150708104863));
#47583=CARTESIAN_POINT('Ctrl Pts',(2.88280888503356,-8.37439801273031,107.888043791918));
#47584=CARTESIAN_POINT('Ctrl Pts',(3.23938019713941,-8.39416578671853,107.954292077865));
#47585=CARTESIAN_POINT('Ctrl Pts',(3.37842474494008,-8.41393356070675,108.289252597531));
#47586=CARTESIAN_POINT('Ctrl Pts',(3.17359159824674,-8.43370133469497,108.588543957285));
#47587=CARTESIAN_POINT('Ctrl Pts',(2.81101433099364,-8.45346910868319,108.580197624016));
#47588=CARTESIAN_POINT('Ctrl Pts',(2.62016990367575,-8.47323688267142,108.271797979773));
#47589=CARTESIAN_POINT('Ctrl Pts',(2.77448022527394,-8.49300465665964,107.943590331087));
#47590=CARTESIAN_POINT('Ctrl Pts',(3.1337222307341,-8.51277243064786,107.893819681898));
#47591=CARTESIAN_POINT('Ctrl Pts',(3.37144973952803,-8.53254020463607,108.167713032621));
#47592=CARTESIAN_POINT('Ctrl Pts',(3.27163779891431,-8.5523079786243,108.51638123094));
#47593=CARTESIAN_POINT('Ctrl Pts',(2.92498634456088,-8.57207575261252,108.622986602298));
#47594=CARTESIAN_POINT('Ctrl Pts',(2.6465004191082,-8.59184352660074,108.390655964343));
#47595=CARTESIAN_POINT('Ctrl Pts',(2.68924248550083,-8.61161130058896,108.030510088664));
#47596=CARTESIAN_POINT('Ctrl Pts',(3.01437247462189,-8.63137907457718,107.869816510131));
#47597=CARTESIAN_POINT('Ctrl Pts',(3.32644207722428,-8.6511468485654,108.05459881215));
#47598=CARTESIAN_POINT('Ctrl Pts',(3.34187106527198,-8.67091462255362,108.41694378912));
#47599=CARTESIAN_POINT('Ctrl Pts',(3.04663898976117,-8.69068239654184,108.627585564647));
#47600=CARTESIAN_POINT('Ctrl Pts',(2.70902567864924,-8.71045017053006,108.495112215751));
#47601=CARTESIAN_POINT('Ctrl Pts',(2.63582313908689,-8.73021794451829,108.139903369846));
#47602=CARTESIAN_POINT('Ctrl Pts',(2.89355112400359,-8.7499857185065,107.884740242026));
#47603=CARTESIAN_POINT('Ctrl Pts',(3.2480100826438,-8.76975349249473,107.961491676198));
#47604=CARTESIAN_POINT('Ctrl Pts',(3.37710022867022,-8.78952126648294,108.300413009558));
#47605=CARTESIAN_POINT('Ctrl Pts',(3.16351627908797,-8.80928904047117,108.593523624325));
#47606=CARTESIAN_POINT('Ctrl Pts',(2.80134373476698,-8.82905681445938,108.574471481458));
#47607=CARTESIAN_POINT('Ctrl Pts',(2.6196917811276,-8.84882458844761,108.260569420702));
#47608=CARTESIAN_POINT('Ctrl Pts',(2.78362905031687,-8.86859236243583,107.937062839968));
#47609=CARTESIAN_POINT('Ctrl Pts',(3.14418439041029,-8.88836013642405,107.897924843879));
#47610=CARTESIAN_POINT('Ctrl Pts',(3.37371818283995,-8.90812791041227,108.178720453069));
#47611=CARTESIAN_POINT('Ctrl Pts',(3.26365117266921,-8.9278956844005,108.524288375886));
#47612=CARTESIAN_POINT('Ctrl Pts',(2.91400216206011,-8.94766345838871,108.620608183754));
#47613=CARTESIAN_POINT('Ctrl Pts',(2.64250009780596,-8.96743123237694,108.380153270904));
#47614=CARTESIAN_POINT('Ctrl Pts',(2.69586115043873,-8.98719900636515,108.021427004694));
#47615=CARTESIAN_POINT('Ctrl Pts',(3.02559569024832,-9.00696678035338,107.87040690913));
#47616=CARTESIAN_POINT('Ctrl Pts',(3.332071214708,-9.02673455434159,108.064326193666));
#47617=CARTESIAN_POINT('Ctrl Pts',(3.33679088083925,-9.04650232832982,108.426968801146));
#47618=CARTESIAN_POINT('Ctrl Pts',(3.03546588901117,-9.06627010231804,108.628798395868));
#47619=CARTESIAN_POINT('Ctrl Pts',(2.70191275060503,-9.08603787630626,108.486410756411));
#47620=CARTESIAN_POINT('Ctrl Pts',(2.63923396028456,-9.10580565029448,108.129194707984));
#47621=CARTESIAN_POINT('Ctrl Pts',(2.90438625299112,-9.1255734242827,107.881755427227));
#47622=CARTESIAN_POINT('Ctrl Pts',(3.2564235481909,-9.14534119827092,107.968943034321));
#47623=CARTESIAN_POINT('Ctrl Pts',(3.37544664493324,-9.16510897225914,108.311529429926));
#47624=CARTESIAN_POINT('Ctrl Pts',(3.15329827158403,-9.18487674624737,108.59820352372));
#47625=CARTESIAN_POINT('Ctrl Pts',(2.79184649073512,-9.20464452023558,108.568462196868));
#47626=CARTESIAN_POINT('Ctrl Pts',(2.61954552618002,-9.22441229422381,108.249331638151));
#47627=CARTESIAN_POINT('Ctrl Pts',(2.7929666844032,-9.24418006821203,107.930808426606));
#47628=CARTESIAN_POINT('Ctrl Pts',(3.15452073504689,-9.26394784220025,107.902337234153));
#47629=CARTESIAN_POINT('Ctrl Pts',(3.37566050136972,-9.28371561618847,108.1897900773));
#47630=CARTESIAN_POINT('Ctrl Pts',(3.25543449645413,-9.30348339017669,108.531956162289));
#47631=CARTESIAN_POINT('Ctrl Pts',(2.90309298249399,-9.32325116416491,108.617906379101));
#47632=CARTESIAN_POINT('Ctrl Pts',(2.63881182940184,-9.34301893815313,108.369536967137));
#47633=CARTESIAN_POINT('Ctrl Pts',(2.70274502066785,-9.36278671214135,108.012543455793));
#47634=CARTESIAN_POINT('Ctrl Pts',(3.03679699339086,-9.38255448612957,107.871328383607));
#47635=CARTESIAN_POINT('Ctrl Pts',(3.3374096596431,-9.40232226011779,108.074215959287));
#47636=CARTESIAN_POINT('Ctrl Pts',(3.33141880989063,-9.42209003410602,108.436838588562));
#47637=CARTESIAN_POINT('Ctrl Pts',(3.0242574980433,-9.44185780809423,108.629682366924));
#47638=CARTESIAN_POINT('Ctrl Pts',(2.69506947405166,-9.46162558208246,108.477499161251));
#47639=CARTESIAN_POINT('Ctrl Pts',(2.64293914677449,-9.48139335607067,108.11859924174));
#47640=CARTESIAN_POINT('Ctrl Pts',(2.91535037624978,-9.50116113005889,107.879072987278));
#47641=CARTESIAN_POINT('Ctrl Pts',(3.26451785003709,-9.52092890404712,107.976673691963));
#47642=CARTESIAN_POINT('Ctrl Pts',(3.37368648223413,-9.54069667803533,108.322492331795));
#47643=CARTESIAN_POINT('Ctrl Pts',(3.1425103302508,-9.56046445202356,108.602707172509));
#47644=CARTESIAN_POINT('Ctrl Pts',(2.84350450152926,-9.57693759701374,108.568400494187));
#47645=CARTESIAN_POINT('Ctrl Pts',(2.70009555898594,-9.59011611300589,108.400337160175));
#47646=CARTESIAN_POINT('Ctrl Pts',(2.67621270542783,-9.59670537100196,108.293259638215));
#47647=CARTESIAN_POINT('Ctrl Pts',(2.67788283232033,-9.6,108.239915065145));
#47648=CARTESIAN_POINT('Ctrl Pts',(2.84618335780813,-7.71596246475387,108.559873914818));
#47649=CARTESIAN_POINT('Ctrl Pts',(2.79486634229295,-7.71925709375191,108.534400938113));
#47650=CARTESIAN_POINT('Ctrl Pts',(2.7056707595231,-7.72584635174798,108.457501870512));
#47651=CARTESIAN_POINT('Ctrl Pts',(2.61939199277579,-7.73902486774013,108.236589261557));
#47652=CARTESIAN_POINT('Ctrl Pts',(2.73857145426251,-7.75549801273031,107.936297512579));
#47653=CARTESIAN_POINT('Ctrl Pts',(3.12092495545807,-7.77526578671853,107.859686435425));
#47654=CARTESIAN_POINT('Ctrl Pts',(3.39274503745041,-7.79503356070675,108.138350444197));
#47655=CARTESIAN_POINT('Ctrl Pts',(3.30800999882123,-7.81480133469497,108.518199671845));
#47656=CARTESIAN_POINT('Ctrl Pts',(2.94324061421599,-7.8345691086832,108.654458582772));
#47657=CARTESIAN_POINT('Ctrl Pts',(2.6301178132617,-7.85433688267141,108.423125267997));
#47658=CARTESIAN_POINT('Ctrl Pts',(2.65307924651231,-7.87410465665964,108.034497962773));
#47659=CARTESIAN_POINT('Ctrl Pts',(2.99130482036317,-7.89387243064785,107.841687026006));
#47660=CARTESIAN_POINT('Ctrl Pts',(3.33742523598857,-7.91364020463608,108.019919032108));
#47661=CARTESIAN_POINT('Ctrl Pts',(3.37692757447162,-7.9334079786243,108.407224958017));
#47662=CARTESIAN_POINT('Ctrl Pts',(3.07391132536006,-7.95317575261252,108.651660440127));
#47663=CARTESIAN_POINT('Ctrl Pts',(2.70373188143028,-7.97294352660074,108.531103219314));
#47664=CARTESIAN_POINT('Ctrl Pts',(2.60277343380117,-7.99271130058896,108.155105427167));
#47665=CARTESIAN_POINT('Ctrl Pts',(2.86277818564407,-8.01247907457718,107.865339003892));
#47666=CARTESIAN_POINT('Ctrl Pts',(3.2474774729342,-8.0322468485654,107.925117260508));
#47667=CARTESIAN_POINT('Ctrl Pts',(3.40729196285943,-8.05201462255362,108.280119124511));
#47668=CARTESIAN_POINT('Ctrl Pts',(3.1969968656489,-8.07178239654184,108.607751502113));
#47669=CARTESIAN_POINT('Ctrl Pts',(2.80768909387483,-8.09155017053006,108.610292126818));
#47670=CARTESIAN_POINT('Ctrl Pts',(2.59313582974341,-8.11131794451828,108.28543231937));
#47671=CARTESIAN_POINT('Ctrl Pts',(2.74830340229062,-8.13108571850651,107.928374869287));
#47672=CARTESIAN_POINT('Ctrl Pts',(3.13218975358964,-8.15085349249472,107.863580835131));
#47673=CARTESIAN_POINT('Ctrl Pts',(3.39595418314122,-8.17062126648295,108.149929090729));
#47674=CARTESIAN_POINT('Ctrl Pts',(3.29991177265145,-8.19038904047117,108.527212609058));
#47675=CARTESIAN_POINT('Ctrl Pts',(2.9313370547779,-8.21015681445939,108.652590737531));
#47676=CARTESIAN_POINT('Ctrl Pts',(2.62515692289811,-8.22992458844761,108.412131334263));
#47677=CARTESIAN_POINT('Ctrl Pts',(2.65959979434693,-8.24969236243583,108.024341847059));
#47678=CARTESIAN_POINT('Ctrl Pts',(3.0033671470522,-8.26946013642405,107.84160978915));
#47679=CARTESIAN_POINT('Ctrl Pts',(3.34407474539452,-8.28922791041227,108.029985292356));
#47680=CARTESIAN_POINT('Ctrl Pts',(3.37211877783007,-8.30899568440049,108.418289979452));
#47681=CARTESIAN_POINT('Ctrl Pts',(3.06201540022193,-8.32876345838871,108.65366817082));
#47682=CARTESIAN_POINT('Ctrl Pts',(2.69555811569654,-8.34853123237693,108.522229757888));
#47683=CARTESIAN_POINT('Ctrl Pts',(2.60574968852405,-8.36829900636515,108.143413913202));
#47684=CARTESIAN_POINT('Ctrl Pts',(2.87419977900041,-8.38806678035338,107.86145372683));
#47685=CARTESIAN_POINT('Ctrl Pts',(3.25696557039913,-8.4078345543416,107.932568751338));
#47686=CARTESIAN_POINT('Ctrl Pts',(3.40622462341796,-8.42760232832982,108.292136175986));
#47687=CARTESIAN_POINT('Ctrl Pts',(3.18634400252412,-8.44737010231804,108.613414109139));
#47688=CARTESIAN_POINT('Ctrl Pts',(2.79713104586844,-8.46713787630626,108.604454636657));
#47689=CARTESIAN_POINT('Ctrl Pts',(2.59226678512645,-8.48690565029448,108.273399305259));
#47690=CARTESIAN_POINT('Ctrl Pts',(2.75791306782568,-8.5066734242827,107.921080831711));
#47691=CARTESIAN_POINT('Ctrl Pts',(3.14354574733523,-8.52644119827092,107.867653925848));
#47692=CARTESIAN_POINT('Ctrl Pts',(3.39873721942354,-8.54620897225914,108.161668058755));
#47693=CARTESIAN_POINT('Ctrl Pts',(3.29159288351379,-8.56597674624736,108.535950156989));
#47694=CARTESIAN_POINT('Ctrl Pts',(2.91947568350271,-8.58574452023558,108.650386983368));
#47695=CARTESIAN_POINT('Ctrl Pts',(2.62053159565738,-8.6055122942238,108.400988847613));
#47696=CARTESIAN_POINT('Ctrl Pts',(2.666413584234,-8.62528006821202,108.014385897676));
#47697=CARTESIAN_POINT('Ctrl Pts',(3.01542830686663,-8.64504784220025,107.841887430548));
#47698=CARTESIAN_POINT('Ctrl Pts',(3.35042319949031,-8.66481561618847,108.040244229503));
#47699=CARTESIAN_POINT('Ctrl Pts',(3.36698563348334,-8.68458339017668,108.429207831343));
#47700=CARTESIAN_POINT('Ctrl Pts',(3.05006518814019,-8.70435116416491,108.655323795174));
#47701=CARTESIAN_POINT('Ctrl Pts',(2.68765009240153,-8.72411893815312,108.513118675166));
#47702=CARTESIAN_POINT('Ctrl Pts',(2.60906994016635,-8.74388671214136,108.131815439603));
#47703=CARTESIAN_POINT('Ctrl Pts',(2.8857311654613,-8.76365448612956,107.857907491208));
#47704=CARTESIAN_POINT('Ctrl Pts',(3.26622942546156,-8.78342226011779,107.940297247322));
#47705=CARTESIAN_POINT('Ctrl Pts',(3.40480280539435,-8.80319003410601,108.304116455377));
#47706=CARTESIAN_POINT('Ctrl Pts',(3.17552852920793,-8.82295780809423,108.618759593003));
#47707=CARTESIAN_POINT('Ctrl Pts',(2.78675002728303,-8.84272558208245,108.59830783961));
#47708=CARTESIAN_POINT('Ctrl Pts',(2.5917535386893,-8.86249335607067,108.261345872599));
#47709=CARTESIAN_POINT('Ctrl Pts',(2.76773398481769,-8.8822611300589,107.914073817351));
#47710=CARTESIAN_POINT('Ctrl Pts',(3.15477647928768,-8.90202890404711,107.87206066167));
#47711=CARTESIAN_POINT('Ctrl Pts',(3.40117230735701,-8.92179667803534,108.173484107483));
#47712=CARTESIAN_POINT('Ctrl Pts',(3.28301954289012,-8.94156445202356,108.54443817745));
#47713=CARTESIAN_POINT('Ctrl Pts',(2.90768457982995,-8.96133222601178,108.647833841191));
#47714=CARTESIAN_POINT('Ctrl Pts',(2.61623740233022,-8.98109999999999,108.389714604203));
#47715=CARTESIAN_POINT('Ctrl Pts',(2.67351847023281,-9.00086777398822,108.004635551233));
#47716=CARTESIAN_POINT('Ctrl Pts',(3.02747600354171,-9.02063554797644,107.8425212015));
#47717=CARTESIAN_POINT('Ctrl Pts',(3.35646586526486,-9.04040332196466,108.050686204945));
#47718=CARTESIAN_POINT('Ctrl Pts',(3.36153224800663,-9.06017109595288,108.439969301858));
#47719=CARTESIAN_POINT('Ctrl Pts',(3.03807128788586,-9.0799388699411,108.65662572353));
#47720=CARTESIAN_POINT('Ctrl Pts',(2.68001463368803,-9.09970664392932,108.503777988303));
#47721=CARTESIAN_POINT('Ctrl Pts',(2.61273132747015,-9.11947441791754,108.120320096896));
#47722=CARTESIAN_POINT('Ctrl Pts',(2.89736226583594,-9.13924219190577,107.854703405629));
#47723=CARTESIAN_POINT('Ctrl Pts',(3.27526096190099,-9.15900996589399,107.948295997901));
#47724=CARTESIAN_POINT('Ctrl Pts',(3.40302774591469,-9.17877773988221,108.316049511389));
#47725=CARTESIAN_POINT('Ctrl Pts',(3.16455988536032,-9.19854551387043,108.623783287661));
#47726=CARTESIAN_POINT('Ctrl Pts',(2.77655509570962,-9.21831328785865,108.591857100323));
#47727=CARTESIAN_POINT('Ctrl Pts',(2.59159653954535,-9.23808106184686,108.249282538883));
#47728=CARTESIAN_POINT('Ctrl Pts',(2.77775758116294,-9.25784883583509,107.907359941616));
#47729=CARTESIAN_POINT('Ctrl Pts',(3.16587215356286,-9.27761660982331,107.876797195424));
#47730=CARTESIAN_POINT('Ctrl Pts',(3.40325731269523,-9.29738438381153,108.185366929616));
#47731=CARTESIAN_POINT('Ctrl Pts',(3.27419925234135,-9.31715215779975,108.552669255586));
#47732=CARTESIAN_POINT('Ctrl Pts',(2.89597398896532,-9.33691993178797,108.644933556279));
#47733=CARTESIAN_POINT('Ctrl Pts',(2.61227818596405,-9.3566877057762,108.37831840441));
#47734=CARTESIAN_POINT('Ctrl Pts',(2.68090804406188,-9.37645547976442,107.995099398128));
#47735=CARTESIAN_POINT('Ctrl Pts',(3.03950017799571,-9.39622325375263,107.843510369433));
#47736=CARTESIAN_POINT('Ctrl Pts',(3.36219648360416,-9.41599102774086,108.06130249357));
#47737=CARTESIAN_POINT('Ctrl Pts',(3.35576553341607,-9.43575880172908,108.450564144638));
#47738=CARTESIAN_POINT('Ctrl Pts',(3.02603950491996,-9.4555265757173,108.657574632961));
#47739=CARTESIAN_POINT('Ctrl Pts',(2.67266863563159,-9.47529434970552,108.4942117286));
#47740=CARTESIAN_POINT('Ctrl Pts',(2.61670870476033,-9.49506212369374,108.108946265394));
#47741=CARTESIAN_POINT('Ctrl Pts',(2.90913183667244,-9.51482989768196,107.851823907994));
#47742=CARTESIAN_POINT('Ctrl Pts',(3.28394988820209,-9.53459767167018,107.956594565928));
#47743=CARTESIAN_POINT('Ctrl Pts',(3.40113827795794,-9.5543654456584,108.32781777111));
#47744=CARTESIAN_POINT('Ctrl Pts',(3.15297943914441,-9.57413321964662,108.628617783972));
#47745=CARTESIAN_POINT('Ctrl Pts',(2.83200801273462,-9.59060636463681,108.591790864833));
#47746=CARTESIAN_POINT('Ctrl Pts',(2.67806394734679,-9.60378488062895,108.411381244473));
#47747=CARTESIAN_POINT('Ctrl Pts',(2.65242660908466,-9.61037413862503,108.296437582315));
#47748=CARTESIAN_POINT('Ctrl Pts',(2.65421942701488,-9.61366876762306,108.239174204598));
#47749=CARTESIAN_POINT('Ctrl Pts',(2.83565695513754,-7.72963123237693,108.581080057132));
#47750=CARTESIAN_POINT('Ctrl Pts',(2.78082807275627,-7.73292586137497,108.553863843763));
#47751=CARTESIAN_POINT('Ctrl Pts',(2.68552841303288,-7.73951511937104,108.471702208088));
#47752=CARTESIAN_POINT('Ctrl Pts',(2.59334518089247,-7.75269363536319,108.235671501093));
#47753=CARTESIAN_POINT('Ctrl Pts',(2.72068065842399,-7.76916678035337,107.914829362876));
#47754=CARTESIAN_POINT('Ctrl Pts',(3.12920042393753,-7.78893455434159,107.832975426201));
#47755=CARTESIAN_POINT('Ctrl Pts',(3.41962244390117,-7.80870232832982,108.130709735327));
#47756=CARTESIAN_POINT('Ctrl Pts',(3.32908858451885,-7.82847010231803,108.536553847972));
#47757=CARTESIAN_POINT('Ctrl Pts',(2.93935630012888,-7.84823787630626,108.682137602709));
#47758=CARTESIAN_POINT('Ctrl Pts',(2.60480502016724,-7.86800565029448,108.434973051549));
#47759=CARTESIAN_POINT('Ctrl Pts',(2.62933781324501,-7.8877734242827,108.019750135828));
#47760=CARTESIAN_POINT('Ctrl Pts',(2.99070976796282,-7.90754119827092,107.813744231789));
#47761=CARTESIAN_POINT('Ctrl Pts',(3.36051684593806,-7.92730897225914,108.004173499763));
#47762=CARTESIAN_POINT('Ctrl Pts',(3.40272251687838,-7.94707674624736,108.417984607911));
#47763=CARTESIAN_POINT('Ctrl Pts',(3.07896942805669,-7.96684452023559,108.679147969885));
#47764=CARTESIAN_POINT('Ctrl Pts',(2.68345684831238,-7.9866122942238,108.55034044642));
#47765=CARTESIAN_POINT('Ctrl Pts',(2.57558933507373,-8.00638006821202,108.148611341282));
#47766=CARTESIAN_POINT('Ctrl Pts',(2.85338744578317,-8.02614784220024,107.839014826749));
#47767=CARTESIAN_POINT('Ctrl Pts',(3.26441353066427,-8.04591561618847,107.902883993107));
#47768=CARTESIAN_POINT('Ctrl Pts',(3.43516488443971,-8.06568339017668,108.282180319114));
#47769=CARTESIAN_POINT('Ctrl Pts',(3.21047829589673,-8.08545116416491,108.6322341349));
#47770=CARTESIAN_POINT('Ctrl Pts',(2.79452834607165,-8.10521893815313,108.634948626608));
#47771=CARTESIAN_POINT('Ctrl Pts',(2.56529218404078,-8.12498671214135,108.287857121108));
#47772=CARTESIAN_POINT('Ctrl Pts',(2.73107860983284,-8.14475448612956,107.906364535512));
#47773=CARTESIAN_POINT('Ctrl Pts',(3.14123612565564,-8.16452226011779,107.837136338157));
#47774=CARTESIAN_POINT('Ctrl Pts',(3.42305120665869,-8.18429003410601,108.14308076358));
#47775=CARTESIAN_POINT('Ctrl Pts',(3.32043615830696,-8.20405780809423,108.546183583244));
#47776=CARTESIAN_POINT('Ctrl Pts',(2.92663812363718,-8.22382558208245,108.680141931955));
#47777=CARTESIAN_POINT('Ctrl Pts',(2.59950463253712,-8.24359335607067,108.423226750764));
#47778=CARTESIAN_POINT('Ctrl Pts',(2.63630459310734,-8.26336113005889,108.008898988927));
#47779=CARTESIAN_POINT('Ctrl Pts',(3.00359757690178,-8.28312890404712,107.813661709249));
#47780=CARTESIAN_POINT('Ctrl Pts',(3.36762141282396,-8.30289667803533,108.014928641963));
#47781=CARTESIAN_POINT('Ctrl Pts',(3.39758463146536,-8.32266445202356,108.429806861266));
#47782=CARTESIAN_POINT('Ctrl Pts',(3.06625940831632,-8.34243222601178,108.681293099116));
#47783=CARTESIAN_POINT('Ctrl Pts',(2.67472371300574,-8.3622,108.540859731924));
#47784=CARTESIAN_POINT('Ctrl Pts',(2.57876926902934,-8.38196777398822,108.136119721542));
#47785=CARTESIAN_POINT('Ctrl Pts',(2.86559067296727,-8.40173554797644,107.834863661742));
#47786=CARTESIAN_POINT('Ctrl Pts',(3.27455094365884,-8.42150332196466,107.910845424811));
#47787=CARTESIAN_POINT('Ctrl Pts',(3.43402450189583,-8.44127109595287,108.29501975444));
#47788=CARTESIAN_POINT('Ctrl Pts',(3.1990964068015,-8.4610388699411,108.638284260993));
#47789=CARTESIAN_POINT('Ctrl Pts',(2.78324776074323,-8.48080664392932,108.628711649297));
#47790=CARTESIAN_POINT('Ctrl Pts',(2.56436366657715,-8.50057441791754,108.275000630746));
#47791=CARTESIAN_POINT('Ctrl Pts',(2.74134591037741,-8.52034219190576,107.898571332334));
#47792=CARTESIAN_POINT('Ctrl Pts',(3.15336926393636,-8.54010996589398,107.841488169797));
#47793=CARTESIAN_POINT('Ctrl Pts',(3.42602469931906,-8.55987773988221,108.155623084889));
#47794=CARTESIAN_POINT('Ctrl Pts',(3.31154796811327,-8.57964551387043,108.555519083038));
#47795=CARTESIAN_POINT('Ctrl Pts',(2.91396502244455,-8.59941328785865,108.677787364438));
#47796=CARTESIAN_POINT('Ctrl Pts',(2.59456277220656,-8.61918106184687,108.411321730883));
#47797=CARTESIAN_POINT('Ctrl Pts',(2.64358468296716,-8.63894883583509,107.998261706687));
#47798=CARTESIAN_POINT('Ctrl Pts',(3.01648413911137,-8.65871660982331,107.813958350965));
#47799=CARTESIAN_POINT('Ctrl Pts',(3.37440432175633,-8.67848438381153,108.025889646857));
#47800=CARTESIAN_POINT('Ctrl Pts',(3.39210020169469,-8.69825215779975,108.441471873566));
#47801=CARTESIAN_POINT('Ctrl Pts',(3.0534913865192,-8.71801993178797,108.683062025701));
#47802=CARTESIAN_POINT('Ctrl Pts',(2.66627450615383,-8.73778770577619,108.531125134581));
#47803=CARTESIAN_POINT('Ctrl Pts',(2.5823167412458,-8.75755547976442,108.123727509361));
#47804=CARTESIAN_POINT('Ctrl Pts',(2.87791120691902,-8.77732325375263,107.831074740389));
#47805=CARTESIAN_POINT('Ctrl Pts',(3.28444876827931,-8.79709102774086,107.919102818446));
#47806=CARTESIAN_POINT('Ctrl Pts',(3.43250538211848,-8.81685880172908,108.307819901196));
#47807=CARTESIAN_POINT('Ctrl Pts',(3.18754077932788,-8.8366265757173,108.643995561682));
#47808=CARTESIAN_POINT('Ctrl Pts',(2.77215631979907,-8.85639434970551,108.622144197762));
#47809=CARTESIAN_POINT('Ctrl Pts',(2.563815296251,-8.87616212369374,108.262122324496));
#47810=CARTESIAN_POINT('Ctrl Pts',(2.7518389193185,-8.89592989768196,107.891084794735));
#47811=CARTESIAN_POINT('Ctrl Pts',(3.16536856816508,-8.91569767167018,107.846196479462));
#47812=CARTESIAN_POINT('Ctrl Pts',(3.42862643187407,-8.9354654456584,108.168247761898));
#47813=CARTESIAN_POINT('Ctrl Pts',(3.30238791311104,-8.95523321964662,108.564587979014));
#47814=CARTESIAN_POINT('Ctrl Pts',(2.90136699759978,-8.97500099363484,108.675059498627));
#47815=CARTESIAN_POINT('Ctrl Pts',(2.58997470685448,-8.99476876762306,108.399275937501));
#47816=CARTESIAN_POINT('Ctrl Pts',(2.65117579002688,-9.01453654161128,107.987844097773));
#47817=CARTESIAN_POINT('Ctrl Pts',(3.02935631683511,-9.0343043155995,107.81463549387));
#47818=CARTESIAN_POINT('Ctrl Pts',(3.38086051582172,-9.05407208958773,108.037046216225));
#47819=CARTESIAN_POINT('Ctrl Pts',(3.38627361517402,-9.07383986357594,108.452969802571));
#47820=CARTESIAN_POINT('Ctrl Pts',(3.04067668676055,-9.09360763756417,108.684453051191));
#47821=CARTESIAN_POINT('Ctrl Pts',(2.65811651677103,-9.11337541155238,108.521145220195));
#47822=CARTESIAN_POINT('Ctrl Pts',(2.58622869465574,-9.13314318554061,108.111445485808));
#47823=CARTESIAN_POINT('Ctrl Pts',(2.89033827868075,-9.15291095952883,107.827651384031));
#47824=CARTESIAN_POINT('Ctrl Pts',(3.29409837561108,-9.17267873351704,107.92764896148));
#47825=CARTESIAN_POINT('Ctrl Pts',(3.43060884689613,-9.19244650750527,108.320569592852));
#47826=CARTESIAN_POINT('Ctrl Pts',(3.17582149913661,-9.21221428149349,108.649363051602));
#47827=CARTESIAN_POINT('Ctrl Pts',(2.76126370068411,-9.23198205548171,108.615252003778));
#47828=CARTESIAN_POINT('Ctrl Pts',(2.56364755291068,-9.25174982946993,108.249233439614));
#47829=CARTESIAN_POINT('Ctrl Pts',(2.76254847792268,-9.27151760345816,107.883911456626));
#47830=CARTESIAN_POINT('Ctrl Pts',(3.17722357207883,-9.29128537744637,107.851257156695));
#47831=CARTESIAN_POINT('Ctrl Pts',(3.43085412402073,-9.3110531514346,108.180943781931));
#47832=CARTESIAN_POINT('Ctrl Pts',(3.29296400822856,-9.33082092542282,108.573382348883));
#47833=CARTESIAN_POINT('Ctrl Pts',(2.88885499543664,-9.35058869941104,108.671960733458));
#47834=CARTESIAN_POINT('Ctrl Pts',(2.58574454252627,-9.37035647339926,108.387099841682));
#47835=CARTESIAN_POINT('Ctrl Pts',(2.65907106745591,-9.39012424738748,107.977655340462));
#47836=CARTESIAN_POINT('Ctrl Pts',(3.04220336260056,-9.4098920213757,107.815692355258));
#47837=CARTESIAN_POINT('Ctrl Pts',(3.38698330756522,-9.42965979536392,108.048389027853));
#47838=CARTESIAN_POINT('Ctrl Pts',(3.38011225694151,-9.44942756935214,108.464289700713));
#47839=CARTESIAN_POINT('Ctrl Pts',(3.02782151179663,-9.46919534334036,108.685466898997));
#47840=CARTESIAN_POINT('Ctrl Pts',(2.65026779721153,-9.48896311732858,108.51092429595));
#47841=CARTESIAN_POINT('Ctrl Pts',(2.59047826274616,-9.5087308913168,108.099293289049));
#47842=CARTESIAN_POINT('Ctrl Pts',(2.9029132970951,-9.52849866530502,107.82457482871));
#47843=CARTESIAN_POINT('Ctrl Pts',(3.3033819263671,-9.54826643929324,107.936515439893));
#47844=CARTESIAN_POINT('Ctrl Pts',(3.42859007368176,-9.56803421328147,108.333143210425));
#47845=CARTESIAN_POINT('Ctrl Pts',(3.16344854803802,-9.58780198726968,108.654528395435));
#47846=CARTESIAN_POINT('Ctrl Pts',(2.82051152393997,-9.60427513225987,108.615181235479));
#47847=CARTESIAN_POINT('Ctrl Pts',(2.65603233570764,-9.61745364825201,108.422425328771));
#47848=CARTESIAN_POINT('Ctrl Pts',(2.62864051274149,-9.62404290624809,108.299615526415));
#47849=CARTESIAN_POINT('Ctrl Pts',(2.63055602170942,-9.62733753524613,108.238433344052));
#47850=CARTESIAN_POINT('Ctrl Pts',(2.82513055246694,-7.7433,108.602286199445));
#47851=CARTESIAN_POINT('Ctrl Pts',(2.7667898032196,-7.74659462899803,108.573326749414));
#47852=CARTESIAN_POINT('Ctrl Pts',(2.66538606654267,-7.75318388699411,108.485902545664));
#47853=CARTESIAN_POINT('Ctrl Pts',(2.56729836900916,-7.76636240298626,108.234753740629));
#47854=CARTESIAN_POINT('Ctrl Pts',(2.70278986258547,-7.78283554797643,107.893361213173));
#47855=CARTESIAN_POINT('Ctrl Pts',(3.13747589241699,-7.80260332196466,107.806264416976));
#47856=CARTESIAN_POINT('Ctrl Pts',(3.44649985035192,-7.82237109595288,108.123069026457));
#47857=CARTESIAN_POINT('Ctrl Pts',(3.35016717021648,-7.8421388699411,108.554908024098));
#47858=CARTESIAN_POINT('Ctrl Pts',(2.93547198604177,-7.86190664392932,108.709816622646));
#47859=CARTESIAN_POINT('Ctrl Pts',(2.57949222707278,-7.88167441791754,108.446820835101));
#47860=CARTESIAN_POINT('Ctrl Pts',(2.60559637997771,-7.90144219190577,108.005002308884));
#47861=CARTESIAN_POINT('Ctrl Pts',(2.99011471556246,-7.92120996589398,107.785801437572));
#47862=CARTESIAN_POINT('Ctrl Pts',(3.38360845588756,-7.94097773988221,107.988427967418));
#47863=CARTESIAN_POINT('Ctrl Pts',(3.42851745928513,-7.96074551387042,108.428744257806));
#47864=CARTESIAN_POINT('Ctrl Pts',(3.08402753075333,-7.98051328785865,108.706635499644));
#47865=CARTESIAN_POINT('Ctrl Pts',(2.66318181519447,-8.00028106184687,108.569577673526));
#47866=CARTESIAN_POINT('Ctrl Pts',(2.54840523634629,-8.02004883583509,108.142117255398));
#47867=CARTESIAN_POINT('Ctrl Pts',(2.84399670592228,-8.03981660982331,107.812690649605));
#47868=CARTESIAN_POINT('Ctrl Pts',(3.28134958839434,-8.05958438381153,107.880650725706));
#47869=CARTESIAN_POINT('Ctrl Pts',(3.46303780601998,-8.07935215779975,108.284241513717));
#47870=CARTESIAN_POINT('Ctrl Pts',(3.22395972614457,-8.09911993178797,108.656716767687));
#47871=CARTESIAN_POINT('Ctrl Pts',(2.78136759826846,-8.11888770577619,108.659605126398));
#47872=CARTESIAN_POINT('Ctrl Pts',(2.53744853833815,-8.13865547976441,108.290281922845));
#47873=CARTESIAN_POINT('Ctrl Pts',(2.71385381737505,-8.15842325375263,107.884354201737));
#47874=CARTESIAN_POINT('Ctrl Pts',(3.15028249772165,-8.17819102774086,107.810691841183));
#47875=CARTESIAN_POINT('Ctrl Pts',(3.45014823017616,-8.19795880172907,108.136232436432));
#47876=CARTESIAN_POINT('Ctrl Pts',(3.34096054396247,-8.2177265757173,108.565154557429));
#47877=CARTESIAN_POINT('Ctrl Pts',(2.92193919249646,-8.23749434970552,108.707693126379));
#47878=CARTESIAN_POINT('Ctrl Pts',(2.57385234217612,-8.25726212369374,108.434322167266));
#47879=CARTESIAN_POINT('Ctrl Pts',(2.61300939186774,-8.27702989768196,107.993456130795));
#47880=CARTESIAN_POINT('Ctrl Pts',(3.00382800675135,-8.29679767167018,107.785713629347));
#47881=CARTESIAN_POINT('Ctrl Pts',(3.3911680802534,-8.3165654456584,107.99987199157));
#47882=CARTESIAN_POINT('Ctrl Pts',(3.42305048510065,-8.33633321964662,108.44132374308));
#47883=CARTESIAN_POINT('Ctrl Pts',(3.07050341641071,-8.35610099363484,108.708918027413));
#47884=CARTESIAN_POINT('Ctrl Pts',(2.65388931031493,-8.37586876762306,108.559489705961));
#47885=CARTESIAN_POINT('Ctrl Pts',(2.55178884953464,-8.39563654161128,108.128825529881));
#47886=CARTESIAN_POINT('Ctrl Pts',(2.85698156693412,-8.4154043155995,107.808273596653));
#47887=CARTESIAN_POINT('Ctrl Pts',(3.29213631691856,-8.43517208958772,107.889122098284));
#47888=CARTESIAN_POINT('Ctrl Pts',(3.4618243803737,-8.45493986357594,108.297903332895));
#47889=CARTESIAN_POINT('Ctrl Pts',(3.21184881107887,-8.47470763756417,108.663154412846));
#47890=CARTESIAN_POINT('Ctrl Pts',(2.76936447561803,-8.49447541155238,108.652968661937));
#47891=CARTESIAN_POINT('Ctrl Pts',(2.53646054802784,-8.51424318554061,108.276601956232));
#47892=CARTESIAN_POINT('Ctrl Pts',(2.72477875292914,-8.53401095952883,107.876061832958));
#47893=CARTESIAN_POINT('Ctrl Pts',(3.16319278053749,-8.55377873351705,107.815322413747));
#47894=CARTESIAN_POINT('Ctrl Pts',(3.45331217921457,-8.57354650750527,108.149578111023));
#47895=CARTESIAN_POINT('Ctrl Pts',(3.33150305271275,-8.59331428149349,108.575088009087));
#47896=CARTESIAN_POINT('Ctrl Pts',(2.90845436138638,-8.61308205548171,108.705187745508));
#47897=CARTESIAN_POINT('Ctrl Pts',(2.56859394875574,-8.63284982946993,108.421654614153));
#47898=CARTESIAN_POINT('Ctrl Pts',(2.62075578170033,-8.65261760345815,107.982137515698));
#47899=CARTESIAN_POINT('Ctrl Pts',(3.0175399713561,-8.67238537744638,107.786029271381));
#47900=CARTESIAN_POINT('Ctrl Pts',(3.39838544402236,-8.6921531514346,108.01153506421));
#47901=CARTESIAN_POINT('Ctrl Pts',(3.41721476990605,-8.71192092542281,108.453735915789));
#47902=CARTESIAN_POINT('Ctrl Pts',(3.05691758489821,-8.73168869941104,108.710800256228));
#47903=CARTESIAN_POINT('Ctrl Pts',(2.64489891990612,-8.75145647339926,108.549131593995));
#47904=CARTESIAN_POINT('Ctrl Pts',(2.55556354232526,-8.77122424738748,108.115639579118));
#47905=CARTESIAN_POINT('Ctrl Pts',(2.87009124837673,-8.7909920213757,107.804241989571));
#47906=CARTESIAN_POINT('Ctrl Pts',(3.30266811109706,-8.81075979536392,107.89790838957));
#47907=CARTESIAN_POINT('Ctrl Pts',(3.4602079588426,-8.83052756935214,108.311523347015));
#47908=CARTESIAN_POINT('Ctrl Pts',(3.19955302944784,-8.85029534334036,108.66923153036));
#47909=CARTESIAN_POINT('Ctrl Pts',(2.75756261231512,-8.87006311732858,108.645980555915));
#47910=CARTESIAN_POINT('Ctrl Pts',(2.5358770538127,-8.8898308913168,108.262898776393));
#47911=CARTESIAN_POINT('Ctrl Pts',(2.73594385381932,-8.90959866530503,107.868095772118));
#47912=CARTESIAN_POINT('Ctrl Pts',(3.17596065704247,-8.92936643929324,107.820332297254));
#47913=CARTESIAN_POINT('Ctrl Pts',(3.45608055639113,-8.94913421328146,108.163011416312));
#47914=CARTESIAN_POINT('Ctrl Pts',(3.32175628333195,-8.96890198726969,108.584737780578));
#47915=CARTESIAN_POINT('Ctrl Pts',(2.89504941536962,-8.9886697612579,108.702285156064));
#47916=CARTESIAN_POINT('Ctrl Pts',(2.56371201137874,-9.00843753524613,108.408837270799));
#47917=CARTESIAN_POINT('Ctrl Pts',(2.62883310982096,-9.02820530923435,107.971052644313));
#47918=CARTESIAN_POINT('Ctrl Pts',(3.0312366301285,-9.04797308322257,107.786749786241));
#47919=CARTESIAN_POINT('Ctrl Pts',(3.40525516637858,-9.06774085721079,108.023406227504));
#47920=CARTESIAN_POINT('Ctrl Pts',(3.41101498234141,-9.08750863119901,108.465970303283));
#47921=CARTESIAN_POINT('Ctrl Pts',(3.04328208563524,-9.10727640518723,108.712280378853));
#47922=CARTESIAN_POINT('Ctrl Pts',(2.63621839985404,-9.12704417917545,108.538512452087));
#47923=CARTESIAN_POINT('Ctrl Pts',(2.55972606184133,-9.14681195316367,108.10257087472));
#47924=CARTESIAN_POINT('Ctrl Pts',(2.88331429152557,-9.16657972715189,107.800599362433));
#47925=CARTESIAN_POINT('Ctrl Pts',(3.31293578932116,-9.18634750114011,107.907001925059));
#47926=CARTESIAN_POINT('Ctrl Pts',(3.45818994787757,-9.20611527512833,108.325089674315));
#47927=CARTESIAN_POINT('Ctrl Pts',(3.18708311291289,-9.22588304911656,108.674942815543));
#47928=CARTESIAN_POINT('Ctrl Pts',(2.7459723056586,-9.24565082310477,108.638646907232));
#47929=CARTESIAN_POINT('Ctrl Pts',(2.53569856627601,-9.265418597093,108.249184340345));
#47930=CARTESIAN_POINT('Ctrl Pts',(2.74733937468242,-9.28518637108122,107.860462971636));
#47931=CARTESIAN_POINT('Ctrl Pts',(3.1885749905948,-9.30495414506944,107.825717117965));
#47932=CARTESIAN_POINT('Ctrl Pts',(3.45845093534624,-9.32472191905766,108.176520634247));
#47933=CARTESIAN_POINT('Ctrl Pts',(3.31172876411578,-9.34448969304588,108.59409544218));
#47934=CARTESIAN_POINT('Ctrl Pts',(2.88173600190796,-9.3642574670341,108.698987910636));
#47935=CARTESIAN_POINT('Ctrl Pts',(2.55921089908849,-9.38402524102233,108.395881278955));
#47936=CARTESIAN_POINT('Ctrl Pts',(2.63723409084994,-9.40379301501054,107.960211282797));
#47937=CARTESIAN_POINT('Ctrl Pts',(3.04490654720541,-9.42356078899876,107.787874341084));
#47938=CARTESIAN_POINT('Ctrl Pts',(3.41177013152627,-9.44332856298698,108.035475562137));
#47939=CARTESIAN_POINT('Ctrl Pts',(3.40445898046695,-9.46309633697521,108.478015256788));
#47940=CARTESIAN_POINT('Ctrl Pts',(3.02960351867329,-9.48286411096342,108.713359165034));
#47941=CARTESIAN_POINT('Ctrl Pts',(2.62786695879146,-9.50263188495165,108.5276368633));
#47942=CARTESIAN_POINT('Ctrl Pts',(2.564247820732,-9.52239965893987,108.089640312703));
#47943=CARTESIAN_POINT('Ctrl Pts',(2.89669475751776,-9.54216743292808,107.797325749426));
#47944=CARTESIAN_POINT('Ctrl Pts',(3.32281396453211,-9.56193520691631,107.916436313859));
#47945=CARTESIAN_POINT('Ctrl Pts',(3.45604186940558,-9.58170298090453,108.33846864974));
#47946=CARTESIAN_POINT('Ctrl Pts',(3.17391765693164,-9.60147075489275,108.680439006897));
#47947=CARTESIAN_POINT('Ctrl Pts',(2.80901503514533,-9.61794389988293,108.638571606125));
#47948=CARTESIAN_POINT('Ctrl Pts',(2.63400072406848,-9.63112241587508,108.433469413069));
#47949=CARTESIAN_POINT('Ctrl Pts',(2.60485441639831,-9.63771167387116,108.302793470514));
#47950=CARTESIAN_POINT('Ctrl Pts',(2.60689261640396,-9.64100630286919,108.237692483505));
#47951=CARTESIAN_POINT('',(3.1742900872407,-9.6,108.602573191677));
#47952=CARTESIAN_POINT('Ctrl Pts',(3.17429377121672,-9.6,108.603153754506));
#47953=CARTESIAN_POINT('Ctrl Pts',(3.16531402749991,-9.6,108.606703341212));
#47954=CARTESIAN_POINT('Ctrl Pts',(3.15621182021442,-9.6,108.609893144108));
#47955=CARTESIAN_POINT('Ctrl Pts',(3.14699950494929,-9.6,108.612705889));
#47956=CARTESIAN_POINT('Ctrl Pts',(3.13221297128382,-9.6,108.617220578938));
#47957=CARTESIAN_POINT('Ctrl Pts',(3.11714267480703,-9.6,108.620764531874));
#47958=CARTESIAN_POINT('Ctrl Pts',(3.10187550064643,-9.6,108.623357279418));
#47959=CARTESIAN_POINT('Ctrl Pts',(3.09495631027381,-9.6,108.624532330784));
#47960=CARTESIAN_POINT('Ctrl Pts',(3.08799668415841,-9.6,108.625511820671));
#47961=CARTESIAN_POINT('Ctrl Pts',(3.08100483727106,-9.6,108.626296670564));
#47962=CARTESIAN_POINT('Ctrl Pts',(3.07531757538958,-9.6,108.626935077976));
#47963=CARTESIAN_POINT('Ctrl Pts',(3.06961045465332,-9.6,108.627444386443));
#47964=CARTESIAN_POINT('Ctrl Pts',(3.06389748778519,-9.6,108.627824830137));
#47965=CARTESIAN_POINT('Ctrl Pts',(3.04242911949262,-9.6,108.629254473532));
#47966=CARTESIAN_POINT('Ctrl Pts',(3.02083984010078,-9.6,108.628872863495));
#47967=CARTESIAN_POINT('Ctrl Pts',(2.9993685461102,-9.6,108.626720448274));
#47968=CARTESIAN_POINT('Ctrl Pts',(2.99279738093697,-9.6,108.626061714061));
#47969=CARTESIAN_POINT('Ctrl Pts',(2.98623737278602,-9.6,108.625236767709));
#47970=CARTESIAN_POINT('Ctrl Pts',(2.97969575955364,-9.6,108.624245868345));
#47971=CARTESIAN_POINT('Ctrl Pts',(2.9737973953897,-9.6,108.62335240597));
#47972=CARTESIAN_POINT('Ctrl Pts',(2.96792150025955,-9.6,108.62232506083));
#47973=CARTESIAN_POINT('Ctrl Pts',(2.96207934152988,-9.6,108.621166234703));
#47974=CARTESIAN_POINT('Ctrl Pts',(2.94154727022957,-9.6,108.61709357907));
#47975=CARTESIAN_POINT('Ctrl Pts',(2.9214053619483,-9.6,108.611396770555));
#47976=CARTESIAN_POINT('Ctrl Pts',(2.90187585569679,-9.6,108.604107979702));
#47977=CARTESIAN_POINT('Ctrl Pts',(2.88931665049007,-9.6,108.599420640511));
#47978=CARTESIAN_POINT('Ctrl Pts',(2.87701101845743,-9.6,108.594073939369));
#47979=CARTESIAN_POINT('Ctrl Pts',(2.86502492333012,-9.6,108.588067088395));
#47980=CARTESIAN_POINT('Ctrl Pts',(2.85938306415935,-9.6,108.58523966154));
#47981=CARTESIAN_POINT('Ctrl Pts',(2.85381209862818,-9.6,108.582265874473));
#47982=CARTESIAN_POINT('Ctrl Pts',(2.84831949871591,-9.6,108.579145145521));
#47983=CARTESIAN_POINT('Ctrl Pts',(2.84383384959628,-9.6,108.576596535518));
#47984=CARTESIAN_POINT('Ctrl Pts',(2.83940054726157,-9.6,108.573949716596));
#47985=CARTESIAN_POINT('Ctrl Pts',(2.83503573984888,-9.6,108.571212399444));
#47986=CARTESIAN_POINT('Ctrl Pts',(2.82136363059275,-9.6,108.562638161079));
#47987=CARTESIAN_POINT('Ctrl Pts',(2.80833101955341,-9.6,108.553159962205));
#47988=CARTESIAN_POINT('Ctrl Pts',(2.79604816320949,-9.6,108.542784903682));
#47989=CARTESIAN_POINT('Ctrl Pts',(2.78292483917589,-9.6,108.531699920591));
#47990=CARTESIAN_POINT('Ctrl Pts',(2.77065685708771,-9.6,108.519590661791));
#47991=CARTESIAN_POINT('Ctrl Pts',(2.75932851942847,-9.6,108.506587814261));
#47992=CARTESIAN_POINT('Ctrl Pts',(2.75483050724524,-9.6,108.501424923786));
#47993=CARTESIAN_POINT('Ctrl Pts',(2.75048091227549,-9.6,108.496121027901));
#47994=CARTESIAN_POINT('Ctrl Pts',(2.7462861731423,-9.6,108.490683960116));
#47995=CARTESIAN_POINT('Ctrl Pts',(2.74283580266206,-9.6,108.486211715815));
#47996=CARTESIAN_POINT('Ctrl Pts',(2.73948942853888,-9.6,108.481647829372));
#47997=CARTESIAN_POINT('Ctrl Pts',(2.73626148259601,-9.6,108.477012896759));
#47998=CARTESIAN_POINT('Ctrl Pts',(2.72501814129942,-9.6,108.460868844106));
#47999=CARTESIAN_POINT('Ctrl Pts',(2.715174764228,-9.6,108.443823493711));
#48000=CARTESIAN_POINT('Ctrl Pts',(2.70685061558342,-9.6,108.426080197397));
#48001=CARTESIAN_POINT('Ctrl Pts',(2.70318585754897,-9.6,108.41826860122));
#48002=CARTESIAN_POINT('Ctrl Pts',(2.69981619459356,-9.6,108.4103214895));
#48003=CARTESIAN_POINT('Ctrl Pts',(2.69675497973943,-9.6,108.40225562313));
#48004=CARTESIAN_POINT('Ctrl Pts',(2.69257854818296,-9.6,108.391251319139));
#48005=CARTESIAN_POINT('Ctrl Pts',(2.68897600041125,-9.6,108.380025872053));
#48006=CARTESIAN_POINT('Ctrl Pts',(2.68596529828858,-9.6,108.368622420101));
#48007=CARTESIAN_POINT('Ctrl Pts',(2.6847911110125,-9.6,108.364175022902));
#48008=CARTESIAN_POINT('Ctrl Pts',(2.68370798559853,-9.6,108.359703786269));
#48009=CARTESIAN_POINT('Ctrl Pts',(2.68271831874412,-9.6,108.355219601019));
#48010=CARTESIAN_POINT('Ctrl Pts',(2.67853974726888,-9.6,108.336286473683));
#48011=CARTESIAN_POINT('Ctrl Pts',(2.67601119798638,-9.6,108.317078942186));
#48012=CARTESIAN_POINT('Ctrl Pts',(2.6751801965963,-9.6,108.297794014685));
#48013=CARTESIAN_POINT('Ctrl Pts',(2.67434919520622,-9.6,108.278509087184));
#48014=CARTESIAN_POINT('Ctrl Pts',(2.67521572840128,-9.6,108.259145218824));
#48015=CARTESIAN_POINT('Ctrl Pts',(2.67788283232033,-9.6,108.239915065145));
#48016=CARTESIAN_POINT('Ctrl Pts',(2.60706672186757,-9.51538364779651,108.249732606859));
#48017=CARTESIAN_POINT('Ctrl Pts',(2.60676993033995,-9.51772231817763,108.203380299727));
#48018=CARTESIAN_POINT('Ctrl Pts',(2.61435669847727,-9.52006098855875,108.157121182639));
#48019=CARTESIAN_POINT('Ctrl Pts',(2.6302588332062,-9.52239965893987,108.113920643923));
#48020=CARTESIAN_POINT('Ctrl Pts',(2.67506346632725,-9.52898891693594,107.992202124944));
#48021=CARTESIAN_POINT('Ctrl Pts',(2.7858791119225,-9.53557817493201,107.894763937185));
#48022=CARTESIAN_POINT('Ctrl Pts',(2.91230680255585,-9.54216743292809,107.865896604045));
#48023=CARTESIAN_POINT('Ctrl Pts',(3.03873449318921,-9.54875669092416,107.837029270904));
#48024=CARTESIAN_POINT('Ctrl Pts',(3.18077422886066,-9.55534594892024,107.876732792381));
#48025=CARTESIAN_POINT('Ctrl Pts',(3.27399874750863,-9.56193520691631,107.966923275767));
#48026=CARTESIAN_POINT('Ctrl Pts',(3.3672232661566,-9.56852446491238,108.057113759153));
#48027=CARTESIAN_POINT('Ctrl Pts',(3.41163256778109,-9.57511372290845,108.197791204446));
#48028=CARTESIAN_POINT('Ctrl Pts',(3.38681651651434,-9.58170298090453,108.325124986619));
#48029=CARTESIAN_POINT('Ctrl Pts',(3.36384682027175,-9.58780198726969,108.442984925999));
#48030=CARTESIAN_POINT('Ctrl Pts',(3.2815695271407,-9.59390099363484,108.549412917973));
#48031=CARTESIAN_POINT('Ctrl Pts',(3.17429377121673,-9.6,108.603153754506));
#48032=CARTESIAN_POINT('',(2.81284134682606,-7.7433,107.987639915065));
#48033=CARTESIAN_POINT('Ctrl Pts',(2.81242348876314,-7.7433,107.987412508431));
#48034=CARTESIAN_POINT('Ctrl Pts',(2.80543771171585,-7.7433,107.991294650159));
#48035=CARTESIAN_POINT('Ctrl Pts',(2.79862088669944,-7.7433,107.995444194259));
#48036=CARTESIAN_POINT('Ctrl Pts',(2.79199078672996,-7.7433,107.999857486819));
#48037=CARTESIAN_POINT('Ctrl Pts',(2.77908729716369,-7.7433,108.008446629481));
#48038=CARTESIAN_POINT('Ctrl Pts',(2.76689025213856,-7.7433,108.018033178706));
#48039=CARTESIAN_POINT('Ctrl Pts',(2.75543032796706,-7.7433,108.028491416979));
#48040=CARTESIAN_POINT('Ctrl Pts',(2.74885145575796,-7.7433,108.034495244937));
#48041=CARTESIAN_POINT('Ctrl Pts',(2.74251154039275,-7.7433,108.040791956438));
#48042=CARTESIAN_POINT('Ctrl Pts',(2.73644185997739,-7.7433,108.047333637481));
#48043=CARTESIAN_POINT('Ctrl Pts',(2.72536667462749,-7.7433,108.059270069895));
#48044=CARTESIAN_POINT('Ctrl Pts',(2.71517634671577,-7.7433,108.072031116775));
#48045=CARTESIAN_POINT('Ctrl Pts',(2.70590800409384,-7.7433,108.085481282292));
#48046=CARTESIAN_POINT('Ctrl Pts',(2.70149813712292,-7.7433,108.091880855883));
#48047=CARTESIAN_POINT('Ctrl Pts',(2.69729719824473,-7.7433,108.098436790851));
#48048=CARTESIAN_POINT('Ctrl Pts',(2.69331048318176,-7.7433,108.105136166992));
#48049=CARTESIAN_POINT('Ctrl Pts',(2.69029373455844,-7.7433,108.110205587161));
#48050=CARTESIAN_POINT('Ctrl Pts',(2.68740348024832,-7.7433,108.115350995326));
#48051=CARTESIAN_POINT('Ctrl Pts',(2.68464466603131,-7.7433,108.120559727848));
#48052=CARTESIAN_POINT('Ctrl Pts',(2.67526428768186,-7.7433,108.138270192538));
#48053=CARTESIAN_POINT('Ctrl Pts',(2.66738748661794,-7.7433,108.156731872377));
#48054=CARTESIAN_POINT('Ctrl Pts',(2.66108511861829,-7.7433,108.175717308618));
#48055=CARTESIAN_POINT('Ctrl Pts',(2.65701462694751,-7.7433,108.187979375843));
#48056=CARTESIAN_POINT('Ctrl Pts',(2.65360153253527,-7.7433,108.200460875424));
#48057=CARTESIAN_POINT('Ctrl Pts',(2.65087412228317,-7.7433,108.213107378602));
#48058=CARTESIAN_POINT('Ctrl Pts',(2.64967297503825,-7.7433,108.218676878987));
#48059=CARTESIAN_POINT('Ctrl Pts',(2.64860492320512,-7.7433,108.224278432823));
#48060=CARTESIAN_POINT('Ctrl Pts',(2.64767292173802,-7.7433,108.229907575979));
#48061=CARTESIAN_POINT('Ctrl Pts',(2.64685670237713,-7.7433,108.234837413315));
#48062=CARTESIAN_POINT('Ctrl Pts',(2.64614551927426,-7.7433,108.239785185843));
#48063=CARTESIAN_POINT('Ctrl Pts',(2.64554197116888,-7.7433,108.244737602616));
#48064=CARTESIAN_POINT('Ctrl Pts',(2.64363794439926,-7.7433,108.26036110309));
#48065=CARTESIAN_POINT('Ctrl Pts',(2.64279904357055,-7.7433,108.276058873989));
#48066=CARTESIAN_POINT('Ctrl Pts',(2.64306324300403,-7.7433,108.291731172273));
#48067=CARTESIAN_POINT('Ctrl Pts',(2.64332016877862,-7.7433,108.306971997444));
#48068=CARTESIAN_POINT('Ctrl Pts',(2.64462004986702,-7.7433,108.322189111009));
#48069=CARTESIAN_POINT('Ctrl Pts',(2.64690694953374,-7.7433,108.337294815271));
#48070=CARTESIAN_POINT('Ctrl Pts',(2.64820783454331,-7.7433,108.34588757713));
#48071=CARTESIAN_POINT('Ctrl Pts',(2.64982842986809,-7.7433,108.354444353112));
#48072=CARTESIAN_POINT('Ctrl Pts',(2.65176092930574,-7.7433,108.3629490723));
#48073=CARTESIAN_POINT('Ctrl Pts',(2.65319972813317,-7.7433,108.369281068965));
#48074=CARTESIAN_POINT('Ctrl Pts',(2.6548126015421,-7.7433,108.375587189865));
#48075=CARTESIAN_POINT('Ctrl Pts',(2.65658913504752,-7.7433,108.381836343915));
#48076=CARTESIAN_POINT('Ctrl Pts',(2.66230148532117,-7.7433,108.401930170878));
#48077=CARTESIAN_POINT('Ctrl Pts',(2.66971154967432,-7.7433,108.421485690035));
#48078=CARTESIAN_POINT('Ctrl Pts',(2.6786763255829,-7.7433,108.4402892797));
#48079=CARTESIAN_POINT('Ctrl Pts',(2.68292788902861,-7.7433,108.449206920841));
#48080=CARTESIAN_POINT('Ctrl Pts',(2.68752991854632,-7.7433,108.457955507247));
#48081=CARTESIAN_POINT('Ctrl Pts',(2.69247119621592,-7.7433,108.466511877091));
#48082=CARTESIAN_POINT('Ctrl Pts',(2.69850572248428,-7.7433,108.47696132803));
#48083=CARTESIAN_POINT('Ctrl Pts',(2.70504610294034,-7.7433,108.487124226895));
#48084=CARTESIAN_POINT('Ctrl Pts',(2.71206752469552,-7.7433,108.496973445774));
#48085=CARTESIAN_POINT('Ctrl Pts',(2.71519702499412,-7.7433,108.501363316444));
#48086=CARTESIAN_POINT('Ctrl Pts',(2.71842256404046,-7.7433,108.505691035234));
#48087=CARTESIAN_POINT('Ctrl Pts',(2.72173214836912,-7.7433,108.50994201636));
#48088=CARTESIAN_POINT('Ctrl Pts',(2.73493899592972,-7.7433,108.526905493988));
#48089=CARTESIAN_POINT('Ctrl Pts',(2.74951416763527,-7.7433,108.542697494939));
#48090=CARTESIAN_POINT('Ctrl Pts',(2.7652868091383,-7.7433,108.557185273403));
#48091=CARTESIAN_POINT('Ctrl Pts',(2.78107258747146,-7.7433,108.57168511855));
#48092=CARTESIAN_POINT('Ctrl Pts',(2.79805862616208,-7.7433,108.584879730222));
#48093=CARTESIAN_POINT('Ctrl Pts',(2.81611663889779,-7.7433,108.596608595281));
#48094=CARTESIAN_POINT('Ctrl Pts',(2.81909225249591,-7.7433,108.598541286928));
#48095=CARTESIAN_POINT('Ctrl Pts',(2.82209705219277,-7.7433,108.600434096425));
#48096=CARTESIAN_POINT('Ctrl Pts',(2.82513055246694,-7.7433,108.602286199445));
#48097=CARTESIAN_POINT('Ctrl Pts',(2.81242348876314,-7.7433,107.987412508431));
#48098=CARTESIAN_POINT('Ctrl Pts',(2.89276360714258,-7.74939900636515,107.930741660299));
#48099=CARTESIAN_POINT('Ctrl Pts',(3.11892943575575,-7.76208727072639,107.892835510919));
#48100=CARTESIAN_POINT('Ctrl Pts',(3.36586763099966,-7.78136479308369,108.145991153067));
#48101=CARTESIAN_POINT('Ctrl Pts',(3.2869314131236,-7.80113256707191,108.499845495719));
#48102=CARTESIAN_POINT('Ctrl Pts',(2.9471249283031,-7.82090034106013,108.626779562835));
#48103=CARTESIAN_POINT('Ctrl Pts',(2.70982409425543,-7.83698193367859,108.451463078785));
#48104=CARTESIAN_POINT('Ctrl Pts',(2.67804342236209,-7.84647426830099,108.297299382674));
#48105=CARTESIAN_POINT('Ctrl Pts',(2.6781760831613,-7.84937734492731,108.250099030543));
#48106=CARTESIAN_POINT('Origin',(3.,-7.7433,108.25));
#48107=CARTESIAN_POINT('',(2.6067,-7.7433,108.25));
#48108=CARTESIAN_POINT('Origin',(3.,-7.7433,108.25));
#48109=CARTESIAN_POINT('Origin',(3.,-7.7433,108.25));
#48110=CARTESIAN_POINT('',(3.18715865317386,-7.7433,107.987639915065));
#48111=CARTESIAN_POINT('Ctrl Pts',(3.17532910733317,-7.7433,108.602640901019));
#48112=CARTESIAN_POINT('Ctrl Pts',(3.18359398155869,-7.7433,108.597648184601));
#48113=CARTESIAN_POINT('Ctrl Pts',(3.19164684676494,-7.7433,108.592340041651));
#48114=CARTESIAN_POINT('Ctrl Pts',(3.19946647439599,-7.7433,108.586715834233));
#48115=CARTESIAN_POINT('Ctrl Pts',(3.21201762835566,-7.7433,108.57768851266));
#48116=CARTESIAN_POINT('Ctrl Pts',(3.22396848685653,-7.7433,108.56784725185));
#48117=CARTESIAN_POINT('Ctrl Pts',(3.23528194102692,-7.7433,108.557273005132));
#48118=CARTESIAN_POINT('Ctrl Pts',(3.2404092782778,-7.7433,108.552480681914));
#48119=CARTESIAN_POINT('Ctrl Pts',(3.24540554458826,-7.7433,108.54753769427));
#48120=CARTESIAN_POINT('Ctrl Pts',(3.25026649528812,-7.7433,108.542451135696));
#48121=CARTESIAN_POINT('Ctrl Pts',(3.25422045744394,-7.7433,108.538313661086));
#48122=CARTESIAN_POINT('Ctrl Pts',(3.25808375246127,-7.7433,108.534082163145));
#48123=CARTESIAN_POINT('Ctrl Pts',(3.26184807585996,-7.7433,108.529767931107));
#48124=CARTESIAN_POINT('Ctrl Pts',(3.27599376874567,-7.7433,108.513555774238));
#48125=CARTESIAN_POINT('Ctrl Pts',(3.28877184484755,-7.7433,108.496149932804));
#48126=CARTESIAN_POINT('Ctrl Pts',(3.30006972609028,-7.7433,108.477764961624));
#48127=CARTESIAN_POINT('Ctrl Pts',(3.3035273783011,-7.7433,108.4721383459));
#48128=CARTESIAN_POINT('Ctrl Pts',(3.30684604562309,-7.7433,108.466419892314));
#48129=CARTESIAN_POINT('Ctrl Pts',(3.31002154851212,-7.7433,108.460615515744));
#48130=CARTESIAN_POINT('Ctrl Pts',(3.31288479673219,-7.7433,108.455381897177));
#48131=CARTESIAN_POINT('Ctrl Pts',(3.3156279244079,-7.7433,108.450085029156));
#48132=CARTESIAN_POINT('Ctrl Pts',(3.31824601493307,-7.7433,108.444735330345));
#48133=CARTESIAN_POINT('Ctrl Pts',(3.32744720835576,-7.7433,108.425933989045));
#48134=CARTESIAN_POINT('Ctrl Pts',(3.33511994980111,-7.7433,108.406458901024));
#48135=CARTESIAN_POINT('Ctrl Pts',(3.34115516947733,-7.7433,108.386506354067));
#48136=CARTESIAN_POINT('Ctrl Pts',(3.3450363511826,-7.7433,108.373675096155));
#48137=CARTESIAN_POINT('Ctrl Pts',(3.34823935165694,-7.7433,108.360646030631));
#48138=CARTESIAN_POINT('Ctrl Pts',(3.35072357452333,-7.7433,108.347471155269));
#48139=CARTESIAN_POINT('Ctrl Pts',(3.35189289819558,-7.7433,108.3412697416));
#48140=CARTESIAN_POINT('Ctrl Pts',(3.35290283345036,-7.7433,108.335036040526));
#48141=CARTESIAN_POINT('Ctrl Pts',(3.35374839004862,-7.7433,108.328775643654));
#48142=CARTESIAN_POINT('Ctrl Pts',(3.35443893300448,-7.7433,108.323662948691));
#48143=CARTESIAN_POINT('Ctrl Pts',(3.35501963039338,-7.7433,108.318532388353));
#48144=CARTESIAN_POINT('Ctrl Pts',(3.35548683149189,-7.7433,108.31340148095));
#48145=CARTESIAN_POINT('Ctrl Pts',(3.35695026851071,-7.7433,108.2973296869));
#48146=CARTESIAN_POINT('Ctrl Pts',(3.35730709707381,-7.7433,108.281218884331));
#48147=CARTESIAN_POINT('Ctrl Pts',(3.35649615794086,-7.7433,108.265161086695));
#48148=CARTESIAN_POINT('Ctrl Pts',(3.35562972897909,-7.7433,108.248004508144));
#48149=CARTESIAN_POINT('Ctrl Pts',(3.35343019058695,-7.7433,108.230907725327));
#48150=CARTESIAN_POINT('Ctrl Pts',(3.34995042508722,-7.7433,108.214016990077));
#48151=CARTESIAN_POINT('Ctrl Pts',(3.34856875501914,-7.7433,108.207310382024));
#48152=CARTESIAN_POINT('Ctrl Pts',(3.34698498184747,-7.7433,108.200636402444));
#48153=CARTESIAN_POINT('Ctrl Pts',(3.34520143590219,-7.7433,108.194004919961));
#48154=CARTESIAN_POINT('Ctrl Pts',(3.34373439173525,-7.7433,108.188550236991));
#48155=CARTESIAN_POINT('Ctrl Pts',(3.34213143104911,-7.7433,108.183122755611));
#48156=CARTESIAN_POINT('Ctrl Pts',(3.34040019349256,-7.7433,108.177746436119));
#48157=CARTESIAN_POINT('Ctrl Pts',(3.33437005187905,-7.7433,108.159019966273));
#48158=CARTESIAN_POINT('Ctrl Pts',(3.32677462929342,-7.7433,108.140861064214));
#48159=CARTESIAN_POINT('Ctrl Pts',(3.31770342973941,-7.7433,108.123487824168));
#48160=CARTESIAN_POINT('Ctrl Pts',(3.31370977647758,-7.7433,108.11583914481));
#48161=CARTESIAN_POINT('Ctrl Pts',(3.30942951053824,-7.7433,108.10834310507));
#48162=CARTESIAN_POINT('Ctrl Pts',(3.30486787449355,-7.7433,108.101020483498));
#48163=CARTESIAN_POINT('Ctrl Pts',(3.29864441319003,-7.7433,108.091030196779));
#48164=CARTESIAN_POINT('Ctrl Pts',(3.29189729436454,-7.7433,108.081362445845));
#48165=CARTESIAN_POINT('Ctrl Pts',(3.2846499513607,-7.7433,108.072057658498));
#48166=CARTESIAN_POINT('Ctrl Pts',(3.28182345518518,-7.7433,108.068428749829));
#48167=CARTESIAN_POINT('Ctrl Pts',(3.27892281702297,-7.7433,108.064857837219));
#48168=CARTESIAN_POINT('Ctrl Pts',(3.27595524844569,-7.7433,108.06135342638));
#48169=CARTESIAN_POINT('Ctrl Pts',(3.2634255806509,-7.7433,108.046557103233));
#48170=CARTESIAN_POINT('Ctrl Pts',(3.24967781791732,-7.7433,108.032907128281));
#48171=CARTESIAN_POINT('Ctrl Pts',(3.23483988540938,-7.7433,108.02056068259));
#48172=CARTESIAN_POINT('Ctrl Pts',(3.22000195290144,-7.7433,108.008214236899));
#48173=CARTESIAN_POINT('Ctrl Pts',(3.20407262972842,-7.7433,107.997170373806));
#48174=CARTESIAN_POINT('Ctrl Pts',(3.18715865317386,-7.7433,107.987639915065));
#48175=CARTESIAN_POINT('Origin',(3.,-7.7433,108.25));
#48176=CARTESIAN_POINT('Origin',(3.,-7.51222265507269,108.25));
#48177=CARTESIAN_POINT('Ctrl Pts',(3.18715865317386,-7.7433,107.987639915065));
#48178=CARTESIAN_POINT('Ctrl Pts',(3.23060708786083,-7.74659462899803,108.018634532712));
#48179=CARTESIAN_POINT('Ctrl Pts',(3.30131753225317,-7.75318388699411,108.102515506643));
#48180=CARTESIAN_POINT('Ctrl Pts',(3.34811842236999,-7.76636240298626,108.318434681996));
#48181=CARTESIAN_POINT('Ctrl Pts',(3.19423247158511,-7.78283554797644,108.577086075122));
#48182=CARTESIAN_POINT('Ctrl Pts',(2.83123989782698,-7.80260332196466,108.591198967572));
#48183=CARTESIAN_POINT('Ctrl Pts',(2.683650632963,-7.81656569099675,108.381854103748));
#48184=CARTESIAN_POINT('Ctrl Pts',(2.67726567995051,-7.82393880203276,108.262849788895));
#48185=CARTESIAN_POINT('Ctrl Pts',(2.67736158403691,-7.82472265507269,108.25018840343));
#48186=CARTESIAN_POINT('Ctrl Pts',(3.22840585926081,-7.7022936971308,107.929819342472));
#48187=CARTESIAN_POINT('Ctrl Pts',(3.2814297344059,-7.70558832612884,107.967644749719));
#48188=CARTESIAN_POINT('Ctrl Pts',(3.36772379314303,-7.71217758412492,108.07001194248));
#48189=CARTESIAN_POINT('Ctrl Pts',(3.42483895901983,-7.72535610011706,108.33351674945));
#48190=CARTESIAN_POINT('Ctrl Pts',(3.23703865045203,-7.74182924510725,108.649171370244));
#48191=CARTESIAN_POINT('Ctrl Pts',(2.79404748061548,-7.76159701909547,108.666394551069));
#48192=CARTESIAN_POINT('Ctrl Pts',(2.53904127250649,-7.78136479308369,108.304686401361));
#48193=CARTESIAN_POINT('Ctrl Pts',(2.70248654639492,-7.8011325670719,107.893528865296));
#48194=CARTESIAN_POINT('Ctrl Pts',(3.1364678991552,-7.82090034106013,107.806185082179));
#48195=CARTESIAN_POINT('Ctrl Pts',(3.44635212159991,-7.84066811504835,108.122191599049));
#48196=CARTESIAN_POINT('Ctrl Pts',(3.35067176640996,-7.86043588903657,108.554314595457));
#48197=CARTESIAN_POINT('Ctrl Pts',(2.93631475070566,-7.88020366302479,108.709915415827));
#48198=CARTESIAN_POINT('Ctrl Pts',(2.57983739147979,-7.89997143701301,108.447582221347));
#48199=CARTESIAN_POINT('Ctrl Pts',(2.60516141258424,-7.91973921100123,108.005706756459));
#48200=CARTESIAN_POINT('Ctrl Pts',(2.98928028820116,-7.93950698498946,107.785821511096));
#48201=CARTESIAN_POINT('Ctrl Pts',(3.38313944150234,-7.95927475897767,107.987739588043));
#48202=CARTESIAN_POINT('Ctrl Pts',(3.42883698967919,-7.97904253296589,108.427975643658));
#48203=CARTESIAN_POINT('Ctrl Pts',(3.08484664817965,-7.99881030695412,108.706483864232));
#48204=CARTESIAN_POINT('Ctrl Pts',(2.66375553478411,-8.01857808094234,108.570181375511));
#48205=CARTESIAN_POINT('Ctrl Pts',(2.54821251073349,-8.03834585493055,108.142927445569));
#48206=CARTESIAN_POINT('Ctrl Pts',(2.84321253014143,-8.05811362891878,107.812971221026));
#48207=CARTESIAN_POINT('Ctrl Pts',(3.28068661206076,-8.077881402907,107.880146665863));
#48208=CARTESIAN_POINT('Ctrl Pts',(3.46309845243368,-8.09764917689522,108.283410891203));
#48209=CARTESIAN_POINT('Ctrl Pts',(3.22468889862713,-8.11741695088343,108.656314364447));
#48210=CARTESIAN_POINT('Ctrl Pts',(2.78210268568124,-8.13718472487166,108.659996614914));
#48211=CARTESIAN_POINT('Ctrl Pts',(2.53752156346275,-8.15695249885988,108.291111551816));
#48212=CARTESIAN_POINT('Ctrl Pts',(2.71319842039437,-8.1767202728481,107.884868081583));
#48213=CARTESIAN_POINT('Ctrl Pts',(3.1494942438801,-8.19648804683632,107.810423004522));
#48214=CARTESIAN_POINT('Ctrl Pts',(3.44994341198594,-8.21625582082455,108.135425177598));
#48215=CARTESIAN_POINT('Ctrl Pts',(3.34152528153087,-8.23602359481276,108.56454243909));
#48216=CARTESIAN_POINT('Ctrl Pts',(2.92276030406872,-8.25579136880098,108.70783238558));
#48217=CARTESIAN_POINT('Ctrl Pts',(2.57418367690396,-8.27555914278921,108.435086257996));
#48218=CARTESIAN_POINT('Ctrl Pts',(2.61254986313247,-8.29532691677743,107.994150717502));
#48219=CARTESIAN_POINT('Ctrl Pts',(3.00299519211957,-8.31509469076565,107.785707535342));
#48220=CARTESIAN_POINT('Ctrl Pts',(3.39071876526407,-8.33486246475387,107.999170754528));
#48221=CARTESIAN_POINT('Ctrl Pts',(3.42339296600063,-8.35463023874209,108.440564582897));
#48222=CARTESIAN_POINT('Ctrl Pts',(3.07132647797405,-8.37439801273031,108.708790799225));
#48223=CARTESIAN_POINT('Ctrl Pts',(2.65444502969431,-8.39416578671854,108.560110023074));
#48224=CARTESIAN_POINT('Ctrl Pts',(2.55157223993528,-8.41393356070675,108.129629705006));
#48225=CARTESIAN_POINT('Ctrl Pts',(2.85618946328992,-8.43370133469498,107.808530869205));
#48226=CARTESIAN_POINT('Ctrl Pts',(3.29148851035998,-8.45346910868319,107.888598682568));
#48227=CARTESIAN_POINT('Ctrl Pts',(3.46190953807653,-8.47323688267141,108.2970748611));
#48228=CARTESIAN_POINT('Ctrl Pts',(3.21258954953447,-8.49300465665963,108.662773724142));
#48229=CARTESIAN_POINT('Ctrl Pts',(2.77008767966747,-8.51277243064786,108.653381691296));
#48230=CARTESIAN_POINT('Ctrl Pts',(2.53650903617205,-8.53254020463608,108.277433380461));
#48231=CARTESIAN_POINT('Ctrl Pts',(2.72410846359058,-8.5523079786243,107.876556129986));
#48232=CARTESIAN_POINT('Ctrl Pts',(3.16241281117998,-8.57207575261252,107.815030411778));
#48233=CARTESIAN_POINT('Ctrl Pts',(3.45313129444197,-8.59184352660074,108.14876515466));
#48234=CARTESIAN_POINT('Ctrl Pts',(3.33208562401345,-8.61161130058896,108.574492838499));
#48235=CARTESIAN_POINT('Ctrl Pts',(2.90927100140282,-8.63137907457718,108.705351197129));
#48236=CARTESIAN_POINT('Ctrl Pts',(2.5689025699531,-8.6511468485654,108.422428158143));
#48237=CARTESIAN_POINT('Ctrl Pts',(2.62027593744494,-8.67091462255362,107.982818226238));
#48238=CARTESIAN_POINT('Ctrl Pts',(3.01670770009012,-8.69068239654185,107.785998581175));
#48239=CARTESIAN_POINT('Ctrl Pts',(3.39795703752631,-8.71045017053006,108.010820861702));
#48240=CARTESIAN_POINT('Ctrl Pts',(3.41757952470489,-8.73021794451828,108.452987202702));
#48241=CARTESIAN_POINT('Ctrl Pts',(3.0577440452905,-8.74998571850651,108.710697394335));
#48242=CARTESIAN_POINT('Ctrl Pts',(2.64543607450032,-8.76975349249472,108.549768054749));
#48243=CARTESIAN_POINT('Ctrl Pts',(2.55532327430049,-8.78952126648295,108.116437005369));
#48244=CARTESIAN_POINT('Ctrl Pts',(2.86929189127361,-8.80928904047117,107.804475753492));
#48245=CARTESIAN_POINT('Ctrl Pts',(3.30203604732418,-8.82905681445939,107.897366067954));
#48246=CARTESIAN_POINT('Ctrl Pts',(3.4603175499762,-8.84882458844761,108.310697751998));
#48247=CARTESIAN_POINT('Ctrl Pts',(3.20030468911872,-8.86859236243583,108.668872886961));
#48248=CARTESIAN_POINT('Ctrl Pts',(2.75827330116574,-8.88836013642405,108.646414766355));
#48249=CARTESIAN_POINT('Ctrl Pts',(2.5359009630086,-8.90812791041227,108.263731270057));
#48250=CARTESIAN_POINT('Ctrl Pts',(2.73525925687653,-8.92789568440049,107.868570055129));
#48251=CARTESIAN_POINT('Ctrl Pts',(3.17518965286302,-8.94766345838871,107.82001738472));
#48252=CARTESIAN_POINT('Ctrl Pts',(3.45592376284752,-8.96743123237694,108.162193471856));
#48253=CARTESIAN_POINT('Ctrl Pts',(3.32235618001346,-8.98719900636516,108.58416007709));
#48254=CARTESIAN_POINT('Ctrl Pts',(2.89586087120222,-9.00696678035337,108.70247265748));
#48255=CARTESIAN_POINT('Ctrl Pts',(2.56399764973763,-9.0267345543416,108.409619593032));
#48256=CARTESIAN_POINT('Ctrl Pts',(2.62833336876932,-9.04650232832981,107.971718884682));
#48257=CARTESIAN_POINT('Ctrl Pts',(3.03040562848843,-9.06627010231804,107.786694526614));
#48258=CARTESIAN_POINT('Ctrl Pts',(3.40484804221826,-9.08603787630626,108.02267968276));
#48259=CARTESIAN_POINT('Ctrl Pts',(3.41140169273562,-9.10580565029448,108.465232690641));
#48260=CARTESIAN_POINT('Ctrl Pts',(3.04411122368577,-9.1255734242827,108.712201973012));
#48261=CARTESIAN_POINT('Ctrl Pts',(2.63673652088457,-9.14534119827093,108.539164501099));
#48262=CARTESIAN_POINT('Ctrl Pts',(2.55946234514999,-9.16510897225914,108.103360856223));
#48263=CARTESIAN_POINT('Ctrl Pts',(2.88250837829689,-9.18487674624736,107.800809413777));
#48264=CARTESIAN_POINT('Ctrl Pts',(3.31232002033802,-9.20464452023558,107.906441170695));
#48265=CARTESIAN_POINT('Ctrl Pts',(3.45832387583295,-9.22441229422381,108.324267676709));
#48266=CARTESIAN_POINT('Ctrl Pts',(3.18784504000744,-9.24418006821202,108.674606529979));
#48267=CARTESIAN_POINT('Ctrl Pts',(2.74666985451794,-9.26394784220025,108.639101920787));
#48268=CARTESIAN_POINT('Ctrl Pts',(2.53569788572799,-9.28371561618846,108.250017174951));
#48269=CARTESIAN_POINT('Ctrl Pts',(2.74664104561622,-9.30348339017669,107.860916831198));
#48270=CARTESIAN_POINT('Ctrl Pts',(3.18781367206768,-9.32325116416491,107.825379560034));
#48271=CARTESIAN_POINT('Ctrl Pts',(3.45831826603152,-9.34301893815313,108.175698436513));
#48272=CARTESIAN_POINT('Ctrl Pts',(3.31234568839827,-9.36278671214135,108.593535664409));
#48273=CARTESIAN_POINT('Ctrl Pts',(2.88254107342349,-9.38255448612957,108.699199398396));
#48274=CARTESIAN_POINT('Ctrl Pts',(2.55947437314993,-9.40232226011779,108.396671482843));
#48275=CARTESIAN_POINT('Ctrl Pts',(2.63671255465142,-9.42209003410602,107.960862951622));
#48276=CARTESIAN_POINT('Ctrl Pts',(3.04408258286891,-9.44185780809423,107.787793567058));
#48277=CARTESIAN_POINT('Ctrl Pts',(3.41137353694225,-9.46162558208245,108.034739653178));
#48278=CARTESIAN_POINT('Ctrl Pts',(3.40489100622148,-9.48139335607067,108.477284935403));
#48279=CARTESIAN_POINT('Ctrl Pts',(3.03038134687606,-9.50116113005889,108.713317276513));
#48280=CARTESIAN_POINT('Ctrl Pts',(2.62847550512648,-9.52092890404712,108.528286005137));
#48281=CARTESIAN_POINT('Ctrl Pts',(2.56370021112967,-9.54069667803534,108.090490261637));
#48282=CARTESIAN_POINT('Ctrl Pts',(2.8963776495683,-9.56046445202356,107.797465456433));
#48283=CARTESIAN_POINT('Ctrl Pts',(3.2500595337559,-9.57693759701374,107.89654078295));
#48284=CARTESIAN_POINT('Ctrl Pts',(3.3904177724541,-9.59011611300589,108.126750448904));
#48285=CARTESIAN_POINT('Ctrl Pts',(3.39852125534571,-9.59670537100196,108.26039191063));
#48286=CARTESIAN_POINT('Ctrl Pts',(3.38620837767256,-9.6,108.324350380063));
#48287=CARTESIAN_POINT('Ctrl Pts',(3.21465679056516,-7.71596246475387,107.949092866669));
#48288=CARTESIAN_POINT('Ctrl Pts',(3.26448885222421,-7.71925709375191,107.98464134405));
#48289=CARTESIAN_POINT('Ctrl Pts',(3.34558837284641,-7.72584635174798,108.080846463868));
#48290=CARTESIAN_POINT('Ctrl Pts',(3.39926544680322,-7.73902486774013,108.328489393632));
#48291=CARTESIAN_POINT('Ctrl Pts',(3.22276992416306,-7.75549801273031,108.625142938537));
#48292=CARTESIAN_POINT('Ctrl Pts',(2.80644495301932,-7.77526578671853,108.64132935657));
#48293=CARTESIAN_POINT('Ctrl Pts',(2.56678904233463,-7.79503356070675,108.301394510814));
#48294=CARTESIAN_POINT('Ctrl Pts',(2.72039560058791,-7.81480133469497,107.914986923049));
#48295=CARTESIAN_POINT('Ctrl Pts',(3.12825310761566,-7.83456910868319,107.832900867024));
#48296=CARTESIAN_POINT('Ctrl Pts',(3.41948360779651,-7.85433688267141,108.129885125346));
#48297=CARTESIAN_POINT('Ctrl Pts',(3.32956280615123,-7.87410465665963,108.53599614123));
#48298=CARTESIAN_POINT('Ctrl Pts',(2.94014833391706,-7.89387243064786,108.682230448957));
#48299=CARTESIAN_POINT('Ctrl Pts',(2.60512940713378,-7.91364020463607,108.435688605557));
#48300=CARTESIAN_POINT('Ctrl Pts',(2.62892902905276,-7.9334079786243,108.020412178633));
#48301=CARTESIAN_POINT('Ctrl Pts',(2.9899255696068,-7.95317575261252,107.813763096971));
#48302=CARTESIAN_POINT('Ctrl Pts',(3.36007606423926,-7.97294352660074,108.003526557921));
#48303=CARTESIAN_POINT('Ctrl Pts',(3.40302281289135,-7.99271130058896,108.417262261091));
#48304=CARTESIAN_POINT('Ctrl Pts',(3.0797392380712,-8.01247907457718,108.679005462285));
#48305=CARTESIAN_POINT('Ctrl Pts',(2.68399603240422,-8.0322468485654,108.550907808094));
#48306=CARTESIAN_POINT('Ctrl Pts',(2.57540821072938,-8.05201462255362,108.149372761425));
#48307=CARTESIAN_POINT('Ctrl Pts',(2.85265047407456,-8.07178239654184,107.839278508954));
#48308=CARTESIAN_POINT('Ctrl Pts',(3.26379046270775,-8.09155017053007,107.90241027554));
#48309=CARTESIAN_POINT('Ctrl Pts',(3.43522188019526,-8.11131794451828,108.28139969657));
#48310=CARTESIAN_POINT('Ctrl Pts',(3.21116357527346,-8.13108571850651,108.631855954637));
#48311=CARTESIAN_POINT('Ctrl Pts',(2.79521918432476,-8.15085349249472,108.635316549168));
#48312=CARTESIAN_POINT('Ctrl Pts',(2.5653608133611,-8.17062126648295,108.288636809916));
#48313=CARTESIAN_POINT('Ctrl Pts',(2.73046266498416,-8.19038904047117,107.906847481961));
#48314=CARTESIAN_POINT('Ctrl Pts',(3.14049532136837,-8.21015681445939,107.836883684329));
#48315=CARTESIAN_POINT('Ctrl Pts',(3.42285871765904,-8.22992458844761,108.142322098321));
#48316=CARTESIAN_POINT('Ctrl Pts',(3.32096690105733,-8.24969236243583,108.545608311845));
#48317=CARTESIAN_POINT('Ctrl Pts',(2.92740980775846,-8.26946013642405,108.680272808339));
#48318=CARTESIAN_POINT('Ctrl Pts',(2.5998160223128,-8.28922791041227,108.423944846458));
#48319=CARTESIAN_POINT('Ctrl Pts',(2.63587272606239,-8.30899568440049,108.009551764446));
#48320=CARTESIAN_POINT('Ctrl Pts',(3.00281489419577,-8.32876345838872,107.813655982077));
#48321=CARTESIAN_POINT('Ctrl Pts',(3.36719914470057,-8.34853123237693,108.014269616431));
#48322=CARTESIAN_POINT('Ctrl Pts',(3.39790649646067,-8.36829900636515,108.429093399322));
#48323=CARTESIAN_POINT('Ctrl Pts',(3.06703292504744,-8.38806678035338,108.681173529528));
#48324=CARTESIAN_POINT('Ctrl Pts',(2.675245980424,-8.40783455434159,108.541442708565));
#48325=CARTESIAN_POINT('Ctrl Pts',(2.57856569841362,-8.42760232832982,108.136875488718));
#48326=CARTESIAN_POINT('Ctrl Pts',(2.86484625061921,-8.44737010231804,107.835105447572));
#48327=CARTESIAN_POINT('Ctrl Pts',(3.27394213232089,-8.46713787630626,107.910353516512));
#48328=CARTESIAN_POINT('Ctrl Pts',(3.43410453346437,-8.48690565029448,108.294241153151));
#48329=CARTESIAN_POINT('Ctrl Pts',(3.19979255592849,-8.5066734242827,108.637926488142));
#48330=CARTESIAN_POINT('Ctrl Pts',(2.78392743096132,-8.52644119827092,108.629099816032));
#48331=CARTESIAN_POINT('Ctrl Pts',(2.56440923593972,-8.54620897225914,108.275782006746));
#48332=CARTESIAN_POINT('Ctrl Pts',(2.74071596962794,-8.56597674624737,107.899035874767));
#48333=CARTESIAN_POINT('Ctrl Pts',(3.15263624544216,-8.58574452023558,107.841213745114));
#48334=CARTESIAN_POINT('Ctrl Pts',(3.42585470304631,-8.60551229422381,108.154859065068));
#48335=CARTESIAN_POINT('Ctrl Pts',(3.31209547108053,-8.62528006821203,108.554959739207));
#48336=CARTESIAN_POINT('Ctrl Pts',(2.91473250417878,-8.64504784220024,108.677940976962));
#48337=CARTESIAN_POINT('Ctrl Pts',(2.59485281571043,-8.66481561618847,108.41204871079));
#48338=CARTESIAN_POINT('Ctrl Pts',(2.64313372331067,-8.68458339017669,107.998901441326));
#48339=CARTESIAN_POINT('Ctrl Pts',(3.01570196706283,-8.7043511641649,107.813929508179));
#48340=CARTESIAN_POINT('Ctrl Pts',(3.37400170352317,-8.72411893815313,108.025218436325));
#48341=CARTESIAN_POINT('Ctrl Pts',(3.39244299979417,-8.74388671214134,108.440768229847));
#48342=CARTESIAN_POINT('Ctrl Pts',(3.05426809748411,-8.76365448612957,108.68296535566));
#48343=CARTESIAN_POINT('Ctrl Pts',(2.66677932630862,-8.78342226011778,108.531723283083));
#48344=CARTESIAN_POINT('Ctrl Pts',(2.58209093634202,-8.80319003410601,108.124476933917));
#48345=CARTESIAN_POINT('Ctrl Pts',(2.87715996773966,-8.82295780809423,107.831294432709));
#48346=CARTESIAN_POINT('Ctrl Pts',(3.2838547520778,-8.84272558208245,107.918593142302));
#48347=CARTESIAN_POINT('Ctrl Pts',(3.43260837632838,-8.86249335607067,108.307044003515));
#48348=CARTESIAN_POINT('Ctrl Pts',(3.18824719225911,-8.8822611300589,108.643658507101));
#48349=CARTESIAN_POINT('Ctrl Pts',(2.77282422818049,-8.90202890404711,108.622552270567));
#48350=CARTESIAN_POINT('Ctrl Pts',(2.56383776621423,-8.92179667803534,108.262904705555));
#48351=CARTESIAN_POINT('Ctrl Pts',(2.75119553222219,-8.94156445202356,107.89153052791));
#48352=CARTESIAN_POINT('Ctrl Pts',(3.16464397518306,-8.96133222601178,107.845900523333));
#48353=CARTESIAN_POINT('Ctrl Pts',(3.42847907664,-8.9811,108.167479054246));
#48354=CARTESIAN_POINT('Ctrl Pts',(3.3029516985443,-9.00086777398822,108.564045050838));
#48355=CARTESIAN_POINT('Ctrl Pts',(2.90212960721617,-9.02063554797644,108.675235713249));
#48356=CARTESIAN_POINT('Ctrl Pts',(2.59024315098975,-9.04040332196466,108.400011167238));
#48357=CARTESIAN_POINT('Ctrl Pts',(2.6507061312773,-9.06017109595288,107.988470233284));
#48358=CARTESIAN_POINT('Ctrl Pts',(3.02857533798636,-9.0799388699411,107.81458356064));
#48359=CARTESIAN_POINT('Ctrl Pts',(3.3804778988175,-9.09970664392933,108.036363406408));
#48360=CARTESIAN_POINT('Ctrl Pts',(3.38663704723469,-9.11947441791755,108.452276591096));
#48361=CARTESIAN_POINT('Ctrl Pts',(3.04145591419998,-9.13924219190576,108.684379365051));
#48362=CARTESIAN_POINT('Ctrl Pts',(2.65860344910236,-9.15900996589399,108.521758018608));
#48363=CARTESIAN_POINT('Ctrl Pts',(2.58598085259615,-9.17877773988221,108.112187913759));
#48364=CARTESIAN_POINT('Ctrl Pts',(2.88958087802693,-9.19854551387043,107.82784879117));
#48365=CARTESIAN_POINT('Ctrl Pts',(3.29351967332174,-9.21831328785865,107.927121962161));
#48366=CARTESIAN_POINT('Ctrl Pts',(3.43073471295386,-9.23808106184687,108.319797076032));
#48367=CARTESIAN_POINT('Ctrl Pts',(3.17653756143592,-9.25784883583509,108.649047009009));
#48368=CARTESIAN_POINT('Ctrl Pts',(2.76191926004626,-9.27761660982331,108.615679627437));
#48369=CARTESIAN_POINT('Ctrl Pts',(2.56364691332878,-9.29738438381153,108.250016141092));
#48370=CARTESIAN_POINT('Ctrl Pts',(2.76189218531883,-9.31715215779975,107.884337995758));
#48371=CARTESIAN_POINT('Ctrl Pts',(3.17650808171374,-9.33691993178797,107.850939918326));
#48372=CARTESIAN_POINT('Ctrl Pts',(3.4307294408388,-9.35668770577619,108.180171077031));
#48373=CARTESIAN_POINT('Ctrl Pts',(3.2935437962731,-9.37645547976441,108.572856267372));
#48374=CARTESIAN_POINT('Ctrl Pts',(2.88961160504489,-9.39622325375264,108.672159490547));
#48375=CARTESIAN_POINT('Ctrl Pts',(2.58599215656126,-9.41599102774085,108.387842478632));
#48376=CARTESIAN_POINT('Ctrl Pts',(2.65858092553529,-9.43575880172908,107.978267781575));
#48377=CARTESIAN_POINT('Ctrl Pts',(3.04142899743941,-9.4555265757173,107.815616443488));
#48378=CARTESIAN_POINT('Ctrl Pts',(3.38661058630124,-9.47529434970552,108.047697417508));
#48379=CARTESIAN_POINT('Ctrl Pts',(3.38051827656907,-9.49506212369374,108.463603341592));
#48380=CARTESIAN_POINT('Ctrl Pts',(3.02855251802456,-9.51482989768196,108.685427531988));
#48381=CARTESIAN_POINT('Ctrl Pts',(2.65083971162567,-9.53459767167018,108.511534362189));
#48382=CARTESIAN_POINT('Ctrl Pts',(2.5899636169306,-9.5543654456584,108.100092074644));
#48383=CARTESIAN_POINT('Ctrl Pts',(2.90261527770578,-9.57413321964662,107.824706125944));
#48384=CARTESIAN_POINT('Ctrl Pts',(3.23500700524924,-9.59060636463681,107.917817535972));
#48385=CARTESIAN_POINT('Ctrl Pts',(3.36691627038736,-9.60378488062896,108.134169551681));
#48386=CARTESIAN_POINT('Ctrl Pts',(3.37453195781123,-9.61037413862503,108.259766361471));
#48387=CARTESIAN_POINT('Ctrl Pts',(3.36296026340509,-9.61366876762306,108.319874800994));
#48388=CARTESIAN_POINT('Ctrl Pts',(3.20090772186951,-7.72963123237693,107.968366390867));
#48389=CARTESIAN_POINT('Ctrl Pts',(3.24754797004252,-7.73292586137497,108.001637938381));
#48390=CARTESIAN_POINT('Ctrl Pts',(3.32345295254979,-7.73951511937104,108.091680985256));
#48391=CARTESIAN_POINT('Ctrl Pts',(3.3736919345866,-7.75269363536319,108.323462037814));
#48392=CARTESIAN_POINT('Ctrl Pts',(3.20850119787409,-7.76916678035338,108.601114506829));
#48393=CARTESIAN_POINT('Ctrl Pts',(2.81884242542315,-7.7889345543416,108.616264162071));
#48394=CARTESIAN_POINT('Ctrl Pts',(2.59453681216278,-7.80870232832982,108.298102620267));
#48395=CARTESIAN_POINT('Ctrl Pts',(2.73830465478089,-7.82847010231804,107.936444980801));
#48396=CARTESIAN_POINT('Ctrl Pts',(3.12003831607613,-7.84823787630626,107.859616651869));
#48397=CARTESIAN_POINT('Ctrl Pts',(3.39261509399311,-7.86800565029448,108.137578651642));
#48398=CARTESIAN_POINT('Ctrl Pts',(3.30845384589251,-7.8877734242827,108.517677687003));
#48399=CARTESIAN_POINT('Ctrl Pts',(2.94398191712845,-7.90754119827092,108.654545482088));
#48400=CARTESIAN_POINT('Ctrl Pts',(2.63042142278778,-7.92730897225914,108.423794989766));
#48401=CARTESIAN_POINT('Ctrl Pts',(2.65269664552128,-7.94707674624736,108.035117600806));
#48402=CARTESIAN_POINT('Ctrl Pts',(2.99057085101244,-7.96684452023558,107.841704682847));
#48403=CARTESIAN_POINT('Ctrl Pts',(3.33701268697619,-7.9866122942238,108.019313527799));
#48404=CARTESIAN_POINT('Ctrl Pts',(3.37720863610352,-8.00638006821202,108.406548878524));
#48405=CARTESIAN_POINT('Ctrl Pts',(3.07463182796275,-8.02614784220024,108.651527060338));
#48406=CARTESIAN_POINT('Ctrl Pts',(2.70423653002431,-8.04591561618847,108.531634240676));
#48407=CARTESIAN_POINT('Ctrl Pts',(2.60260391072527,-8.06568339017669,108.155818077281));
#48408=CARTESIAN_POINT('Ctrl Pts',(2.8620884180077,-8.0854511641649,107.865585796883));
#48409=CARTESIAN_POINT('Ctrl Pts',(3.24689431335474,-8.10521893815313,107.924673885216));
#48410=CARTESIAN_POINT('Ctrl Pts',(3.40734530795685,-8.12498671214135,108.279388501936));
#48411=CARTESIAN_POINT('Ctrl Pts',(3.1976382519198,-8.14475448612957,108.607397544827));
#48412=CARTESIAN_POINT('Ctrl Pts',(2.80833568296828,-8.16452226011779,108.610636483421));
#48413=CARTESIAN_POINT('Ctrl Pts',(2.59320006325944,-8.18429003410601,108.286162068016));
#48414=CARTESIAN_POINT('Ctrl Pts',(2.74772690957395,-8.20405780809423,107.928826882338));
#48415=CARTESIAN_POINT('Ctrl Pts',(3.13149639885665,-8.22382558208245,107.863344364136));
#48416=CARTESIAN_POINT('Ctrl Pts',(3.39577402333215,-8.24359335607067,108.149219019044));
#48417=CARTESIAN_POINT('Ctrl Pts',(3.30040852058379,-8.26336113005889,108.5266741846));
#48418=CARTESIAN_POINT('Ctrl Pts',(2.93205931144819,-8.28312890404711,108.652713231099));
#48419=CARTESIAN_POINT('Ctrl Pts',(2.62544836772165,-8.30289667803533,108.412803434919));
#48420=CARTESIAN_POINT('Ctrl Pts',(2.65919558899231,-8.32266445202356,108.02495281139));
#48421=CARTESIAN_POINT('Ctrl Pts',(3.00263459627197,-8.34243222601178,107.841604428812));
#48422=CARTESIAN_POINT('Ctrl Pts',(3.34367952413706,-8.3622,108.029368478334));
#48423=CARTESIAN_POINT('Ctrl Pts',(3.37242002692071,-8.38196777398822,108.417622215747));
#48424=CARTESIAN_POINT('Ctrl Pts',(3.06273937212083,-8.40173554797644,108.653556259832));
#48425=CARTESIAN_POINT('Ctrl Pts',(2.69604693115369,-8.42150332196466,108.522775394056));
#48426=CARTESIAN_POINT('Ctrl Pts',(2.60555915689196,-8.44127109595288,108.14412127243));
#48427=CARTESIAN_POINT('Ctrl Pts',(2.87350303794851,-8.46103886994111,107.861680025938));
#48428=CARTESIAN_POINT('Ctrl Pts',(3.25639575428181,-8.48080664392932,107.932108350456));
#48429=CARTESIAN_POINT('Ctrl Pts',(3.40629952885221,-8.50057441791754,108.291407445201));
#48430=CARTESIAN_POINT('Ctrl Pts',(3.18699556232252,-8.52034219190576,108.613079252141));
#48431=CARTESIAN_POINT('Ctrl Pts',(2.79776718225517,-8.54010996589398,108.604817940768));
#48432=CARTESIAN_POINT('Ctrl Pts',(2.5923094357074,-8.55987773988221,108.27413063303));
#48433=CARTESIAN_POINT('Ctrl Pts',(2.7573234756653,-8.57964551387043,107.921515619549));
#48434=CARTESIAN_POINT('Ctrl Pts',(3.14285967970434,-8.59941328785865,107.86739707845));
#48435=CARTESIAN_POINT('Ctrl Pts',(3.39857811165065,-8.61918106184687,108.160952975476));
#48436=CARTESIAN_POINT('Ctrl Pts',(3.2921053181476,-8.63894883583509,108.535426639916));
#48437=CARTESIAN_POINT('Ctrl Pts',(2.92019400695475,-8.65871660982331,108.650530756794));
#48438=CARTESIAN_POINT('Ctrl Pts',(2.62080306146777,-8.67848438381153,108.401669263437));
#48439=CARTESIAN_POINT('Ctrl Pts',(2.66599150917639,-8.69825215779975,108.014984656413));
#48440=CARTESIAN_POINT('Ctrl Pts',(3.01469623403554,-8.71801993178797,107.841860435183));
#48441=CARTESIAN_POINT('Ctrl Pts',(3.35004636952003,-8.73778770577619,108.039616010948));
#48442=CARTESIAN_POINT('Ctrl Pts',(3.36730647488344,-8.75755547976441,108.428549256992));
#48443=CARTESIAN_POINT('Ctrl Pts',(3.05079214967772,-8.77732325375264,108.655233316985));
#48444=CARTESIAN_POINT('Ctrl Pts',(2.68812257811692,-8.79709102774085,108.513678511417));
#48445=CARTESIAN_POINT('Ctrl Pts',(2.60885859838356,-8.81685880172908,108.132516862465));
#48446=CARTESIAN_POINT('Ctrl Pts',(2.88502804420571,-8.8366265757173,107.858113111926));
#48447=CARTESIAN_POINT('Ctrl Pts',(3.26567345683143,-8.85639434970552,107.93982021665));
#48448=CARTESIAN_POINT('Ctrl Pts',(3.40489920268056,-8.87616212369374,108.303390255031));
#48449=CARTESIAN_POINT('Ctrl Pts',(3.1761896953995,-8.89592989768196,108.618444127241));
#48450=CARTESIAN_POINT('Ctrl Pts',(2.78737515519524,-8.91569767167018,108.598689774779));
#48451=CARTESIAN_POINT('Ctrl Pts',(2.59177456941985,-8.9354654456584,108.262078141053));
#48452=CARTESIAN_POINT('Ctrl Pts',(2.76713180756785,-8.95523321964662,107.914491000691));
#48453=CARTESIAN_POINT('Ctrl Pts',(3.15409829750309,-8.97500099363484,107.871783661947));
#48454=CARTESIAN_POINT('Ctrl Pts',(3.40103439043249,-8.99476876762306,108.172764636635));
#48455=CARTESIAN_POINT('Ctrl Pts',(3.28354721707514,-9.01453654161128,108.543930024585));
#48456=CARTESIAN_POINT('Ctrl Pts',(2.90839834323012,-9.03430431559951,108.647998769019));
#48457=CARTESIAN_POINT('Ctrl Pts',(2.61648865224188,-9.05407208958772,108.390402741443));
#48458=CARTESIAN_POINT('Ctrl Pts',(2.67307889378527,-9.07383986357594,108.005221581886));
#48459=CARTESIAN_POINT('Ctrl Pts',(3.0267450474843,-9.09360763756417,107.842472594666));
#48460=CARTESIAN_POINT('Ctrl Pts',(3.35610775541675,-9.11337541155239,108.050047130056));
#48461=CARTESIAN_POINT('Ctrl Pts',(3.36187240173376,-9.13314318554061,108.439320491552));
#48462=CARTESIAN_POINT('Ctrl Pts',(3.03880060471419,-9.15291095952883,108.65655675709));
#48463=CARTESIAN_POINT('Ctrl Pts',(2.68047037732015,-9.17267873351705,108.504351536118));
#48464=CARTESIAN_POINT('Ctrl Pts',(2.61249936004231,-9.19244650750527,108.121014971295));
#48465=CARTESIAN_POINT('Ctrl Pts',(2.89665337775696,-9.21221428149349,107.854888168563));
#48466=CARTESIAN_POINT('Ctrl Pts',(3.27471932630547,-9.23198205548171,107.947802753628));
#48467=CARTESIAN_POINT('Ctrl Pts',(3.40314555007477,-9.25174982946993,108.315326475355));
#48468=CARTESIAN_POINT('Ctrl Pts',(3.16523008286441,-9.27151760345816,108.62348748804));
#48469=CARTESIAN_POINT('Ctrl Pts',(2.77716866557457,-9.29128537744637,108.592257334087));
#48470=CARTESIAN_POINT('Ctrl Pts',(2.59159594092957,-9.3110531514346,108.250015107232));
#48471=CARTESIAN_POINT('Ctrl Pts',(2.77714332502144,-9.33082092542281,107.907759160318));
#48472=CARTESIAN_POINT('Ctrl Pts',(3.16520249135981,-9.35058869941103,107.876500276617));
#48473=CARTESIAN_POINT('Ctrl Pts',(3.40314061564608,-9.37035647339926,108.184643717548));
#48474=CARTESIAN_POINT('Ctrl Pts',(3.27474190414793,-9.39012424738748,108.552176870334));
#48475=CARTESIAN_POINT('Ctrl Pts',(2.89668213666629,-9.4098920213757,108.645119582698));
#48476=CARTESIAN_POINT('Ctrl Pts',(2.61250993997259,-9.42965979536392,108.37901347442));
#48477=CARTESIAN_POINT('Ctrl Pts',(2.68044929641917,-9.44942756935214,107.995672611527));
#48478=CARTESIAN_POINT('Ctrl Pts',(3.03877541200992,-9.46919534334036,107.843439319918));
#48479=CARTESIAN_POINT('Ctrl Pts',(3.36184763566024,-9.48896311732858,108.060655181838));
#48480=CARTESIAN_POINT('Ctrl Pts',(3.35614554691665,-9.5087308913168,108.449921747782));
#48481=CARTESIAN_POINT('Ctrl Pts',(3.02672368917307,-9.52849866530503,108.657537787464));
#48482=CARTESIAN_POINT('Ctrl Pts',(2.67320391812486,-9.54826643929324,108.49478271924));
#48483=CARTESIAN_POINT('Ctrl Pts',(2.61622702273152,-9.56803421328147,108.109693887651));
#48484=CARTESIAN_POINT('Ctrl Pts',(2.90885290584327,-9.58780198726969,107.851946795456));
#48485=CARTESIAN_POINT('Ctrl Pts',(3.21995447674257,-9.60427513225987,107.939094288995));
#48486=CARTESIAN_POINT('Ctrl Pts',(3.34341476832062,-9.61745364825202,108.141588654458));
#48487=CARTESIAN_POINT('Ctrl Pts',(3.35054266027676,-9.62404290624809,108.259140812312));
#48488=CARTESIAN_POINT('Ctrl Pts',(3.33971214913761,-9.62733753524613,108.315399221924));
#48489=CARTESIAN_POINT('Ctrl Pts',(3.18715865317386,-7.7433,107.987639915065));
#48490=CARTESIAN_POINT('Ctrl Pts',(3.23060708786083,-7.74659462899803,108.018634532712));
#48491=CARTESIAN_POINT('Ctrl Pts',(3.30131753225317,-7.75318388699411,108.102515506643));
#48492=CARTESIAN_POINT('Ctrl Pts',(3.34811842236999,-7.76636240298626,108.318434681996));
#48493=CARTESIAN_POINT('Ctrl Pts',(3.19423247158511,-7.78283554797644,108.577086075122));
#48494=CARTESIAN_POINT('Ctrl Pts',(2.83123989782698,-7.80260332196466,108.591198967572));
#48495=CARTESIAN_POINT('Ctrl Pts',(2.62228458199092,-7.82237109595288,108.294810729719));
#48496=CARTESIAN_POINT('Ctrl Pts',(2.75621370897387,-7.8421388699411,107.957903038554));
#48497=CARTESIAN_POINT('Ctrl Pts',(3.1118235245366,-7.86190664392932,107.886332436713));
#48498=CARTESIAN_POINT('Ctrl Pts',(3.3657465801897,-7.88167441791754,108.145272177939));
#48499=CARTESIAN_POINT('Ctrl Pts',(3.28734488563378,-7.90144219190576,108.499359232776));
#48500=CARTESIAN_POINT('Ctrl Pts',(2.94781550033985,-7.92120996589399,108.626860515219));
#48501=CARTESIAN_POINT('Ctrl Pts',(2.65571343844177,-7.9409777398822,108.411901373976));
#48502=CARTESIAN_POINT('Ctrl Pts',(2.6764642619898,-7.96074551387043,108.04982302298));
#48503=CARTESIAN_POINT('Ctrl Pts',(2.99121613241808,-7.98051328785865,107.869646268722));
#48504=CARTESIAN_POINT('Ctrl Pts',(3.31394930971311,-8.00028106184687,108.035100497677));
#48505=CARTESIAN_POINT('Ctrl Pts',(3.35139445931568,-8.02004883583509,108.395835495957));
#48506=CARTESIAN_POINT('Ctrl Pts',(3.0695244178543,-8.03981660982331,108.624048658391));
#48507=CARTESIAN_POINT('Ctrl Pts',(2.72447702764442,-8.05958438381153,108.512360673259));
#48508=CARTESIAN_POINT('Ctrl Pts',(2.62979961072117,-8.07935215779975,108.162263393137));
#48509=CARTESIAN_POINT('Ctrl Pts',(2.87152636194084,-8.09911993178797,107.891893084811));
#48510=CARTESIAN_POINT('Ctrl Pts',(3.22999816400173,-8.11888770577619,107.946937494892));
#48511=CARTESIAN_POINT('Ctrl Pts',(3.37946873571844,-8.13865547976441,108.277377307303));
#48512=CARTESIAN_POINT('Ctrl Pts',(3.18411292856613,-8.15842325375263,108.582939135017));
#48513=CARTESIAN_POINT('Ctrl Pts',(2.8214521816118,-8.17819102774085,108.585956417675));
#48514=CARTESIAN_POINT('Ctrl Pts',(2.62103931315779,-8.19795880172907,108.283687326116));
#48515=CARTESIAN_POINT('Ctrl Pts',(2.76499115416374,-8.2177265757173,107.950806282716));
#48516=CARTESIAN_POINT('Ctrl Pts',(3.12249747634493,-8.23749434970551,107.889805043942));
#48517=CARTESIAN_POINT('Ctrl Pts',(3.36868932900526,-8.25726212369374,108.156115939767));
#48518=CARTESIAN_POINT('Ctrl Pts',(3.27985014011025,-8.27702989768196,108.507740057355));
#48519=CARTESIAN_POINT('Ctrl Pts',(2.93670881513792,-8.29679767167018,108.625153653859));
#48520=CARTESIAN_POINT('Ctrl Pts',(2.65108071313049,-8.3165654456584,108.401662023381));
#48521=CARTESIAN_POINT('Ctrl Pts',(2.68251845192224,-8.33633321964662,108.040353858334));
#48522=CARTESIAN_POINT('Ctrl Pts',(3.00245429834817,-8.35610099363484,107.869552875547));
#48523=CARTESIAN_POINT('Ctrl Pts',(3.32015990357356,-8.37586876762306,108.044467340237));
#48524=CARTESIAN_POINT('Ctrl Pts',(3.34693355738075,-8.39563654161128,108.406151032172));
#48525=CARTESIAN_POINT('Ctrl Pts',(3.05844581919422,-8.4154043155995,108.625938990135));
#48526=CARTESIAN_POINT('Ctrl Pts',(2.71684788188338,-8.43517208958773,108.504108079548));
#48527=CARTESIAN_POINT('Ctrl Pts',(2.63255261537031,-8.45493986357594,108.151367056142));
#48528=CARTESIAN_POINT('Ctrl Pts',(2.8821598252778,-8.47470763756417,107.888254604305));
#48529=CARTESIAN_POINT('Ctrl Pts',(3.23884937624272,-8.49447541155238,107.9538631844));
#48530=CARTESIAN_POINT('Ctrl Pts',(3.37849452424005,-8.51424318554061,108.288573737252));
#48531=CARTESIAN_POINT('Ctrl Pts',(3.17419856871655,-8.53401095952883,108.58823201614));
#48532=CARTESIAN_POINT('Ctrl Pts',(2.81160693354902,-8.55377873351705,108.580536065503));
#48533=CARTESIAN_POINT('Ctrl Pts',(2.62020963547507,-8.57354650750527,108.272479259314));
#48534=CARTESIAN_POINT('Ctrl Pts',(2.77393098170266,-8.59331428149349,107.94399536433));
#48535=CARTESIAN_POINT('Ctrl Pts',(3.13308311396652,-8.61308205548171,107.893580411787));
#48536=CARTESIAN_POINT('Ctrl Pts',(3.37130152025498,-8.63284982946993,108.167046885883));
#48537=CARTESIAN_POINT('Ctrl Pts',(3.27211516521468,-8.65261760345815,108.515893540624));
#48538=CARTESIAN_POINT('Ctrl Pts',(2.92565550973071,-8.67238537744637,108.623120536626));
#48539=CARTESIAN_POINT('Ctrl Pts',(2.6467533072251,-8.6921531514346,108.391289816083));
#48540=CARTESIAN_POINT('Ctrl Pts',(2.68884929504212,-8.71192092542282,108.0310678715));
#48541=CARTESIAN_POINT('Ctrl Pts',(3.01369050100825,-8.73168869941104,107.869791362187));
#48542=CARTESIAN_POINT('Ctrl Pts',(3.32609103551689,-8.75145647339926,108.054013585571));
#48543=CARTESIAN_POINT('Ctrl Pts',(3.34216994997271,-8.77122424738748,108.416330284137));
#48544=CARTESIAN_POINT('Ctrl Pts',(3.04731620187133,-8.7909920213757,108.62750127831));
#48545=CARTESIAN_POINT('Ctrl Pts',(2.70946582992522,-8.81075979536392,108.495633739751));
#48546=CARTESIAN_POINT('Ctrl Pts',(2.6356262604251,-8.83052756935215,108.140556791013));
#48547=CARTESIAN_POINT('Ctrl Pts',(2.89289612067176,-8.85029534334036,107.884931791143));
#48548=CARTESIAN_POINT('Ctrl Pts',(3.24749216158505,-8.87006311732858,107.961047290999));
#48549=CARTESIAN_POINT('Ctrl Pts',(3.37719002903275,-8.88983089131681,108.299736506548));
#48550=CARTESIAN_POINT('Ctrl Pts',(3.16413219853988,-8.90959866530502,108.593229747382));
#48551=CARTESIAN_POINT('Ctrl Pts',(2.80192608220999,-8.92936643929325,108.574827278991));
#48552=CARTESIAN_POINT('Ctrl Pts',(2.61971137262547,-8.94913421328146,108.261251576551));
#48553=CARTESIAN_POINT('Ctrl Pts',(2.78306808291351,-8.96890198726969,107.937451473473));
#48554=CARTESIAN_POINT('Ctrl Pts',(3.14355261982312,-8.9886697612579,107.897666800561));
#48555=CARTESIAN_POINT('Ctrl Pts',(3.37358970422498,-9.00843753524613,108.178050219025));
#48556=CARTESIAN_POINT('Ctrl Pts',(3.26414273560599,-9.02820530923435,108.523814998333));
#48557=CARTESIAN_POINT('Ctrl Pts',(2.91466707924407,-9.04797308322257,108.620761824788));
#48558=CARTESIAN_POINT('Ctrl Pts',(2.64273415349401,-9.06774085721079,108.380794315648));
#48559=CARTESIAN_POINT('Ctrl Pts',(2.69545165629325,-9.08750863119901,108.021972930488));
#48560=CARTESIAN_POINT('Ctrl Pts',(3.02491475698223,-9.10727640518723,107.870361628692));
#48561=CARTESIAN_POINT('Ctrl Pts',(3.331737612016,-9.12704417917545,108.063730853703));
#48562=CARTESIAN_POINT('Ctrl Pts',(3.33710775623283,-9.14681195316367,108.426364392007));
#48563=CARTESIAN_POINT('Ctrl Pts',(3.0361452952284,-9.1665797271519,108.628734149129));
#48564=CARTESIAN_POINT('Ctrl Pts',(2.70233730553794,-9.18634750114011,108.486945053627));
#48565=CARTESIAN_POINT('Ctrl Pts',(2.63901786748847,-9.20611527512833,108.129842028831));
#48566=CARTESIAN_POINT('Ctrl Pts',(2.90372587748699,-9.22588304911656,107.881927545957));
#48567=CARTESIAN_POINT('Ctrl Pts',(3.25591897928919,-9.24565082310478,107.968483545095));
#48568=CARTESIAN_POINT('Ctrl Pts',(3.37555638719568,-9.265418597093,108.310855874679));
#48569=CARTESIAN_POINT('Ctrl Pts',(3.15392260429289,-9.28518637108122,108.597927967071));
#48570=CARTESIAN_POINT('Ctrl Pts',(2.79241807110289,-9.30495414506944,108.568835040736));
#48571=CARTESIAN_POINT('Ctrl Pts',(2.61954496853035,-9.32472191905766,108.250014073372));
#48572=CARTESIAN_POINT('Ctrl Pts',(2.79239446472405,-9.34448969304588,107.931180324878));
#48573=CARTESIAN_POINT('Ctrl Pts',(3.15389690100588,-9.3642574670341,107.902060634909));
#48574=CARTESIAN_POINT('Ctrl Pts',(3.37555179045336,-9.38402524102232,108.189116358066));
#48575=CARTESIAN_POINT('Ctrl Pts',(3.25594001202276,-9.40379301501054,108.531497473297));
#48576=CARTESIAN_POINT('Ctrl Pts',(2.9037526682877,-9.42356078899877,108.618079674849));
#48577=CARTESIAN_POINT('Ctrl Pts',(2.63902772338391,-9.44332856298698,108.370184470209));
#48578=CARTESIAN_POINT('Ctrl Pts',(2.70231766730304,-9.46309633697521,108.01307744148));
#48579=CARTESIAN_POINT('Ctrl Pts',(3.03612182658042,-9.48286411096343,107.871262196348));
#48580=CARTESIAN_POINT('Ctrl Pts',(3.33708468501923,-9.50263188495165,108.073612946168));
#48581=CARTESIAN_POINT('Ctrl Pts',(3.33177281726424,-9.52239965893987,108.436240153971));
#48582=CARTESIAN_POINT('Ctrl Pts',(3.02489486032158,-9.54216743292809,108.629648042939));
#48583=CARTESIAN_POINT('Ctrl Pts',(2.69556812462404,-9.56193520691631,108.478031076292));
#48584=CARTESIAN_POINT('Ctrl Pts',(2.64249042853245,-9.58170298090453,108.119295700658));
#48585=CARTESIAN_POINT('Ctrl Pts',(2.91509053398075,-9.60147075489276,107.879187464968));
#48586=CARTESIAN_POINT('Ctrl Pts',(3.20490194823591,-9.61794389988293,107.960371042017));
#48587=CARTESIAN_POINT('Ctrl Pts',(3.31991326625387,-9.63112241587508,108.149007757235));
#48588=CARTESIAN_POINT('Ctrl Pts',(3.32655336274228,-9.63771167387116,108.258515263153));
#48589=CARTESIAN_POINT('Ctrl Pts',(3.31646403487013,-9.64100630286919,108.310923642855));
#48590=CARTESIAN_POINT('',(3.38620837767256,-9.6,108.324350380063));
#48591=CARTESIAN_POINT('Ctrl Pts',(2.9047663113757,-9.6,107.941669514675));
#48592=CARTESIAN_POINT('Ctrl Pts',(2.91208752841734,-9.6,107.938464535723));
#48593=CARTESIAN_POINT('Ctrl Pts',(2.91951909466324,-9.6,107.93555598867));
#48594=CARTESIAN_POINT('Ctrl Pts',(2.9270473341129,-9.6,107.93295579821));
#48595=CARTESIAN_POINT('Ctrl Pts',(2.94169878127661,-9.6,107.927895311836));
#48596=CARTESIAN_POINT('Ctrl Pts',(2.95671562307874,-9.6,107.924001174705));
#48597=CARTESIAN_POINT('Ctrl Pts',(2.97197926144626,-9.6,107.921221613959));
#48598=CARTESIAN_POINT('Ctrl Pts',(2.98074175619374,-9.6,107.9196259337));
#48599=CARTESIAN_POINT('Ctrl Pts',(2.98959245259031,-9.6,107.918397815162));
#48600=CARTESIAN_POINT('Ctrl Pts',(2.998474281856,-9.6,107.917533107911));
#48601=CARTESIAN_POINT('Ctrl Pts',(3.01468072942063,-9.6,107.915955298622));
#48602=CARTESIAN_POINT('Ctrl Pts',(3.03100700663023,-9.6,107.915581069742));
#48603=CARTESIAN_POINT('Ctrl Pts',(3.04732282720845,-9.6,107.916357855643));
#48604=CARTESIAN_POINT('Ctrl Pts',(3.0550860205024,-9.6,107.916727456368));
#48605=CARTESIAN_POINT('Ctrl Pts',(3.06284700521599,-9.6,107.917358017175));
#48606=CARTESIAN_POINT('Ctrl Pts',(3.07059229349538,-9.6,107.918245921928));
#48607=CARTESIAN_POINT('Ctrl Pts',(3.07645289849991,-9.6,107.918917770264));
#48608=CARTESIAN_POINT('Ctrl Pts',(3.08229730575072,-9.6,107.919736283014));
#48609=CARTESIAN_POINT('Ctrl Pts',(3.08811244646604,-9.6,107.92069772171));
#48610=CARTESIAN_POINT('Ctrl Pts',(3.10788527884949,-9.6,107.92396683713));
#48611=CARTESIAN_POINT('Ctrl Pts',(3.1273446475303,-9.6,107.928887258058));
#48612=CARTESIAN_POINT('Ctrl Pts',(3.14626667162367,-9.6,107.935377526743));
#48613=CARTESIAN_POINT('Ctrl Pts',(3.15848777788601,-9.6,107.939569375505));
#48614=CARTESIAN_POINT('Ctrl Pts',(3.17048510749447,-9.6,107.944417154964));
#48615=CARTESIAN_POINT('Ctrl Pts',(3.18219822161691,-9.6,107.949910387659));
#48616=CARTESIAN_POINT('Ctrl Pts',(3.18735667522611,-9.6,107.95232960647));
#48617=CARTESIAN_POINT('Ctrl Pts',(3.19245998065074,-9.6,107.954874127728));
#48618=CARTESIAN_POINT('Ctrl Pts',(3.19750279605545,-9.6,107.957543597182));
#48619=CARTESIAN_POINT('Ctrl Pts',(3.20191914257529,-9.6,107.959881438485));
#48620=CARTESIAN_POINT('Ctrl Pts',(3.20628611153622,-9.6,107.962313705682));
#48621=CARTESIAN_POINT('Ctrl Pts',(3.21059155521031,-9.6,107.964834412739));
#48622=CARTESIAN_POINT('Ctrl Pts',(3.22417397784133,-9.6,107.9727865104));
#48623=CARTESIAN_POINT('Ctrl Pts',(3.2371700909409,-9.6,107.981630931996));
#48624=CARTESIAN_POINT('Ctrl Pts',(3.24947753805501,-9.6,107.991337449338));
#48625=CARTESIAN_POINT('Ctrl Pts',(3.26144617364877,-9.6,108.000776756114));
#48626=CARTESIAN_POINT('Ctrl Pts',(3.27276398520879,-9.6,108.011031382882));
#48627=CARTESIAN_POINT('Ctrl Pts',(3.28339510187528,-9.6,108.02200369201));
#48628=CARTESIAN_POINT('Ctrl Pts',(3.2894425301682,-9.6,108.02824520499));
#48629=CARTESIAN_POINT('Ctrl Pts',(3.29526760808024,-9.6,108.034719247612));
#48630=CARTESIAN_POINT('Ctrl Pts',(3.3008622810014,-9.6,108.041409871992));
#48631=CARTESIAN_POINT('Ctrl Pts',(3.30502766752572,-9.6,108.046391224258));
#48632=CARTESIAN_POINT('Ctrl Pts',(3.30906699199165,-9.6,108.051495376588));
#48633=CARTESIAN_POINT('Ctrl Pts',(3.31296183144936,-9.6,108.056695204982));
#48634=CARTESIAN_POINT('Ctrl Pts',(3.32548548455846,-9.6,108.07341498194));
#48635=CARTESIAN_POINT('Ctrl Pts',(3.33655220478908,-9.6,108.091159138622));
#48636=CARTESIAN_POINT('Ctrl Pts',(3.34607870297481,-9.6,108.109684473486));
#48637=CARTESIAN_POINT('Ctrl Pts',(3.35059666448507,-9.6,108.118470151944));
#48638=CARTESIAN_POINT('Ctrl Pts',(3.35476778148254,-9.6,108.127432195746));
#48639=CARTESIAN_POINT('Ctrl Pts',(3.35858042570842,-9.6,108.136547646305));
#48640=CARTESIAN_POINT('Ctrl Pts',(3.36323661049533,-9.6,108.147679873628));
#48641=CARTESIAN_POINT('Ctrl Pts',(3.36735832511144,-9.6,108.159040884373));
#48642=CARTESIAN_POINT('Ctrl Pts',(3.37093902375822,-9.6,108.170594501883));
#48643=CARTESIAN_POINT('Ctrl Pts',(3.3725349679066,-9.6,108.175744035556));
#48644=CARTESIAN_POINT('Ctrl Pts',(3.37402327625765,-9.6,108.180932309664));
#48645=CARTESIAN_POINT('Ctrl Pts',(3.37539961282126,-9.6,108.18614094522));
#48646=CARTESIAN_POINT('Ctrl Pts',(3.38089186464593,-9.6,108.206925932622));
#48647=CARTESIAN_POINT('Ctrl Pts',(3.38462307558806,-9.6,108.228089606938));
#48648=CARTESIAN_POINT('Ctrl Pts',(3.38659117017677,-9.6,108.249415616141));
#48649=CARTESIAN_POINT('Ctrl Pts',(3.38856090362137,-9.6,108.270759383766));
#48650=CARTESIAN_POINT('Ctrl Pts',(3.38876502618137,-9.6,108.292267093563));
#48651=CARTESIAN_POINT('Ctrl Pts',(3.38715357967984,-9.6,108.313739432014));
#48652=CARTESIAN_POINT('Ctrl Pts',(3.38688804448339,-9.6,108.317277657828));
#48653=CARTESIAN_POINT('Ctrl Pts',(3.38657309767225,-9.6,108.320814935752));
#48654=CARTESIAN_POINT('Ctrl Pts',(3.38620837767256,-9.6,108.324350380063));
#48655=CARTESIAN_POINT('Ctrl Pts',(3.38620837767256,-9.6,108.324350380063));
#48656=CARTESIAN_POINT('Ctrl Pts',(3.39852125534571,-9.59670537100196,108.26039191063));
#48657=CARTESIAN_POINT('Ctrl Pts',(3.39446951389991,-9.59341074200393,108.193571179767));
#48658=CARTESIAN_POINT('Ctrl Pts',(3.37489886333973,-9.59011611300589,108.131384606091));
#48659=CARTESIAN_POINT('Ctrl Pts',(3.35532821277956,-9.58682148400785,108.069198032416));
#48660=CARTESIAN_POINT('Ctrl Pts',(3.320238653105,-9.58352685500982,108.011645615927));
#48661=CARTESIAN_POINT('Ctrl Pts',(3.2732668210428,-9.58023222601178,107.9666723165));
#48662=CARTESIAN_POINT('Ctrl Pts',(3.17932315691838,-9.5736429680157,107.876725717647));
#48663=CARTESIAN_POINT('Ctrl Pts',(3.03785040324334,-9.56705371001963,107.83709558704));
#48664=CARTESIAN_POINT('Ctrl Pts',(2.91166778666605,-9.56046445202356,107.86611798927));
#48665=CARTESIAN_POINT('Ctrl Pts',(2.78548517008876,-9.55387519402749,107.895140391501));
#48666=CARTESIAN_POINT('Ctrl Pts',(2.67459269060921,-9.54728593603141,107.992815326569));
#48667=CARTESIAN_POINT('Ctrl Pts',(2.62994233320224,-9.54069667803534,108.114618751353));
#48668=CARTESIAN_POINT('Ctrl Pts',(2.61417555827885,-9.53836990275806,108.157629542195));
#48669=CARTESIAN_POINT('Ctrl Pts',(2.60666859404062,-9.53604312748078,108.203648943736));
#48670=CARTESIAN_POINT('Ctrl Pts',(2.60697877099099,-9.5337163522035,108.249759674367));
#48671=CARTESIAN_POINT('Origin',(3.35,-7.7,108.25));
#48672=CARTESIAN_POINT('',(2.65,-7.7,108.25));
#48673=CARTESIAN_POINT('Origin',(3.,-7.7,108.25));
#48674=CARTESIAN_POINT('Origin',(3.,-7.725,108.25));
#48675=CARTESIAN_POINT('',(2.625,-7.725,108.25));
#48676=CARTESIAN_POINT('Origin',(3.,-8.675,108.25));
#48677=CARTESIAN_POINT('Origin',(3.,-9.6,108.25));
#48678=CARTESIAN_POINT('Origin',(3.9,-9.6,108.25));
#48679=CARTESIAN_POINT('',(2.1,-9.6,108.25));
#48680=CARTESIAN_POINT('Origin',(3.,-9.6,108.25));
#48681=CARTESIAN_POINT('Origin',(3.,-9.7,108.25));
#48682=CARTESIAN_POINT('',(2.,-9.7,108.25));
#48683=CARTESIAN_POINT('Origin',(3.,-11.1,108.25));
#48684=CARTESIAN_POINT('',(2.,-11.2,108.25));
#48685=CARTESIAN_POINT('Origin',(3.,-11.2,108.25));
#48686=CARTESIAN_POINT('',(1.95,-11.1,108.25));
#48687=CARTESIAN_POINT('Origin',(3.,-11.2,108.25));
#48688=CARTESIAN_POINT('',(0.,0.,0.));
#48689=CARTESIAN_POINT('Origin',(-8.5,0.,109.7));
#48690=CARTESIAN_POINT('',(-8.9,-4.89858719658942E-17,112.75));
#48691=CARTESIAN_POINT('Origin',(-8.5,0.,112.75));
#48692=CARTESIAN_POINT('',(-8.9,-4.89858719658942E-17,109.7));
#48693=CARTESIAN_POINT('',(-8.9,-4.89858719658942E-17,109.7));
#48694=CARTESIAN_POINT('Origin',(-8.5,0.,109.7));
#48695=CARTESIAN_POINT('Origin',(-8.5,0.,109.7));
#48696=CARTESIAN_POINT('Origin',(-8.5,0.,113.95));
#48697=CARTESIAN_POINT('',(-8.09585481156726,-0.7,113.95));
#48698=CARTESIAN_POINT('',(-7.69170962313452,0.,113.95));
#48699=CARTESIAN_POINT('',(-8.09585481156726,-0.7,113.95));
#48700=CARTESIAN_POINT('',(-8.09585481156726,0.7,113.95));
#48701=CARTESIAN_POINT('',(-7.69170962313452,0.,113.95));
#48702=CARTESIAN_POINT('',(-8.90414518843274,0.7,113.95));
#48703=CARTESIAN_POINT('',(-8.09585481156726,0.7,113.95));
#48704=CARTESIAN_POINT('',(-9.30829037686548,1.11022302462516E-16,113.95));
#48705=CARTESIAN_POINT('',(-8.90414518843274,0.7,113.95));
#48706=CARTESIAN_POINT('',(-8.90414518843274,-0.7,113.95));
#48707=CARTESIAN_POINT('',(-9.30829037686548,9.89870222809913E-17,113.95));
#48708=CARTESIAN_POINT('',(-8.90414518843274,-0.7,113.95));
#48709=CARTESIAN_POINT('',(-9.1,-7.34788079488412E-17,113.95));
#48710=CARTESIAN_POINT('Origin',(-8.5,0.,113.95));
#48711=CARTESIAN_POINT('Origin',(-8.90414518843274,-0.7,112.75));
#48712=CARTESIAN_POINT('',(-8.90414518843274,-0.7,112.75));
#48713=CARTESIAN_POINT('',(-8.09585481156726,-0.7,112.75));
#48714=CARTESIAN_POINT('',(-8.90414518843274,-0.7,112.75));
#48715=CARTESIAN_POINT('',(-8.09585481156726,-0.7,112.75));
#48716=CARTESIAN_POINT('',(-8.90414518843274,-0.7,112.75));
#48717=CARTESIAN_POINT('Origin',(-9.30829037686548,9.89870222809913E-17,
112.75));
#48718=CARTESIAN_POINT('',(-9.30829037686548,9.89870222809913E-17,112.75));
#48719=CARTESIAN_POINT('',(-9.30829037686548,9.89870222809913E-17,112.75));
#48720=CARTESIAN_POINT('',(-9.30829037686548,9.89870222809913E-17,112.75));
#48721=CARTESIAN_POINT('Origin',(-8.90414518843274,0.7,112.75));
#48722=CARTESIAN_POINT('',(-8.90414518843274,0.7,112.75));
#48723=CARTESIAN_POINT('',(-8.90414518843274,0.7,112.75));
#48724=CARTESIAN_POINT('',(-8.90414518843274,0.7,112.75));
#48725=CARTESIAN_POINT('Origin',(-8.09585481156726,0.7,112.75));
#48726=CARTESIAN_POINT('',(-8.09585481156726,0.7,112.75));
#48727=CARTESIAN_POINT('',(-8.09585481156726,0.7,112.75));
#48728=CARTESIAN_POINT('',(-8.09585481156726,0.7,112.75));
#48729=CARTESIAN_POINT('Origin',(-7.69170962313452,0.,112.75));
#48730=CARTESIAN_POINT('',(-7.69170962313452,0.,112.75));
#48731=CARTESIAN_POINT('',(-7.69170962313452,0.,112.75));
#48732=CARTESIAN_POINT('',(-7.69170962313452,0.,112.75));
#48733=CARTESIAN_POINT('Origin',(-8.09585481156726,-0.7,112.75));
#48734=CARTESIAN_POINT('',(-8.09585481156726,-0.7,112.75));
#48735=CARTESIAN_POINT('Origin',(-8.5,0.,112.75));
#48736=CARTESIAN_POINT('Origin',(-8.5,0.,115.4));
#48737=CARTESIAN_POINT('',(-7.94098300562502,-0.217944947176943,115.4));
#48738=CARTESIAN_POINT('',(-7.94098300562502,0.217944947176943,115.4));
#48739=CARTESIAN_POINT('',(-7.94098300562502,0.,115.4));
#48740=CARTESIAN_POINT('Origin',(-8.5,0.,115.4));
#48741=CARTESIAN_POINT('Origin',(-8.5,0.,115.4));
#48742=CARTESIAN_POINT('',(-9.05901699437498,0.217944947176943,115.4));
#48743=CARTESIAN_POINT('',(-9.05901699437498,-0.217944947176943,115.4));
#48744=CARTESIAN_POINT('',(-9.05901699437498,0.,115.4));
#48745=CARTESIAN_POINT('',(-9.1,-7.34788079488412E-17,115.4));
#48746=CARTESIAN_POINT('Origin',(-8.5,0.,115.4));
#48747=CARTESIAN_POINT('Origin',(-8.5,0.,115.4));
#48748=CARTESIAN_POINT('Origin',(-8.5,0.,113.95));
#48749=CARTESIAN_POINT('Ctrl Pts',(-9.05901699437498,-0.217944947176941,
115.4));
#48750=CARTESIAN_POINT('Ctrl Pts',(-9.05746114535787,-0.221935615703616,
115.399719436761));
#48751=CARTESIAN_POINT('Ctrl Pts',(-9.05586245181257,-0.225909893277269,
115.399432356204));
#48752=CARTESIAN_POINT('Ctrl Pts',(-9.02357718014127,-0.303751656945718,
115.393661962552));
#48753=CARTESIAN_POINT('Ctrl Pts',(-8.97743240350865,-0.371095733915202,
115.385929127254));
#48754=CARTESIAN_POINT('Ctrl Pts',(-8.87109817623925,-0.477429961184608,
115.371475590715));
#48755=CARTESIAN_POINT('Ctrl Pts',(-8.80375305869836,-0.523576651819584,
115.363804435153));
#48756=CARTESIAN_POINT('Ctrl Pts',(-8.65597871120912,-0.584866716033612,
115.352992026863));
#48757=CARTESIAN_POINT('Ctrl Pts',(-8.57553441616499,-0.6,115.35));
#48758=CARTESIAN_POINT('Ctrl Pts',(-8.42446558383501,-0.6,115.35));
#48759=CARTESIAN_POINT('Ctrl Pts',(-8.34402128879088,-0.584866716033612,
115.352992026863));
#48760=CARTESIAN_POINT('Ctrl Pts',(-8.19624694130164,-0.523576651819584,
115.363804435153));
#48761=CARTESIAN_POINT('Ctrl Pts',(-8.12890182376075,-0.477429961184608,
115.371475590715));
#48762=CARTESIAN_POINT('Ctrl Pts',(-8.02256759649135,-0.371095733915202,
115.385929127254));
#48763=CARTESIAN_POINT('Ctrl Pts',(-7.97642281985873,-0.303751656945718,
115.393661962552));
#48764=CARTESIAN_POINT('Ctrl Pts',(-7.94413754818743,-0.225909893277269,
115.399432356204));
#48765=CARTESIAN_POINT('Ctrl Pts',(-7.94253885464213,-0.221935615703617,
115.399719436761));
#48766=CARTESIAN_POINT('Ctrl Pts',(-7.94098300562502,-0.217944947176942,
115.4));
#48767=CARTESIAN_POINT('',(-9.1,-7.34788079488412E-17,113.95));
#48768=CARTESIAN_POINT('Ctrl Pts',(-7.94098300562502,0.217944947176942,
115.4));
#48769=CARTESIAN_POINT('Ctrl Pts',(-7.94253885464213,0.221935615703616,
115.399719436761));
#48770=CARTESIAN_POINT('Ctrl Pts',(-7.94413754818743,0.225909893277269,
115.399432356204));
#48771=CARTESIAN_POINT('Ctrl Pts',(-7.97642281985873,0.303751656945718,
115.393661962552));
#48772=CARTESIAN_POINT('Ctrl Pts',(-8.02256759649135,0.371095733915202,
115.385929127254));
#48773=CARTESIAN_POINT('Ctrl Pts',(-8.12890182376075,0.477429961184608,
115.371475590715));
#48774=CARTESIAN_POINT('Ctrl Pts',(-8.19624694130164,0.523576651819582,
115.363804435153));
#48775=CARTESIAN_POINT('Ctrl Pts',(-8.34402128879088,0.584866716033611,
115.352992026863));
#48776=CARTESIAN_POINT('Ctrl Pts',(-8.42446558383501,0.6,115.35));
#48777=CARTESIAN_POINT('Ctrl Pts',(-8.57553441616499,0.6,115.35));
#48778=CARTESIAN_POINT('Ctrl Pts',(-8.65597871120912,0.584866716033612,
115.352992026863));
#48779=CARTESIAN_POINT('Ctrl Pts',(-8.80375305869836,0.523576651819584,
115.363804435153));
#48780=CARTESIAN_POINT('Ctrl Pts',(-8.87109817623925,0.477429961184608,
115.371475590715));
#48781=CARTESIAN_POINT('Ctrl Pts',(-8.97743240350865,0.371095733915202,
115.385929127254));
#48782=CARTESIAN_POINT('Ctrl Pts',(-9.02357718014127,0.30375165694572,115.393661962552));
#48783=CARTESIAN_POINT('Ctrl Pts',(-9.05586245181257,0.22590989327727,115.399432356204));
#48784=CARTESIAN_POINT('Ctrl Pts',(-9.05746114535787,0.221935615703616,
115.399719436761));
#48785=CARTESIAN_POINT('Ctrl Pts',(-9.05901699437498,0.217944947176941,
115.4));
#48786=CARTESIAN_POINT('Origin',(-8.5,-1.5,118.5));
#48787=CARTESIAN_POINT('',(-8.68357599741213,-1.5,118.737275900955));
#48788=CARTESIAN_POINT('',(-8.20011630702142,-1.5,118.491647115137));
#48789=CARTESIAN_POINT('Origin',(-8.5,-1.5,118.5));
#48790=CARTESIAN_POINT('',(-8.68357599741213,-1.6,118.737275900955));
#48791=CARTESIAN_POINT('',(-8.68357599741213,-1.5,118.737275900955));
#48792=CARTESIAN_POINT('',(-8.20011630702142,-1.6,118.491647115137));
#48793=CARTESIAN_POINT('Origin',(-8.5,-1.6,118.5));
#48794=CARTESIAN_POINT('',(-8.20011630702142,-1.5,118.491647115137));
#48795=CARTESIAN_POINT('Origin',(-8.07858983848623,-1.5,118.429903810568));
#48796=CARTESIAN_POINT('',(-8.07858983848623,-1.5,118.429903810568));
#48797=CARTESIAN_POINT('',(-7.10771361113469,-1.5,117.936635905003));
#48798=CARTESIAN_POINT('',(-8.07858983848623,-1.6,118.429903810568));
#48799=CARTESIAN_POINT('',(-8.07858983848623,-1.6,118.429903810568));
#48800=CARTESIAN_POINT('',(-8.07858983848623,-1.5,118.429903810568));
#48801=CARTESIAN_POINT('Origin',(-8.22858983848623,-1.5,118.170096189432));
#48802=CARTESIAN_POINT('',(-8.22858983848623,-1.5,118.170096189432));
#48803=CARTESIAN_POINT('',(-7.82858983848618,-1.5,118.86291651246));
#48804=CARTESIAN_POINT('',(-8.22858983848623,-1.6,118.170096189432));
#48805=CARTESIAN_POINT('',(-8.22858983848623,-1.6,118.170096189432));
#48806=CARTESIAN_POINT('',(-8.22858983848623,-1.5,118.170096189432));
#48807=CARTESIAN_POINT('Origin',(-8.34282434302488,-1.5,118.244469546131));
#48808=CARTESIAN_POINT('',(-8.34282434302488,-1.5,118.244469546131));
#48809=CARTESIAN_POINT('',(-7.43809082420648,-1.5,117.655435007187));
#48810=CARTESIAN_POINT('',(-8.34282434302488,-1.6,118.244469546131));
#48811=CARTESIAN_POINT('',(-10.5784609690827,-1.6,119.7));
#48812=CARTESIAN_POINT('',(-8.34282434302488,-1.5,118.244469546131));
#48813=CARTESIAN_POINT('Origin',(-8.5,-1.5,118.5));
#48814=CARTESIAN_POINT('',(-8.79727495663918,-1.5,118.540343526806));
#48815=CARTESIAN_POINT('Origin',(-8.5,-1.5,118.5));
#48816=CARTESIAN_POINT('',(-8.79727495663918,-1.6,118.540343526806));
#48817=CARTESIAN_POINT('Origin',(-8.5,-1.6,118.5));
#48818=CARTESIAN_POINT('',(-8.79727495663918,-1.5,118.540343526806));
#48819=CARTESIAN_POINT('Origin',(-10.5784609690827,-1.5,119.7));
#48820=CARTESIAN_POINT('',(-10.5784609690827,-1.5,119.7));
#48821=CARTESIAN_POINT('',(-8.55590913723536,-1.5,118.383200234122));
#48822=CARTESIAN_POINT('',(-10.5784609690827,-1.6,119.7));
#48823=CARTESIAN_POINT('',(-10.5784609690827,-1.6,119.7));
#48824=CARTESIAN_POINT('',(-10.5784609690827,-1.5,119.7));
#48825=CARTESIAN_POINT('Origin',(-8.68357599741213,-1.5,118.737275900955));
#48826=CARTESIAN_POINT('',(-7.41020669059764,-1.5,118.090321950197));
#48827=CARTESIAN_POINT('',(-8.07858983848623,-1.6,118.429903810568));
#48828=CARTESIAN_POINT('Origin',(-9.32852540378444,-1.6,118.935048094716));
#48829=CARTESIAN_POINT('Origin',(-5.95068842566558,-1.5,117.60859072421));
#48830=CARTESIAN_POINT('',(-5.95068842566558,-1.5,117.60859072421));
#48831=CARTESIAN_POINT('',(-6.28355820636889,-1.5,117.716746672241));
#48832=CARTESIAN_POINT('',(-5.92307740174221,-1.5,117.599619358704));
#48833=CARTESIAN_POINT('',(-5.95068842566558,-1.45,117.60859072421));
#48834=CARTESIAN_POINT('',(-5.95068842566558,-1.5,117.60859072421));
#48835=CARTESIAN_POINT('',(-6.28355820636889,-1.45,117.716746672241));
#48836=CARTESIAN_POINT('',(-5.95068842566558,-1.45,117.60859072421));
#48837=CARTESIAN_POINT('',(-6.28355820636889,-1.5,117.716746672241));
#48838=CARTESIAN_POINT('Origin',(-5.91360638634059,-1.5,117.722717506165));
#48839=CARTESIAN_POINT('',(-5.91360638634059,-1.5,117.722717506165));
#48840=CARTESIAN_POINT('',(-5.78441421709369,-1.5,118.120330118589));
#48841=CARTESIAN_POINT('',(-5.91360638634059,-1.45,117.722717506165));
#48842=CARTESIAN_POINT('',(-5.91360638634059,-1.5,117.722717506165));
#48843=CARTESIAN_POINT('',(-5.91360638634059,-1.45,117.722717506165));
#48844=CARTESIAN_POINT('Origin',(-6.24647616704389,-1.5,117.830873454197));
#48845=CARTESIAN_POINT('',(-6.24647616704389,-1.5,117.830873454197));
#48846=CARTESIAN_POINT('',(-6.05243025276885,-1.5,117.767824114675));
#48847=CARTESIAN_POINT('',(-6.24647616704389,-1.45,117.830873454197));
#48848=CARTESIAN_POINT('',(-6.24647616704389,-1.5,117.830873454197));
#48849=CARTESIAN_POINT('',(-6.24647616704389,-1.45,117.830873454197));
#48850=CARTESIAN_POINT('Origin',(-6.28355820636889,-1.5,117.716746672241));
#48851=CARTESIAN_POINT('',(-6.13582501745948,-1.5,118.171422675642));
#48852=CARTESIAN_POINT('',(-6.28355820636889,-1.45,117.716746672241));
#48853=CARTESIAN_POINT('Origin',(-6.09858229635474,-1.45,117.719732089203));
#48854=CARTESIAN_POINT('Origin',(-6.28038700005009,-1.5,120.038479161527));
#48855=CARTESIAN_POINT('',(-6.28038700005009,-1.5,120.038479161527));
#48856=CARTESIAN_POINT('',(-6.56354294808132,-1.5,119.832754323225));
#48857=CARTESIAN_POINT('',(-6.42352262153444,-1.5,119.934485045246));
#48858=CARTESIAN_POINT('',(-6.28038700005009,-1.45,120.038479161527));
#48859=CARTESIAN_POINT('',(-6.28038700005009,-1.5,120.038479161527));
#48860=CARTESIAN_POINT('',(-6.56354294808132,-1.45,119.832754323225));
#48861=CARTESIAN_POINT('',(-6.28038700005009,-1.45,120.038479161527));
#48862=CARTESIAN_POINT('',(-6.56354294808132,-1.5,119.832754323225));
#48863=CARTESIAN_POINT('Origin',(-6.35092123032519,-1.5,120.135561200852));
#48864=CARTESIAN_POINT('',(-6.35092123032519,-1.5,120.135561200852));
#48865=CARTESIAN_POINT('',(-5.83232499367828,-1.5,119.421774716707));
#48866=CARTESIAN_POINT('',(-6.35092123032519,-1.45,120.135561200852));
#48867=CARTESIAN_POINT('',(-6.35092123032519,-1.5,120.135561200852));
#48868=CARTESIAN_POINT('',(-6.35092123032519,-1.45,120.135561200852));
#48869=CARTESIAN_POINT('Origin',(-6.63407717835642,-1.5,119.92983636255));
#48870=CARTESIAN_POINT('',(-6.63407717835642,-1.5,119.92983636255));
#48871=CARTESIAN_POINT('',(-6.63563482582516,-1.5,119.92870466542));
#48872=CARTESIAN_POINT('',(-6.63407717835642,-1.45,119.92983636255));
#48873=CARTESIAN_POINT('',(-6.63407717835642,-1.5,119.92983636255));
#48874=CARTESIAN_POINT('',(-6.63407717835642,-1.45,119.92983636255));
#48875=CARTESIAN_POINT('Origin',(-6.56354294808132,-1.5,119.832754323225));
#48876=CARTESIAN_POINT('',(-6.08021382657196,-1.5,119.167508858742));
#48877=CARTESIAN_POINT('',(-6.56354294808132,-1.45,119.832754323225));
#48878=CARTESIAN_POINT('Origin',(-6.45723208920326,-1.45,119.984157762038));
#48879=CARTESIAN_POINT('Origin',(-10.4516147160749,-1.5,116.633238097668));
#48880=CARTESIAN_POINT('',(-10.4516147160749,-1.5,116.633238097668));
#48881=CARTESIAN_POINT('',(-10.0273506473629,-1.5,117.057502166379));
#48882=CARTESIAN_POINT('',(-8.77202056147305,-1.5,118.312832252269));
#48883=CARTESIAN_POINT('',(-10.4516147160749,-1.45,116.633238097668));
#48884=CARTESIAN_POINT('',(-10.4516147160749,-1.5,116.633238097668));
#48885=CARTESIAN_POINT('',(-10.0273506473629,-1.45,117.057502166379));
#48886=CARTESIAN_POINT('',(-10.4516147160749,-1.45,116.633238097668));
#48887=CARTESIAN_POINT('',(-10.0273506473629,-1.5,117.057502166379));
#48888=CARTESIAN_POINT('Origin',(-10.3667619023325,-1.5,116.548385283925));
#48889=CARTESIAN_POINT('',(-10.3667619023325,-1.5,116.548385283925));
#48890=CARTESIAN_POINT('',(-9.66297510576788,-1.5,115.844598487361));
#48891=CARTESIAN_POINT('',(-10.3667619023325,-1.45,116.548385283925));
#48892=CARTESIAN_POINT('',(-10.3667619023325,-1.5,116.548385283925));
#48893=CARTESIAN_POINT('',(-10.3667619023325,-1.45,116.548385283925));
#48894=CARTESIAN_POINT('Origin',(-9.94249783362056,-1.5,116.972649352637));
#48895=CARTESIAN_POINT('',(-9.94249783362056,-1.5,116.972649352637));
#48896=CARTESIAN_POINT('',(-8.4750357133747,-1.5,118.440111472883));
#48897=CARTESIAN_POINT('',(-9.94249783362056,-1.45,116.972649352637));
#48898=CARTESIAN_POINT('',(-9.94249783362056,-1.5,116.972649352637));
#48899=CARTESIAN_POINT('',(-9.94249783362056,-1.45,116.972649352637));
#48900=CARTESIAN_POINT('Origin',(-10.0273506473629,-1.5,117.057502166379));
#48901=CARTESIAN_POINT('',(-9.28113744392716,-1.5,116.311288962944));
#48902=CARTESIAN_POINT('',(-10.0273506473629,-1.45,117.057502166379));
#48903=CARTESIAN_POINT('Origin',(-10.1970562748477,-1.45,116.802943725152));
#48904=CARTESIAN_POINT('Origin',(-9.67231395784547,-1.5,120.932957045293));
#48905=CARTESIAN_POINT('',(-9.67231395784547,-1.5,120.932957045293));
#48906=CARTESIAN_POINT('',(-9.39991965800175,-1.5,120.39835313078));
#48907=CARTESIAN_POINT('',(-8.76057109110912,-1.5,119.143560916717));
#48908=CARTESIAN_POINT('',(-9.67231395784547,-1.45,120.932957045293));
#48909=CARTESIAN_POINT('',(-9.67231395784547,-1.5,120.932957045293));
#48910=CARTESIAN_POINT('',(-9.39991965800175,-1.45,120.39835313078));
#48911=CARTESIAN_POINT('',(-9.67231395784547,-1.45,120.932957045293));
#48912=CARTESIAN_POINT('',(-9.39991965800175,-1.5,120.39835313078));
#48913=CARTESIAN_POINT('Origin',(-9.77923474074808,-1.5,120.878478185324));
#48914=CARTESIAN_POINT('',(-9.77923474074808,-1.5,120.878478185324));
#48915=CARTESIAN_POINT('',(-8.60136023711026,-1.5,121.478635221238));
#48916=CARTESIAN_POINT('',(-9.77923474074808,-1.45,120.878478185324));
#48917=CARTESIAN_POINT('',(-9.77923474074808,-1.5,120.878478185324));
#48918=CARTESIAN_POINT('',(-9.77923474074808,-1.45,120.878478185324));
#48919=CARTESIAN_POINT('Origin',(-9.50684044090435,-1.5,120.343874270811));
#48920=CARTESIAN_POINT('',(-9.50684044090435,-1.5,120.343874270811));
#48921=CARTESIAN_POINT('',(-8.73129472408986,-1.5,118.821780099492));
#48922=CARTESIAN_POINT('',(-9.50684044090435,-1.45,120.343874270811));
#48923=CARTESIAN_POINT('',(-9.50684044090435,-1.5,120.343874270811));
#48924=CARTESIAN_POINT('',(-9.50684044090435,-1.45,120.343874270811));
#48925=CARTESIAN_POINT('Origin',(-9.39991965800175,-1.5,120.39835313078));
#48926=CARTESIAN_POINT('',(-8.27550554581525,-1.5,120.97127073671));
#48927=CARTESIAN_POINT('',(-9.39991965800175,-1.45,120.39835313078));
#48928=CARTESIAN_POINT('Origin',(-9.58957719937491,-1.45,120.638415658052));
#48929=CARTESIAN_POINT('Origin',(-11.1573724517045,-1.5,118.981634356044));
#48930=CARTESIAN_POINT('',(-11.1573724517045,-1.5,118.981634356044));
#48931=CARTESIAN_POINT('',(-10.5647594473474,-1.5,118.88777367702));
#48932=CARTESIAN_POINT('',(-8.40947721758703,-1.5,118.546410507318));
#48933=CARTESIAN_POINT('',(-11.1573724517045,-1.45,118.981634356044));
#48934=CARTESIAN_POINT('',(-11.1573724517045,-1.5,118.981634356044));
#48935=CARTESIAN_POINT('',(-10.5647594473474,-1.45,118.88777367702));
#48936=CARTESIAN_POINT('',(-11.1573724517045,-1.45,118.981634356044));
#48937=CARTESIAN_POINT('',(-10.5647594473474,-1.5,118.88777367702));
#48938=CARTESIAN_POINT('Origin',(-11.1761445875093,-1.5,118.863111755173));
#48939=CARTESIAN_POINT('',(-11.1761445875093,-1.5,118.863111755173));
#48940=CARTESIAN_POINT('',(-11.1359675278721,-1.5,119.116779726312));
#48941=CARTESIAN_POINT('',(-11.1761445875093,-1.45,118.863111755173));
#48942=CARTESIAN_POINT('',(-11.1761445875093,-1.5,118.863111755173));
#48943=CARTESIAN_POINT('',(-11.1761445875093,-1.45,118.863111755173));
#48944=CARTESIAN_POINT('Origin',(-10.5835315831522,-1.5,118.769251076149));
#48945=CARTESIAN_POINT('',(-10.5835315831522,-1.5,118.769251076149));
#48946=CARTESIAN_POINT('',(-8.1319428512133,-1.5,118.380957566935));
#48947=CARTESIAN_POINT('',(-10.5835315831522,-1.45,118.769251076149));
#48948=CARTESIAN_POINT('',(-10.5835315831522,-1.5,118.769251076149));
#48949=CARTESIAN_POINT('',(-10.5835315831522,-1.45,118.769251076149));
#48950=CARTESIAN_POINT('Origin',(-10.5647594473474,-1.5,118.88777367702));
#48951=CARTESIAN_POINT('',(-10.5339684556126,-1.5,119.082180347724));
#48952=CARTESIAN_POINT('',(-10.5647594473474,-1.45,118.88777367702));
#48953=CARTESIAN_POINT('Origin',(-10.8704520174283,-1.45,118.875442716097));
#48954=CARTESIAN_POINT('Origin',(-11.0863936136594,-1.5,117.722717506165));
#48955=CARTESIAN_POINT('',(-11.0863936136594,-1.5,117.722717506165));
#48956=CARTESIAN_POINT('',(-10.7535238329561,-1.5,117.830873454197));
#48957=CARTESIAN_POINT('',(-8.4909299957391,-1.5,118.566034756484));
#48958=CARTESIAN_POINT('',(-11.0863936136594,-1.45,117.722717506165));
#48959=CARTESIAN_POINT('',(-11.0863936136594,-1.5,117.722717506165));
#48960=CARTESIAN_POINT('',(-10.7535238329561,-1.45,117.830873454197));
#48961=CARTESIAN_POINT('',(-11.0863936136594,-1.45,117.722717506165));
#48962=CARTESIAN_POINT('',(-10.7535238329561,-1.5,117.830873454197));
#48963=CARTESIAN_POINT('Origin',(-11.0493115743344,-1.5,117.60859072421));
#48964=CARTESIAN_POINT('',(-11.0493115743344,-1.5,117.60859072421));
#48965=CARTESIAN_POINT('',(-10.9201194050875,-1.5,117.210978111787));
#48966=CARTESIAN_POINT('',(-11.0493115743344,-1.45,117.60859072421));
#48967=CARTESIAN_POINT('',(-11.0493115743344,-1.5,117.60859072421));
#48968=CARTESIAN_POINT('',(-11.0493115743344,-1.45,117.60859072421));
#48969=CARTESIAN_POINT('Origin',(-10.7164417936311,-1.5,117.716746672241));
#48970=CARTESIAN_POINT('',(-10.7164417936311,-1.5,117.716746672241));
#48971=CARTESIAN_POINT('',(-8.2874130660625,-1.5,118.505985948544));
#48972=CARTESIAN_POINT('',(-10.7164417936311,-1.45,117.716746672241));
#48973=CARTESIAN_POINT('',(-10.7164417936311,-1.5,117.716746672241));
#48974=CARTESIAN_POINT('',(-10.7164417936311,-1.45,117.716746672241));
#48975=CARTESIAN_POINT('Origin',(-10.7535238329561,-1.5,117.830873454197));
#48976=CARTESIAN_POINT('',(-10.6057906440467,-1.5,117.376197450796));
#48977=CARTESIAN_POINT('',(-10.7535238329561,-1.45,117.830873454197));
#48978=CARTESIAN_POINT('Origin',(-10.9014177036453,-1.45,117.719732089203));
#48979=CARTESIAN_POINT('Origin',(-10.6490787696748,-1.5,120.135561200852));
#48980=CARTESIAN_POINT('',(-10.6490787696748,-1.5,120.135561200852));
#48981=CARTESIAN_POINT('',(-10.3659228216436,-1.5,119.92983636255));
#48982=CARTESIAN_POINT('',(-8.60786850634683,-1.5,118.652535135943));
#48983=CARTESIAN_POINT('',(-10.6490787696748,-1.45,120.135561200852));
#48984=CARTESIAN_POINT('',(-10.6490787696748,-1.5,120.135561200852));
#48985=CARTESIAN_POINT('',(-10.3659228216436,-1.45,119.92983636255));
#48986=CARTESIAN_POINT('',(-10.6490787696748,-1.45,120.135561200852));
#48987=CARTESIAN_POINT('',(-10.3659228216436,-1.5,119.92983636255));
#48988=CARTESIAN_POINT('Origin',(-10.7196129999499,-1.5,120.038479161527));
#48989=CARTESIAN_POINT('',(-10.7196129999499,-1.5,120.038479161527));
#48990=CARTESIAN_POINT('',(-10.2010167633031,-1.5,120.752265645672));
#48991=CARTESIAN_POINT('',(-10.7196129999499,-1.45,120.038479161527));
#48992=CARTESIAN_POINT('',(-10.7196129999499,-1.5,120.038479161527));
#48993=CARTESIAN_POINT('',(-10.7196129999499,-1.45,120.038479161527));
#48994=CARTESIAN_POINT('Origin',(-10.4364570519187,-1.5,119.832754323225));
#48995=CARTESIAN_POINT('',(-10.4364570519187,-1.5,119.832754323225));
#48996=CARTESIAN_POINT('',(-8.53682476260632,-1.5,118.452590677467));
#48997=CARTESIAN_POINT('',(-10.4364570519187,-1.45,119.832754323225));
#48998=CARTESIAN_POINT('',(-10.4364570519187,-1.5,119.832754323225));
#48999=CARTESIAN_POINT('',(-10.4364570519187,-1.45,119.832754323225));
#49000=CARTESIAN_POINT('Origin',(-10.3659228216436,-1.5,119.92983636255));
#49001=CARTESIAN_POINT('',(-9.88259370013425,-1.5,120.595081827033));
#49002=CARTESIAN_POINT('',(-10.3659228216436,-1.45,119.92983636255));
#49003=CARTESIAN_POINT('Origin',(-10.5427679107967,-1.45,119.984157762038));
#49004=CARTESIAN_POINT('Origin',(-8.44,-1.5,121.2));
#49005=CARTESIAN_POINT('',(-8.44,-1.5,121.2));
#49006=CARTESIAN_POINT('',(-8.44,-1.5,120.85));
#49007=CARTESIAN_POINT('',(-8.44,-1.5,119.85));
#49008=CARTESIAN_POINT('',(-8.44,-1.45,121.2));
#49009=CARTESIAN_POINT('',(-8.44,-1.5,121.2));
#49010=CARTESIAN_POINT('',(-8.44,-1.45,120.85));
#49011=CARTESIAN_POINT('',(-8.44,-1.45,121.2));
#49012=CARTESIAN_POINT('',(-8.44,-1.5,120.85));
#49013=CARTESIAN_POINT('Origin',(-8.56,-1.5,121.2));
#49014=CARTESIAN_POINT('',(-8.56,-1.5,121.2));
#49015=CARTESIAN_POINT('',(-7.08,-1.5,121.2));
#49016=CARTESIAN_POINT('',(-8.56,-1.45,121.2));
#49017=CARTESIAN_POINT('',(-8.56,-1.5,121.2));
#49018=CARTESIAN_POINT('',(-8.56,-1.45,121.2));
#49019=CARTESIAN_POINT('Origin',(-8.56,-1.5,120.85));
#49020=CARTESIAN_POINT('',(-8.56,-1.5,120.85));
#49021=CARTESIAN_POINT('',(-8.56,-1.5,119.675));
#49022=CARTESIAN_POINT('',(-8.56,-1.45,120.85));
#49023=CARTESIAN_POINT('',(-8.56,-1.5,120.85));
#49024=CARTESIAN_POINT('',(-8.56,-1.45,120.85));
#49025=CARTESIAN_POINT('Origin',(-8.44,-1.5,120.85));
#49026=CARTESIAN_POINT('',(-7.02,-1.5,120.85));
#49027=CARTESIAN_POINT('',(-8.44,-1.45,120.85));
#49028=CARTESIAN_POINT('Origin',(-8.5,-1.45,121.025));
#49029=CARTESIAN_POINT('Origin',(-7.22076525925192,-1.5,120.878478185324));
#49030=CARTESIAN_POINT('',(-7.22076525925192,-1.5,120.878478185324));
#49031=CARTESIAN_POINT('',(-7.49315955909565,-1.5,120.343874270811));
#49032=CARTESIAN_POINT('',(-7.53479674181235,-1.5,120.262156698592));
#49033=CARTESIAN_POINT('',(-7.22076525925192,-1.45,120.878478185324));
#49034=CARTESIAN_POINT('',(-7.22076525925192,-1.5,120.878478185324));
#49035=CARTESIAN_POINT('',(-7.49315955909565,-1.45,120.343874270811));
#49036=CARTESIAN_POINT('',(-7.22076525925192,-1.45,120.878478185324));
#49037=CARTESIAN_POINT('',(-7.49315955909565,-1.5,120.343874270811));
#49038=CARTESIAN_POINT('Origin',(-7.32768604215453,-1.5,120.932957045293));
#49039=CARTESIAN_POINT('',(-7.32768604215453,-1.5,120.932957045293));
#49040=CARTESIAN_POINT('',(-6.14981153851683,-1.5,120.332800009379));
#49041=CARTESIAN_POINT('',(-7.32768604215453,-1.45,120.932957045293));
#49042=CARTESIAN_POINT('',(-7.32768604215453,-1.5,120.932957045293));
#49043=CARTESIAN_POINT('',(-7.32768604215453,-1.45,120.932957045293));
#49044=CARTESIAN_POINT('Origin',(-7.60008034199825,-1.5,120.39835313078));
#49045=CARTESIAN_POINT('',(-7.60008034199825,-1.5,120.39835313078));
#49046=CARTESIAN_POINT('',(-7.77791467463682,-1.5,120.049333601304));
#49047=CARTESIAN_POINT('',(-7.60008034199825,-1.45,120.39835313078));
#49048=CARTESIAN_POINT('',(-7.60008034199825,-1.5,120.39835313078));
#49049=CARTESIAN_POINT('',(-7.60008034199825,-1.45,120.39835313078));
#49050=CARTESIAN_POINT('Origin',(-7.49315955909565,-1.5,120.343874270811));
#49051=CARTESIAN_POINT('',(-6.36874544690924,-1.5,119.770956664882));
#49052=CARTESIAN_POINT('',(-7.49315955909565,-1.45,120.343874270811));
#49053=CARTESIAN_POINT('Origin',(-7.41042280062509,-1.45,120.638415658052));
#49054=CARTESIAN_POINT('Origin',(-5.82385541249071,-1.5,118.863111755173));
#49055=CARTESIAN_POINT('',(-5.82385541249071,-1.5,118.863111755173));
#49056=CARTESIAN_POINT('',(-6.4164684168478,-1.5,118.769251076149));
#49057=CARTESIAN_POINT('',(-5.74271869798015,-1.5,118.87596254829));
#49058=CARTESIAN_POINT('',(-5.82385541249071,-1.45,118.863111755173));
#49059=CARTESIAN_POINT('',(-5.82385541249071,-1.5,118.863111755173));
#49060=CARTESIAN_POINT('',(-6.4164684168478,-1.45,118.769251076149));
#49061=CARTESIAN_POINT('',(-5.82385541249071,-1.45,118.863111755173));
#49062=CARTESIAN_POINT('',(-6.4164684168478,-1.5,118.769251076149));
#49063=CARTESIAN_POINT('Origin',(-5.84262754829554,-1.5,118.981634356044));
#49064=CARTESIAN_POINT('',(-5.84262754829554,-1.5,118.981634356044));
#49065=CARTESIAN_POINT('',(-5.80245048865833,-1.5,118.727966384905));
#49066=CARTESIAN_POINT('',(-5.84262754829554,-1.45,118.981634356044));
#49067=CARTESIAN_POINT('',(-5.84262754829554,-1.5,118.981634356044));
#49068=CARTESIAN_POINT('',(-5.84262754829554,-1.45,118.981634356044));
#49069=CARTESIAN_POINT('Origin',(-6.43524055265262,-1.5,118.88777367702));
#49070=CARTESIAN_POINT('',(-6.43524055265262,-1.5,118.88777367702));
#49071=CARTESIAN_POINT('',(-6.05779733596353,-1.5,118.94755480965));
#49072=CARTESIAN_POINT('',(-6.43524055265262,-1.45,118.88777367702));
#49073=CARTESIAN_POINT('',(-6.43524055265262,-1.5,118.88777367702));
#49074=CARTESIAN_POINT('',(-6.43524055265262,-1.45,118.88777367702));
#49075=CARTESIAN_POINT('Origin',(-6.4164684168478,-1.5,118.769251076149));
#49076=CARTESIAN_POINT('',(-6.385677425113,-1.5,118.574844405445));
#49077=CARTESIAN_POINT('',(-6.4164684168478,-1.45,118.769251076149));
#49078=CARTESIAN_POINT('Origin',(-6.12954798257167,-1.45,118.875442716097));
#49079=CARTESIAN_POINT('Origin',(-6.63323809766752,-1.5,116.548385283925));
#49080=CARTESIAN_POINT('',(-6.63323809766752,-1.5,116.548385283925));
#49081=CARTESIAN_POINT('',(-7.05750216637944,-1.5,116.972649352637));
#49082=CARTESIAN_POINT('',(-6.86283225226936,-1.5,116.777979438527));
#49083=CARTESIAN_POINT('',(-6.63323809766752,-1.45,116.548385283925));
#49084=CARTESIAN_POINT('',(-6.63323809766752,-1.5,116.548385283925));
#49085=CARTESIAN_POINT('',(-7.05750216637944,-1.45,116.972649352637));
#49086=CARTESIAN_POINT('',(-6.63323809766752,-1.45,116.548385283925));
#49087=CARTESIAN_POINT('',(-7.05750216637944,-1.5,116.972649352637));
#49088=CARTESIAN_POINT('Origin',(-6.54838528392513,-1.5,116.633238097668));
#49089=CARTESIAN_POINT('',(-6.54838528392513,-1.5,116.633238097668));
#49090=CARTESIAN_POINT('',(-5.84459848736068,-1.5,117.337024894232));
#49091=CARTESIAN_POINT('',(-6.54838528392513,-1.45,116.633238097668));
#49092=CARTESIAN_POINT('',(-6.54838528392513,-1.5,116.633238097668));
#49093=CARTESIAN_POINT('',(-6.54838528392513,-1.45,116.633238097668));
#49094=CARTESIAN_POINT('Origin',(-6.97264935263706,-1.5,117.057502166379));
#49095=CARTESIAN_POINT('',(-6.97264935263706,-1.5,117.057502166379));
#49096=CARTESIAN_POINT('',(-6.99011147288294,-1.5,117.074964286625));
#49097=CARTESIAN_POINT('',(-6.97264935263706,-1.45,117.057502166379));
#49098=CARTESIAN_POINT('',(-6.97264935263706,-1.5,117.057502166379));
#49099=CARTESIAN_POINT('',(-6.97264935263706,-1.45,117.057502166379));
#49100=CARTESIAN_POINT('Origin',(-7.05750216637944,-1.5,116.972649352637));
#49101=CARTESIAN_POINT('',(-6.31128896294379,-1.5,117.718862556073));
#49102=CARTESIAN_POINT('',(-7.05750216637944,-1.45,116.972649352637));
#49103=CARTESIAN_POINT('Origin',(-6.80294372515229,-1.45,116.802943725152));
#49104=CARTESIAN_POINT('Origin',(-5.6,-1.5,118.5));
#49105=CARTESIAN_POINT('',(-11.4,-1.5,118.5));
#49106=CARTESIAN_POINT('Origin',(-8.5,-1.5,118.5));
#49107=CARTESIAN_POINT('Origin',(-8.5,-1.625,118.5));
#49108=CARTESIAN_POINT('',(-11.4,-1.7,118.5));
#49109=CARTESIAN_POINT('',(-11.4,-1.625,118.5));
#49110=CARTESIAN_POINT('Origin',(-8.5,-1.7,118.5));
#49111=CARTESIAN_POINT('Origin',(-5.55,1.4,118.5));
#49112=CARTESIAN_POINT('',(-11.45,1.4,118.5));
#49113=CARTESIAN_POINT('Origin',(-8.5,1.4,118.5));
#49114=CARTESIAN_POINT('Origin',(-8.5,1.3,118.5));
#49115=CARTESIAN_POINT('',(-11.65,1.2,118.5));
#49116=CARTESIAN_POINT('Origin',(-8.5,1.2,118.5));
#49117=CARTESIAN_POINT('',(-11.55,1.3,118.5));
#49118=CARTESIAN_POINT('Origin',(-8.5,0.,118.5));
#49119=CARTESIAN_POINT('',(-11.65,-1.2,118.5));
#49120=CARTESIAN_POINT('Origin',(-8.5,-1.2,118.5));
#49121=CARTESIAN_POINT('',(-11.65,0.,118.5));
#49122=CARTESIAN_POINT('Origin',(-5.2,-1.2,118.5));
#49123=CARTESIAN_POINT('',(-11.8,-1.2,118.5));
#49124=CARTESIAN_POINT('Origin',(-8.5,-1.2,118.5));
#49125=CARTESIAN_POINT('Origin',(-8.5,-1.4,118.5));
#49126=CARTESIAN_POINT('',(-11.8,-1.6,118.5));
#49127=CARTESIAN_POINT('Origin',(-8.5,-1.6,118.5));
#49128=CARTESIAN_POINT('',(-11.8,-1.4,118.5));
#49129=CARTESIAN_POINT('Origin',(-8.5,-1.65,118.5));
#49130=CARTESIAN_POINT('',(-11.7,-1.7,118.5));
#49131=CARTESIAN_POINT('Origin',(-8.5,-1.7,118.5));
#49132=CARTESIAN_POINT('',(-11.75,-1.65,118.5));
#49133=CARTESIAN_POINT('Origin',(-8.5,-1.7,118.5));
#49134=CARTESIAN_POINT('',(0.,0.,0.));
#49135=CARTESIAN_POINT('Ctrl Pts',(28.7991583057917,11.,74.402898825339));
#49136=CARTESIAN_POINT('Ctrl Pts',(28.7991583057917,11.0443255072037,74.402898825339));
#49137=CARTESIAN_POINT('Ctrl Pts',(28.7965453592084,11.0915510411579,74.4116063134345));
#49138=CARTESIAN_POINT('Ctrl Pts',(28.7871669871617,11.1779078402817,74.4468238161368));
#49139=CARTESIAN_POINT('Ctrl Pts',(28.7806043669257,11.2170846527409,74.4732883033298));
#49140=CARTESIAN_POINT('Ctrl Pts',(28.7683045654192,11.2788962751735,74.5344620266402));
#49141=CARTESIAN_POINT('Ctrl Pts',(28.7617930434695,11.3057060685816,74.5732868944695));
#49142=CARTESIAN_POINT('Ctrl Pts',(28.7525231854577,11.3414465815878,74.65904064169));
#49143=CARTESIAN_POINT('Ctrl Pts',(28.7499823739105,11.3502679248349,74.7059347785805));
#49144=CARTESIAN_POINT('Ctrl Pts',(28.7499717367413,11.3503212800739,74.7941254313177));
#49145=CARTESIAN_POINT('Ctrl Pts',(28.7525477553864,11.3414466364947,74.8410052800481));
#49146=CARTESIAN_POINT('Ctrl Pts',(28.7618133828337,11.3058394721478,74.9267618361903));
#49147=CARTESIAN_POINT('Ctrl Pts',(28.7683297787118,11.2789656668451,74.9656153280843));
#49148=CARTESIAN_POINT('Ctrl Pts',(28.7806136472154,11.2174765285995,75.0267085651774));
#49149=CARTESIAN_POINT('Ctrl Pts',(28.7938779355307,11.137485266407,75.079826557824));
#49150=CARTESIAN_POINT('Ctrl Pts',(28.8019055096204,11.,75.1059958179575));
#49151=CARTESIAN_POINT('Ctrl Pts',(28.7938779355307,10.8625147335932,75.079826557824));
#49152=CARTESIAN_POINT('Ctrl Pts',(28.7806136472154,10.7825234714004,75.0267085651771));
#49153=CARTESIAN_POINT('Ctrl Pts',(28.7683297787118,10.7210343331551,74.9656153280842));
#49154=CARTESIAN_POINT('Ctrl Pts',(28.7618133828337,10.6941605278523,74.9267618361901));
#49155=CARTESIAN_POINT('Ctrl Pts',(28.7525477553864,10.6585533635054,74.8410052800478));
#49156=CARTESIAN_POINT('Ctrl Pts',(28.7499717367413,10.6496787199262,74.7941254313175));
#49157=CARTESIAN_POINT('Ctrl Pts',(28.7499823739105,10.6497320751652,74.7059347785801));
#49158=CARTESIAN_POINT('Ctrl Pts',(28.7525231854577,10.6585534184123,74.6590406416897));
#49159=CARTESIAN_POINT('Ctrl Pts',(28.7617930434695,10.6942939314186,74.5732868944692));
#49160=CARTESIAN_POINT('Ctrl Pts',(28.7683045654192,10.7211037248264,74.5344620266403));
#49161=CARTESIAN_POINT('Ctrl Pts',(28.7806043669256,10.7829153472589,74.4732883033299));
#49162=CARTESIAN_POINT('Ctrl Pts',(28.7871669871616,10.8220921597181,74.4468238161368));
#49163=CARTESIAN_POINT('Ctrl Pts',(28.7965453592083,10.9084489588421,74.4116063134345));
#49164=CARTESIAN_POINT('Ctrl Pts',(28.7991583057917,10.9556744927962,74.402898825339));
#49165=CARTESIAN_POINT('Ctrl Pts',(28.7991583057917,11.,74.402898825339));
#49166=CARTESIAN_POINT('Ctrl Pts',(28.8245239133973,11.,74.4352658835594));
#49167=CARTESIAN_POINT('Ctrl Pts',(28.8245139996716,11.0409058476698,74.4352690808426));
#49168=CARTESIAN_POINT('Ctrl Pts',(28.8222946915156,11.0844693260521,74.4435587606527));
#49169=CARTESIAN_POINT('Ctrl Pts',(28.8143446526051,11.1634798118501,74.4766846891437));
#49170=CARTESIAN_POINT('Ctrl Pts',(28.8088018057836,11.1989487338351,74.5013491133979));
#49171=CARTESIAN_POINT('Ctrl Pts',(28.7984971202627,11.2543047022451,74.5574809291687));
#49172=CARTESIAN_POINT('Ctrl Pts',(28.7930705898665,11.277994263562,74.5926796862592));
#49173=CARTESIAN_POINT('Ctrl Pts',(28.7854083939203,11.3092896913271,74.6694190769384));
#49174=CARTESIAN_POINT('Ctrl Pts',(28.783317023756,11.316933318266,74.7109865811412));
#49175=CARTESIAN_POINT('Ctrl Pts',(28.7833092717601,11.3169759220082,74.789072841938));
#49176=CARTESIAN_POINT('Ctrl Pts',(28.7854300007706,11.3093021925761,74.8306284308288));
#49177=CARTESIAN_POINT('Ctrl Pts',(28.7930936893998,11.2781129419873,74.9073660164418));
#49178=CARTESIAN_POINT('Ctrl Pts',(28.7985190764957,11.2543992363159,74.9426040045736));
#49179=CARTESIAN_POINT('Ctrl Pts',(28.8088155168561,11.1992993473659,74.998632839126));
#49180=CARTESIAN_POINT('Ctrl Pts',(28.8200190370477,11.1268998693587,75.0482404349203));
#49181=CARTESIAN_POINT('Ctrl Pts',(28.8268763497815,11.,75.0732472458756));
#49182=CARTESIAN_POINT('Ctrl Pts',(28.8200190370477,10.8731001306415,75.0482404349203));
#49183=CARTESIAN_POINT('Ctrl Pts',(28.8088155168561,10.8007006526339,74.9986328391256));
#49184=CARTESIAN_POINT('Ctrl Pts',(28.7985190764957,10.7456007636843,74.9426040045735));
#49185=CARTESIAN_POINT('Ctrl Pts',(28.7930936893998,10.7218870580128,74.9073660164416));
#49186=CARTESIAN_POINT('Ctrl Pts',(28.7854300007706,10.690697807424,74.8306284308285));
#49187=CARTESIAN_POINT('Ctrl Pts',(28.78330927176,10.6830240779919,74.7890728419378));
#49188=CARTESIAN_POINT('Ctrl Pts',(28.783317023756,10.6830666817342,74.7109865811408));
#49189=CARTESIAN_POINT('Ctrl Pts',(28.7854083939203,10.6907103086731,74.669419076938));
#49190=CARTESIAN_POINT('Ctrl Pts',(28.7930705898666,10.7220057364382,74.5926796862589));
#49191=CARTESIAN_POINT('Ctrl Pts',(28.7984971202626,10.7456952977549,74.5574809291687));
#49192=CARTESIAN_POINT('Ctrl Pts',(28.8088018057835,10.8010512661648,74.501349113398));
#49193=CARTESIAN_POINT('Ctrl Pts',(28.8143446526051,10.8365201881497,74.4766846891437));
#49194=CARTESIAN_POINT('Ctrl Pts',(28.8222946915156,10.9155306739479,74.4435587606527));
#49195=CARTESIAN_POINT('Ctrl Pts',(28.8245139996716,10.9590941523302,74.4352690808426));
#49196=CARTESIAN_POINT('Ctrl Pts',(28.8245239133973,11.,74.4352658835594));
#49197=CARTESIAN_POINT('Ctrl Pts',(28.8498895210029,11.,74.4676329417797));
#49198=CARTESIAN_POINT('Ctrl Pts',(28.8498994347286,11.0374731686475,74.4676297444964));
#49199=CARTESIAN_POINT('Ctrl Pts',(28.8480500789078,11.0773718356336,74.4755355640341));
#49200=CARTESIAN_POINT('Ctrl Pts',(28.8415279162029,11.1490230557141,74.5065180699672));
#49201=CARTESIAN_POINT('Ctrl Pts',(28.8370145392765,11.1807553920361,74.5294168541035));
#49202=CARTESIAN_POINT('Ctrl Pts',(28.8286875791424,11.2296820491551,74.5804873246879));
#49203=CARTESIAN_POINT('Ctrl Pts',(28.82436943821,11.2501911813549,74.6120535237142));
#49204=CARTESIAN_POINT('Ctrl Pts',(28.8182862167288,11.2770897699908,74.6798098456223));
#49205=CARTESIAN_POINT('Ctrl Pts',(28.8166559433367,11.2835149969489,74.7160141451695));
#49206=CARTESIAN_POINT('Ctrl Pts',(28.8166480659251,11.2835588407745,74.7840389985826));
#49207=CARTESIAN_POINT('Ctrl Pts',(28.8183009558858,11.2770859558961,74.8202442285893));
#49208=CARTESIAN_POINT('Ctrl Pts',(28.824374236808,11.25031714301,74.8879969147892));
#49209=CARTESIAN_POINT('Ctrl Pts',(28.8287019700868,11.229715550308,74.9195760683006));
#49210=CARTESIAN_POINT('Ctrl Pts',(28.8370133377376,11.1810854764448,74.9706146871361));
#49211=CARTESIAN_POINT('Ctrl Pts',(28.8461514336814,11.1161862398084,75.0165933605779));
#49212=CARTESIAN_POINT('Ctrl Pts',(28.85182326022,11.,75.0405083037254));
#49213=CARTESIAN_POINT('Ctrl Pts',(28.8461514336813,10.8838137601915,75.0165933605779));
#49214=CARTESIAN_POINT('Ctrl Pts',(28.8370133377375,10.8189145235551,74.970614687136));
#49215=CARTESIAN_POINT('Ctrl Pts',(28.8287019700867,10.7702844496919,74.9195760683005));
#49216=CARTESIAN_POINT('Ctrl Pts',(28.824374236808,10.7496828569899,74.8879969147891));
#49217=CARTESIAN_POINT('Ctrl Pts',(28.8183009558857,10.7229140441039,74.8202442285892));
#49218=CARTESIAN_POINT('Ctrl Pts',(28.816648065925,10.7164411592254,74.7840389985825));
#49219=CARTESIAN_POINT('Ctrl Pts',(28.8166559433366,10.716485003051,74.7160141451694));
#49220=CARTESIAN_POINT('Ctrl Pts',(28.8182862167287,10.7229102300091,74.6798098456222));
#49221=CARTESIAN_POINT('Ctrl Pts',(28.82436943821,10.749808818645,74.6120535237141));
#49222=CARTESIAN_POINT('Ctrl Pts',(28.8286875791424,10.7703179508449,74.5804873246878));
#49223=CARTESIAN_POINT('Ctrl Pts',(28.8370145392765,10.8192446079639,74.5294168541034));
#49224=CARTESIAN_POINT('Ctrl Pts',(28.8415279162029,10.8509769442859,74.5065180699671));
#49225=CARTESIAN_POINT('Ctrl Pts',(28.8480500789077,10.9226281643664,74.475535564034));
#49226=CARTESIAN_POINT('Ctrl Pts',(28.8498994347286,10.9625268313525,74.4676297444964));
#49227=CARTESIAN_POINT('Ctrl Pts',(28.8498895210029,11.,74.4676329417797));
#49228=CARTESIAN_POINT('Ctrl Pts',(28.8752551286084,11.,74.5));
#49229=CARTESIAN_POINT('Ctrl Pts',(28.8752551286084,11.0340535091136,74.5));
#49230=CARTESIAN_POINT('Ctrl Pts',(28.873799411215,11.0702901205278,74.5074880112523));
#49231=CARTESIAN_POINT('Ctrl Pts',(28.8687055816464,11.1345950272825,74.5363789429741));
#49232=CARTESIAN_POINT('Ctrl Pts',(28.8652119781344,11.1626194731303,74.5574776641716));
#49233=CARTESIAN_POINT('Ctrl Pts',(28.8588801339858,11.2050904762266,74.6035062272164));
#49234=CARTESIAN_POINT('Ctrl Pts',(28.8556469846071,11.2224793763353,74.6314463155039));
#49235=CARTESIAN_POINT('Ctrl Pts',(28.8511714251914,11.2449328797301,74.6901882808707));
#49236=CARTESIAN_POINT('Ctrl Pts',(28.8499905931822,11.2501803903799,74.7210659477303));
#49237=CARTESIAN_POINT('Ctrl Pts',(28.8499856009438,11.2502134827088,74.778986409203));
#49238=CARTESIAN_POINT('Ctrl Pts',(28.85118320127,11.2449415119774,74.80986737937));
#49239=CARTESIAN_POINT('Ctrl Pts',(28.8556545433741,11.2225906128495,74.8686010950407));
#49240=CARTESIAN_POINT('Ctrl Pts',(28.8588912678706,11.2051491197789,74.8965647447899));
#49241=CARTESIAN_POINT('Ctrl Pts',(28.8652152073783,11.1629082952113,74.9425389610847));
#49242=CARTESIAN_POINT('Ctrl Pts',(28.8722925351983,11.1056008427601,74.9850072376742));
#49243=CARTESIAN_POINT('Ctrl Pts',(28.8767941003811,11.,75.0077597316435));
#49244=CARTESIAN_POINT('Ctrl Pts',(28.8722925351983,10.8943991572398,74.9850072376742));
#49245=CARTESIAN_POINT('Ctrl Pts',(28.8652152073782,10.8370917047886,74.9425389610846));
#49246=CARTESIAN_POINT('Ctrl Pts',(28.8588912678706,10.794850880221,74.8965647447899));
#49247=CARTESIAN_POINT('Ctrl Pts',(28.8556545433741,10.7774093871504,74.8686010950406));
#49248=CARTESIAN_POINT('Ctrl Pts',(28.8511832012699,10.7550584880225,74.8098673793699));
#49249=CARTESIAN_POINT('Ctrl Pts',(28.8499856009438,10.7497865172911,74.7789864092028));
#49250=CARTESIAN_POINT('Ctrl Pts',(28.8499905931821,10.74981960962,74.7210659477302));
#49251=CARTESIAN_POINT('Ctrl Pts',(28.8511714251913,10.7550671202698,74.6901882808706));
#49252=CARTESIAN_POINT('Ctrl Pts',(28.8556469846071,10.7775206236646,74.6314463155038));
#49253=CARTESIAN_POINT('Ctrl Pts',(28.8588801339858,10.7949095237734,74.6035062272163));
#49254=CARTESIAN_POINT('Ctrl Pts',(28.8652119781344,10.8373805268697,74.5574776641715));
#49255=CARTESIAN_POINT('Ctrl Pts',(28.8687055816464,10.8654049727175,74.536378942974));
#49256=CARTESIAN_POINT('Ctrl Pts',(28.873799411215,10.9297098794722,74.5074880112522));
#49257=CARTESIAN_POINT('Ctrl Pts',(28.8752551286084,10.9659464908864,74.5));
#49258=CARTESIAN_POINT('Ctrl Pts',(28.8752551286084,11.,74.5));
#49259=CARTESIAN_POINT('',(28.7991583057917,11.,74.402898825339));
#49260=CARTESIAN_POINT('',(28.8752551286084,11.,74.5));
#49261=CARTESIAN_POINT('',(28.7991583057917,11.,74.402898825339));
#49262=CARTESIAN_POINT('',(28.8752935786535,11.,75.000175566987));
#49263=CARTESIAN_POINT('Ctrl Pts',(28.8752551286084,11.,74.5));
#49264=CARTESIAN_POINT('Ctrl Pts',(28.8752551286084,11.0340535091136,74.5));
#49265=CARTESIAN_POINT('Ctrl Pts',(28.873799411215,11.0702901205278,74.5074880112523));
#49266=CARTESIAN_POINT('Ctrl Pts',(28.8687055816464,11.1345950272825,74.5363789429741));
#49267=CARTESIAN_POINT('Ctrl Pts',(28.8652119781344,11.1626194731303,74.5574776641716));
#49268=CARTESIAN_POINT('Ctrl Pts',(28.8588801339858,11.2050904762266,74.6035062272164));
#49269=CARTESIAN_POINT('Ctrl Pts',(28.8556469846071,11.2224793763353,74.6314463155039));
#49270=CARTESIAN_POINT('Ctrl Pts',(28.8511714251914,11.2449328797301,74.6901882808707));
#49271=CARTESIAN_POINT('Ctrl Pts',(28.8499905931822,11.2501803903799,74.7210659477303));
#49272=CARTESIAN_POINT('Ctrl Pts',(28.8499856009438,11.2502134827088,74.778986409203));
#49273=CARTESIAN_POINT('Ctrl Pts',(28.85118320127,11.2449415119774,74.80986737937));
#49274=CARTESIAN_POINT('Ctrl Pts',(28.8556545433741,11.2225906128495,74.8686010950407));
#49275=CARTESIAN_POINT('Ctrl Pts',(28.8588912678706,11.2051491197789,74.8965647447899));
#49276=CARTESIAN_POINT('Ctrl Pts',(28.8652152073783,11.1629082952113,74.9425389610847));
#49277=CARTESIAN_POINT('Ctrl Pts',(28.8722925351983,11.1056008427601,74.9850072376742));
#49278=CARTESIAN_POINT('Ctrl Pts',(28.8752935786535,11.03520028092,75.000175566987));
#49279=CARTESIAN_POINT('Ctrl Pts',(28.8752935786535,11.,75.000175566987));
#49280=CARTESIAN_POINT('Ctrl Pts',(28.8752935786535,11.,75.000175566987));
#49281=CARTESIAN_POINT('Ctrl Pts',(28.8752935786535,10.9647997190799,75.000175566987));
#49282=CARTESIAN_POINT('Ctrl Pts',(28.8722925351983,10.8943991572398,74.9850072376742));
#49283=CARTESIAN_POINT('Ctrl Pts',(28.8652152073782,10.8370917047886,74.9425389610846));
#49284=CARTESIAN_POINT('Ctrl Pts',(28.8588912678706,10.794850880221,74.8965647447899));
#49285=CARTESIAN_POINT('Ctrl Pts',(28.8556545433741,10.7774093871504,74.8686010950406));
#49286=CARTESIAN_POINT('Ctrl Pts',(28.8511832012699,10.7550584880225,74.8098673793699));
#49287=CARTESIAN_POINT('Ctrl Pts',(28.8499856009438,10.7497865172911,74.7789864092028));
#49288=CARTESIAN_POINT('Ctrl Pts',(28.8499905931821,10.74981960962,74.7210659477302));
#49289=CARTESIAN_POINT('Ctrl Pts',(28.8511714251913,10.7550671202698,74.6901882808706));
#49290=CARTESIAN_POINT('Ctrl Pts',(28.8556469846071,10.7775206236646,74.6314463155038));
#49291=CARTESIAN_POINT('Ctrl Pts',(28.8588801339858,10.7949095237734,74.6035062272163));
#49292=CARTESIAN_POINT('Ctrl Pts',(28.8652119781344,10.8373805268697,74.5574776641715));
#49293=CARTESIAN_POINT('Ctrl Pts',(28.8687055816464,10.8654049727175,74.536378942974));
#49294=CARTESIAN_POINT('Ctrl Pts',(28.873799411215,10.9297098794722,74.5074880112522));
#49295=CARTESIAN_POINT('Ctrl Pts',(28.8752551286084,10.9659464908864,74.5));
#49296=CARTESIAN_POINT('Ctrl Pts',(28.8752551286084,11.,74.5));
#49297=CARTESIAN_POINT('Ctrl Pts',(28.7991583057917,11.,74.402898825339));
#49298=CARTESIAN_POINT('Ctrl Pts',(28.7991583057917,10.9556744927962,74.402898825339));
#49299=CARTESIAN_POINT('Ctrl Pts',(28.7965453592083,10.9084489588421,74.4116063134345));
#49300=CARTESIAN_POINT('Ctrl Pts',(28.7871669871616,10.8220921597181,74.4468238161368));
#49301=CARTESIAN_POINT('Ctrl Pts',(28.7806043669256,10.7829153472589,74.4732883033299));
#49302=CARTESIAN_POINT('Ctrl Pts',(28.7683045654192,10.7211037248264,74.5344620266403));
#49303=CARTESIAN_POINT('Ctrl Pts',(28.7617930434695,10.6942939314186,74.5732868944692));
#49304=CARTESIAN_POINT('Ctrl Pts',(28.7525231854577,10.6585534184123,74.6590406416897));
#49305=CARTESIAN_POINT('Ctrl Pts',(28.7499823739105,10.6497320751652,74.7059347785801));
#49306=CARTESIAN_POINT('Ctrl Pts',(28.7499717367413,10.6496787199262,74.7941254313175));
#49307=CARTESIAN_POINT('Ctrl Pts',(28.7525477553864,10.6585533635054,74.8410052800478));
#49308=CARTESIAN_POINT('Ctrl Pts',(28.7618133828337,10.6941605278523,74.9267618361901));
#49309=CARTESIAN_POINT('Ctrl Pts',(28.7683297787118,10.7210343331551,74.9656153280842));
#49310=CARTESIAN_POINT('Ctrl Pts',(28.7806136472154,10.7825234714004,75.0267085651771));
#49311=CARTESIAN_POINT('Ctrl Pts',(28.7938779355307,10.8625147335932,75.079826557824));
#49312=CARTESIAN_POINT('Ctrl Pts',(28.8019055096204,11.,75.1059958179575));
#49313=CARTESIAN_POINT('Ctrl Pts',(28.7938779355307,11.137485266407,75.079826557824));
#49314=CARTESIAN_POINT('Ctrl Pts',(28.7806136472154,11.2174765285995,75.0267085651774));
#49315=CARTESIAN_POINT('Ctrl Pts',(28.7683297787118,11.2789656668451,74.9656153280843));
#49316=CARTESIAN_POINT('Ctrl Pts',(28.7618133828337,11.3058394721478,74.9267618361903));
#49317=CARTESIAN_POINT('Ctrl Pts',(28.7525477553864,11.3414466364947,74.8410052800481));
#49318=CARTESIAN_POINT('Ctrl Pts',(28.7499717367413,11.3503212800739,74.7941254313177));
#49319=CARTESIAN_POINT('Ctrl Pts',(28.7499823739105,11.3502679248349,74.7059347785805));
#49320=CARTESIAN_POINT('Ctrl Pts',(28.7525231854577,11.3414465815878,74.65904064169));
#49321=CARTESIAN_POINT('Ctrl Pts',(28.7617930434695,11.3057060685816,74.5732868944695));
#49322=CARTESIAN_POINT('Ctrl Pts',(28.7683045654192,11.2788962751735,74.5344620266402));
#49323=CARTESIAN_POINT('Ctrl Pts',(28.7806043669257,11.2170846527409,74.4732883033298));
#49324=CARTESIAN_POINT('Ctrl Pts',(28.7871669871617,11.1779078402817,74.4468238161368));
#49325=CARTESIAN_POINT('Ctrl Pts',(28.7965453592084,11.0915510411579,74.4116063134345));
#49326=CARTESIAN_POINT('Ctrl Pts',(28.7991583057917,11.0443255072037,74.402898825339));
#49327=CARTESIAN_POINT('Ctrl Pts',(28.7991583057917,11.,74.402898825339));
#49328=CARTESIAN_POINT('Origin',(30.,11.,74.75));
#49329=CARTESIAN_POINT('',(31.1247090374087,11.0002124504859,75.0000451515836));
#49330=CARTESIAN_POINT('',(30.,11.,75.));
#49331=CARTESIAN_POINT('',(31.1247448713916,11.,74.5));
#49332=CARTESIAN_POINT('Ctrl Pts',(31.1247448713916,11.,74.5));
#49333=CARTESIAN_POINT('Ctrl Pts',(31.1247448713916,10.9659464908864,74.5));
#49334=CARTESIAN_POINT('Ctrl Pts',(31.1261756827447,10.9298345168618,74.5073000076697));
#49335=CARTESIAN_POINT('Ctrl Pts',(31.1339517690006,10.8327646136186,74.5515990517654));
#49336=CARTESIAN_POINT('Ctrl Pts',(31.1420908159051,10.7893390509663,74.6017232396597));
#49337=CARTESIAN_POINT('Ctrl Pts',(31.1476872898868,10.7609713644184,74.67535844061));
#49338=CARTESIAN_POINT('Ctrl Pts',(31.1494354031251,10.7527134717349,74.7054449809965));
#49339=CARTESIAN_POINT('Ctrl Pts',(31.1499942735367,10.7501398764272,74.7353946550602));
#49340=CARTESIAN_POINT('Ctrl Pts',(31.1500134121921,10.7500904271462,74.7788322674921));
#49341=CARTESIAN_POINT('Ctrl Pts',(31.1488155000854,10.7553567498143,74.8097236484711));
#49342=CARTESIAN_POINT('Ctrl Pts',(31.1443472815917,10.7777313954793,74.868459151291));
#49343=CARTESIAN_POINT('Ctrl Pts',(31.1411083085017,10.7951159561359,74.896430652982));
#49344=CARTESIAN_POINT('Ctrl Pts',(31.1347942340493,10.8375063649237,74.9423984737415));
#49345=CARTESIAN_POINT('Ctrl Pts',(31.127685335322,10.893977625089,74.984921689387));
#49346=CARTESIAN_POINT('Ctrl Pts',(31.1247224286309,10.9657107289254,74.9999918828307));
#49347=CARTESIAN_POINT('Ctrl Pts',(31.1247055431382,11.0002331671188,75.0000495544391));
#49348=CARTESIAN_POINT('Ctrl Pts',(31.1247055431382,11.0002331671188,75.0000495544391));
#49349=CARTESIAN_POINT('Ctrl Pts',(31.124701321765,11.0088637766672,75.0000639723411));
#49350=CARTESIAN_POINT('Ctrl Pts',(31.1250505782355,11.0430501864293,74.9982522876711));
#49351=CARTESIAN_POINT('Ctrl Pts',(31.1285913723511,11.1138410678152,74.9795740487944));
#49352=CARTESIAN_POINT('Ctrl Pts',(31.1347735960806,11.1625638434507,74.9425264014548));
#49353=CARTESIAN_POINT('Ctrl Pts',(31.1411018668555,11.2050979482099,74.8965372843256));
#49354=CARTESIAN_POINT('Ctrl Pts',(31.1443369970737,11.2224255640565,74.8685817070521));
#49355=CARTESIAN_POINT('Ctrl Pts',(31.1488131353229,11.2448334943903,74.8098480629189));
#49356=CARTESIAN_POINT('Ctrl Pts',(31.150002757725,11.2500769678483,74.7789675358608));
#49357=CARTESIAN_POINT('Ctrl Pts',(31.1500033272209,11.2500687651821,74.721048432782));
#49358=CARTESIAN_POINT('Ctrl Pts',(31.1488168576793,11.2448183482373,74.6901688043705));
#49359=CARTESIAN_POINT('Ctrl Pts',(31.1443391274454,11.2223904507778,74.6314330366943));
#49360=CARTESIAN_POINT('Ctrl Pts',(31.1411144986666,11.2050367965143,74.6034936013564));
#49361=CARTESIAN_POINT('Ctrl Pts',(31.1347817423216,11.1625707484721,74.5574686435559));
#49362=CARTESIAN_POINT('Ctrl Pts',(31.1312907402135,11.1345635586083,74.5363723884131));
#49363=CARTESIAN_POINT('Ctrl Pts',(31.1261983005099,11.0702714603723,74.5074842459491));
#49364=CARTESIAN_POINT('Ctrl Pts',(31.1247448713916,11.0340535091136,74.5));
#49365=CARTESIAN_POINT('Ctrl Pts',(31.1247448713916,11.,74.5));
#49366=CARTESIAN_POINT('Origin',(30.,0.0749999999999993,74.75));
#49367=CARTESIAN_POINT('',(30.,12.35,73.5));
#49368=CARTESIAN_POINT('Origin',(30.,12.35,74.75));
#49369=CARTESIAN_POINT('',(30.,-12.2,73.5));
#49370=CARTESIAN_POINT('',(30.,0.0749999999999993,73.5));
#49371=CARTESIAN_POINT('Origin',(30.,-12.2,74.75));
#49372=CARTESIAN_POINT('',(31.2008416942083,11.,74.402898825339));
#49373=CARTESIAN_POINT('Ctrl Pts',(31.2008416942083,11.,74.402898825339));
#49374=CARTESIAN_POINT('Ctrl Pts',(31.2008416942083,11.0443255072037,74.402898825339));
#49375=CARTESIAN_POINT('Ctrl Pts',(31.2034498953288,11.0915227449673,74.4115972952524));
#49376=CARTESIAN_POINT('Ctrl Pts',(31.2128253403987,11.177860265399,74.4468073082167));
#49377=CARTESIAN_POINT('Ctrl Pts',(31.219382667204,11.2170105083336,74.4732679137741));
#49378=CARTESIAN_POINT('Ctrl Pts',(31.2316840240808,11.2788159105534,74.5344263730226));
#49379=CARTESIAN_POINT('Ctrl Pts',(31.238178124029,11.3055670964467,74.5732631185048));
#49380=CARTESIAN_POINT('Ctrl Pts',(31.2474552469493,11.3412831677777,74.6590054383893));
#49381=CARTESIAN_POINT('Ctrl Pts',(31.2500082287207,11.3501163526545,74.7058957316331));
#49382=CARTESIAN_POINT('Ctrl Pts',(31.2500067841583,11.3501273161404,74.7940892347985));
#49383=CARTESIAN_POINT('Ctrl Pts',(31.2474485597635,11.3413050526674,74.8409763148676));
#49384=CARTESIAN_POINT('Ctrl Pts',(31.2381724030552,11.3056138390971,74.9267271045948));
#49385=CARTESIAN_POINT('Ctrl Pts',(31.2316599526739,11.2788954176252,74.9655685845438));
#49386=CARTESIAN_POINT('Ctrl Pts',(31.219366031553,11.2170074672431,75.0266815633276));
#49387=CARTESIAN_POINT('Ctrl Pts',(31.2077858172596,11.1489334478727,75.0729876097142));
#49388=CARTESIAN_POINT('Ctrl Pts',(31.2013950695966,11.0560522523136,75.0949726057065));
#49389=CARTESIAN_POINT('Ctrl Pts',(31.2001387800288,10.967068766035,75.099203566257));
#49390=CARTESIAN_POINT('Ctrl Pts',(31.2060936622365,10.8619583503284,75.0796341470907));
#49391=CARTESIAN_POINT('Ctrl Pts',(31.2193944389923,10.7831211214257,75.0265430631575));
#49392=CARTESIAN_POINT('Ctrl Pts',(31.231663625954,10.721424531713,74.9654333947178));
#49393=CARTESIAN_POINT('Ctrl Pts',(31.2381824498022,10.6946289834658,74.926572349275));
#49394=CARTESIAN_POINT('Ctrl Pts',(31.2474426701246,10.6589884763849,74.8408147269102));
#49395=CARTESIAN_POINT('Ctrl Pts',(31.2500188041202,10.6501203427759,74.7938953965327));
#49396=CARTESIAN_POINT('Ctrl Pts',(31.2499777517717,10.6502163880535,74.7277738109954));
#49397=CARTESIAN_POINT('Ctrl Pts',(31.2487735251553,10.6545117760602,74.6821698523604));
#49398=CARTESIAN_POINT('Ctrl Pts',(31.2451073934782,10.6679307949249,74.6374154183254));
#49399=CARTESIAN_POINT('Ctrl Pts',(31.2334589811991,10.7131771584539,74.5297226811336));
#49400=CARTESIAN_POINT('Ctrl Pts',(31.2176555102524,10.7784674980498,74.4652559194838));
#49401=CARTESIAN_POINT('Ctrl Pts',(31.2034310816527,10.9085549642993,74.4114322650177));
#49402=CARTESIAN_POINT('Ctrl Pts',(31.2008416942083,10.9556744927963,74.402898825339));
#49403=CARTESIAN_POINT('Ctrl Pts',(31.2008416942083,11.,74.402898825339));
#49404=CARTESIAN_POINT('Ctrl Pts',(31.2008416942083,11.,74.402898825339));
#49405=CARTESIAN_POINT('Ctrl Pts',(31.2008416942083,10.9556744927963,74.402898825339));
#49406=CARTESIAN_POINT('Ctrl Pts',(31.2034310816527,10.9085549642993,74.4114322650177));
#49407=CARTESIAN_POINT('Ctrl Pts',(31.2176555102524,10.7784674980498,74.4652559194838));
#49408=CARTESIAN_POINT('Ctrl Pts',(31.2334589811991,10.7131771584539,74.5297226811336));
#49409=CARTESIAN_POINT('Ctrl Pts',(31.2451073934782,10.6679307949249,74.6374154183254));
#49410=CARTESIAN_POINT('Ctrl Pts',(31.2487735251553,10.6545117760602,74.6821698523604));
#49411=CARTESIAN_POINT('Ctrl Pts',(31.2499777517717,10.6502163880535,74.7277738109954));
#49412=CARTESIAN_POINT('Ctrl Pts',(31.2500188041202,10.6501203427759,74.7938953965327));
#49413=CARTESIAN_POINT('Ctrl Pts',(31.2474426701246,10.6589884763849,74.8408147269102));
#49414=CARTESIAN_POINT('Ctrl Pts',(31.2381824498022,10.6946289834658,74.926572349275));
#49415=CARTESIAN_POINT('Ctrl Pts',(31.231663625954,10.721424531713,74.9654333947178));
#49416=CARTESIAN_POINT('Ctrl Pts',(31.2193944389923,10.7831211214257,75.0265430631575));
#49417=CARTESIAN_POINT('Ctrl Pts',(31.2060936622365,10.8619583503284,75.0796341470907));
#49418=CARTESIAN_POINT('Ctrl Pts',(31.2001387800288,10.967068766035,75.099203566257));
#49419=CARTESIAN_POINT('Ctrl Pts',(31.2013950695966,11.0560522523136,75.0949726057065));
#49420=CARTESIAN_POINT('Ctrl Pts',(31.2077858172596,11.1489334478727,75.0729876097142));
#49421=CARTESIAN_POINT('Ctrl Pts',(31.219366031553,11.2170074672431,75.0266815633276));
#49422=CARTESIAN_POINT('Ctrl Pts',(31.2316599526739,11.2788954176252,74.9655685845438));
#49423=CARTESIAN_POINT('Ctrl Pts',(31.2381724030552,11.3056138390971,74.9267271045948));
#49424=CARTESIAN_POINT('Ctrl Pts',(31.2474485597635,11.3413050526674,74.8409763148676));
#49425=CARTESIAN_POINT('Ctrl Pts',(31.2500067841583,11.3501273161404,74.7940892347985));
#49426=CARTESIAN_POINT('Ctrl Pts',(31.2500082287207,11.3501163526545,74.7058957316331));
#49427=CARTESIAN_POINT('Ctrl Pts',(31.2474552469493,11.3412831677777,74.6590054383893));
#49428=CARTESIAN_POINT('Ctrl Pts',(31.238178124029,11.3055670964467,74.5732631185048));
#49429=CARTESIAN_POINT('Ctrl Pts',(31.2316840240808,11.2788159105534,74.5344263730226));
#49430=CARTESIAN_POINT('Ctrl Pts',(31.219382667204,11.2170105083336,74.4732679137741));
#49431=CARTESIAN_POINT('Ctrl Pts',(31.2128253403987,11.177860265399,74.4468073082167));
#49432=CARTESIAN_POINT('Ctrl Pts',(31.2034498953288,11.0915227449673,74.4115972952524));
#49433=CARTESIAN_POINT('Ctrl Pts',(31.2008416942083,11.0443255072037,74.402898825339));
#49434=CARTESIAN_POINT('Ctrl Pts',(31.2008416942083,11.,74.402898825339));
#49435=CARTESIAN_POINT('Ctrl Pts',(31.1754760866027,11.,74.4352658835594));
#49436=CARTESIAN_POINT('Ctrl Pts',(31.1754825039498,10.9590934828951,74.4352569922628));
#49437=CARTESIAN_POINT('Ctrl Pts',(31.1776872705737,10.9156346775601,74.4434035072065));
#49438=CARTESIAN_POINT('Ctrl Pts',(31.1897460686789,10.7965923103755,74.4940126606344));
#49439=CARTESIAN_POINT('Ctrl Pts',(31.203023603427,10.7384950675313,74.5537875973164));
#49440=CARTESIAN_POINT('Ctrl Pts',(31.2126198620762,10.6990038501938,74.6500105505282));
#49441=CARTESIAN_POINT('Ctrl Pts',(31.2156609325165,10.6872473752913,74.6899269201168));
#49442=CARTESIAN_POINT('Ctrl Pts',(31.2166432344204,10.6835579773301,74.7302838024659));
#49443=CARTESIAN_POINT('Ctrl Pts',(31.2166789556008,10.6834636791878,74.7888557538772));
#49444=CARTESIAN_POINT('Ctrl Pts',(31.2145612377667,10.6911385284789,74.8304330234096));
#49445=CARTESIAN_POINT('Ctrl Pts',(31.2069013357892,10.7223471955558,74.9071783895744));
#49446=CARTESIAN_POINT('Ctrl Pts',(31.2014756711748,10.7460081723241,74.9424240072697));
#49447=CARTESIAN_POINT('Ctrl Pts',(31.1911904443518,10.8012679295396,74.9984625048355));
#49448=CARTESIAN_POINT('Ctrl Pts',(31.1799556567174,10.8726518369506,75.0480526205252));
#49449=CARTESIAN_POINT('Ctrl Pts',(31.174870941357,10.9696232075473,75.0667395509409));
#49450=CARTESIAN_POINT('Ctrl Pts',(31.1759381545625,11.0517459258799,75.0627103479815));
#49451=CARTESIAN_POINT('Ctrl Pts',(31.181383646221,11.1372451760654,75.0418355394467));
#49452=CARTESIAN_POINT('Ctrl Pts',(31.1911648504381,11.198886235768,74.9986042623894));
#49453=CARTESIAN_POINT('Ctrl Pts',(31.2014701628226,11.2542970310271,74.942558360535));
#49454=CARTESIAN_POINT('Ctrl Pts',(31.2068926720193,11.2779026324523,74.9073307299006));
#49455=CARTESIAN_POINT('Ctrl Pts',(31.2145655752016,11.3091504024221,74.8305998229589));
#49456=CARTESIAN_POINT('Ctrl Pts',(31.2166694778626,11.3167865617185,74.7890364518618));
#49457=CARTESIAN_POINT('Ctrl Pts',(31.216671810142,11.3167751295637,74.7109475137158));
#49458=CARTESIAN_POINT('Ctrl Pts',(31.2145709126828,11.3091292053491,74.6693866581129));
#49459=CARTESIAN_POINT('Ctrl Pts',(31.2069004985881,11.2778549144797,74.5926509937699));
#49460=CARTESIAN_POINT('Ctrl Pts',(31.2014913594011,11.2542241587106,74.5574480118848));
#49461=CARTESIAN_POINT('Ctrl Pts',(31.1911853119282,11.1988747330847,74.5013269976795));
#49462=CARTESIAN_POINT('Ctrl Pts',(31.1856476298239,11.163432158172,74.4766690551516));
#49463=CARTESIAN_POINT('Ctrl Pts',(31.1777005937812,11.0844410836489,74.4435491508169));
#49464=CARTESIAN_POINT('Ctrl Pts',(31.1754859791547,11.0409058106239,74.4352694871419));
#49465=CARTESIAN_POINT('Ctrl Pts',(31.1754760866027,11.,74.4352658835593));
#49466=CARTESIAN_POINT('Ctrl Pts',(31.1501104789971,11.,74.4676329417797));
#49467=CARTESIAN_POINT('Ctrl Pts',(31.15010406165,10.9625275007876,74.4676418330762));
#49468=CARTESIAN_POINT('Ctrl Pts',(31.1519194938237,10.922754803601,74.475328765481));
#49469=CARTESIAN_POINT('Ctrl Pts',(31.1618612105741,10.8146398012929,74.5228423106149));
#49470=CARTESIAN_POINT('Ctrl Pts',(31.1725261936772,10.7640211418889,74.5776583234768));
#49471=CARTESIAN_POINT('Ctrl Pts',(31.1801748212888,10.7298983091494,74.6627633084073));
#49472=CARTESIAN_POINT('Ctrl Pts',(31.1825479957639,10.7199778725037,74.6976879132401));
#49473=CARTESIAN_POINT('Ctrl Pts',(31.183328790888,10.7167982871505,74.7328846635897));
#49474=CARTESIAN_POINT('Ctrl Pts',(31.1833532607115,10.7167470907343,74.7838719101477));
#49475=CARTESIAN_POINT('Ctrl Pts',(31.1816969324434,10.7232066977203,74.8201053519717));
#49476=CARTESIAN_POINT('Ctrl Pts',(31.1756283956047,10.7500131833893,74.8878531109917));
#49477=CARTESIAN_POINT('Ctrl Pts',(31.1712962632809,10.7705323155248,74.9194400404301));
#49478=CARTESIAN_POINT('Ctrl Pts',(31.1629982286899,10.8193595568098,74.9704790320636));
#49479=CARTESIAN_POINT('Ctrl Pts',(31.1538233408412,10.8832841384667,75.0165032159526));
#49480=CARTESIAN_POINT('Ctrl Pts',(31.1496199039663,10.9721229253927,75.0343396723273));
#49481=CARTESIAN_POINT('Ctrl Pts',(31.1505074932696,11.047356512863,75.0305145453961));
#49482=CARTESIAN_POINT('Ctrl Pts',(31.1549935433897,11.1255293396224,75.010726119062));
#49483=CARTESIAN_POINT('Ctrl Pts',(31.1629747771955,11.1806850749257,74.9706037023929));
#49484=CARTESIAN_POINT('Ctrl Pts',(31.1712916567069,11.229696334808,74.9195475083345));
#49485=CARTESIAN_POINT('Ctrl Pts',(31.1756167281097,11.2501367707013,74.8879780817463));
#49486=CARTESIAN_POINT('Ctrl Pts',(31.1816961198849,11.2769881446356,74.8202245548277));
#49487=CARTESIAN_POINT('Ctrl Pts',(31.1833400640207,11.2834177222702,74.7840203187975));
#49488=CARTESIAN_POINT('Ctrl Pts',(31.1833397457996,11.2834099882729,74.7159966506994));
#49489=CARTESIAN_POINT('Ctrl Pts',(31.1817011919459,11.2769723106658,74.6797875846469));
#49490=CARTESIAN_POINT('Ctrl Pts',(31.1756167528863,11.2501026327447,74.6120451614292));
#49491=CARTESIAN_POINT('Ctrl Pts',(31.1713071633463,11.2296285483571,74.5804719624942));
#49492=CARTESIAN_POINT('Ctrl Pts',(31.1629790975973,11.1807065237209,74.5294095596505));
#49493=CARTESIAN_POINT('Ctrl Pts',(31.1584684507883,11.1489916658353,74.5065106414782));
#49494=CARTESIAN_POINT('Ctrl Pts',(31.1519476020576,11.0773531216907,74.4755323903846));
#49495=CARTESIAN_POINT('Ctrl Pts',(31.1501005864452,11.0374732056933,74.4676293381971));
#49496=CARTESIAN_POINT('Ctrl Pts',(31.1501104789971,11.,74.4676329417797));
#49497=CARTESIAN_POINT('Ctrl Pts',(31.1247448713916,11.,74.5));
#49498=CARTESIAN_POINT('Ctrl Pts',(31.1247448713916,10.9659464908864,74.5));
#49499=CARTESIAN_POINT('Ctrl Pts',(31.1261756827447,10.9298345168618,74.5073000076697));
#49500=CARTESIAN_POINT('Ctrl Pts',(31.1339517690006,10.8327646136186,74.5515990517654));
#49501=CARTESIAN_POINT('Ctrl Pts',(31.1420908159051,10.7893390509663,74.6017232396597));
#49502=CARTESIAN_POINT('Ctrl Pts',(31.1476872898868,10.7609713644184,74.67535844061));
#49503=CARTESIAN_POINT('Ctrl Pts',(31.1494354031251,10.7527134717349,74.7054449809965));
#49504=CARTESIAN_POINT('Ctrl Pts',(31.1499942735367,10.7501398764272,74.7353946550602));
#49505=CARTESIAN_POINT('Ctrl Pts',(31.1500134121921,10.7500904271462,74.7788322674921));
#49506=CARTESIAN_POINT('Ctrl Pts',(31.1488155000854,10.7553567498143,74.8097236484711));
#49507=CARTESIAN_POINT('Ctrl Pts',(31.1443472815917,10.7777313954793,74.868459151291));
#49508=CARTESIAN_POINT('Ctrl Pts',(31.1411083085017,10.7951159561359,74.896430652982));
#49509=CARTESIAN_POINT('Ctrl Pts',(31.1347942340493,10.8375063649237,74.9423984737415));
#49510=CARTESIAN_POINT('Ctrl Pts',(31.127685335322,10.893977625089,74.984921689387));
#49511=CARTESIAN_POINT('Ctrl Pts',(31.1243520652945,10.974677366905,75.0018756570112));
#49512=CARTESIAN_POINT('Ctrl Pts',(31.1250505782355,11.0430501864293,74.9982522876711));
#49513=CARTESIAN_POINT('Ctrl Pts',(31.1285913723511,11.1138410678152,74.9795740487944));
#49514=CARTESIAN_POINT('Ctrl Pts',(31.1347735960806,11.1625638434507,74.9425264014548));
#49515=CARTESIAN_POINT('Ctrl Pts',(31.1411018668555,11.2050979482099,74.8965372843256));
#49516=CARTESIAN_POINT('Ctrl Pts',(31.1443369970737,11.2224255640565,74.8685817070521));
#49517=CARTESIAN_POINT('Ctrl Pts',(31.1488131353229,11.2448334943903,74.8098480629189));
#49518=CARTESIAN_POINT('Ctrl Pts',(31.150002757725,11.2500769678483,74.7789675358608));
#49519=CARTESIAN_POINT('Ctrl Pts',(31.1500033272209,11.2500687651821,74.721048432782));
#49520=CARTESIAN_POINT('Ctrl Pts',(31.1488168576793,11.2448183482373,74.6901688043705));
#49521=CARTESIAN_POINT('Ctrl Pts',(31.1443391274454,11.2223904507778,74.6314330366943));
#49522=CARTESIAN_POINT('Ctrl Pts',(31.1411144986666,11.2050367965143,74.6034936013564));
#49523=CARTESIAN_POINT('Ctrl Pts',(31.1347817423216,11.1625707484721,74.5574686435559));
#49524=CARTESIAN_POINT('Ctrl Pts',(31.1312907402135,11.1345635586083,74.5363723884131));
#49525=CARTESIAN_POINT('Ctrl Pts',(31.1261983005099,11.0702714603723,74.5074842459491));
#49526=CARTESIAN_POINT('Ctrl Pts',(31.1247448713916,11.0340535091136,74.5));
#49527=CARTESIAN_POINT('Ctrl Pts',(31.1247448713916,11.,74.5));
#49528=CARTESIAN_POINT('',(31.2008416942083,11.,74.402898825339));
#49529=CARTESIAN_POINT('Origin',(30.,-13.6,72.55));
#49530=CARTESIAN_POINT('',(30.,-13.6,71.05));
#49531=CARTESIAN_POINT('Origin',(30.,-13.6,70.75));
#49532=CARTESIAN_POINT('Origin',(30.,-13.6,72.55));
#49533=CARTESIAN_POINT('',(29.5980419823739,-13.9,74.3045454545454));
#49534=CARTESIAN_POINT('',(30.,-13.82360679775,74.15));
#49535=CARTESIAN_POINT('Ctrl Pts',(29.5980419823739,-13.9,74.3045454545454));
#49536=CARTESIAN_POINT('Ctrl Pts',(29.6299329572115,-13.9,74.2757684824466));
#49537=CARTESIAN_POINT('Ctrl Pts',(29.6652052380112,-13.8937937433722,74.2501593480394));
#49538=CARTESIAN_POINT('Ctrl Pts',(29.7577242969844,-13.8709763234875,74.1975402590115));
#49539=CARTESIAN_POINT('Ctrl Pts',(29.8164159855257,-13.8512468382518,74.1753780693518));
#49540=CARTESIAN_POINT('Ctrl Pts',(29.9235631410305,-13.8279036783418,74.1530313303057));
#49541=CARTESIAN_POINT('Ctrl Pts',(29.9641370497313,-13.82360679775,74.15));
#49542=CARTESIAN_POINT('Ctrl Pts',(30.,-13.82360679775,74.15));
#49543=CARTESIAN_POINT('',(30.,-13.37639320225,74.15));
#49544=CARTESIAN_POINT('Ctrl Pts',(30.,-13.37639320225,74.15));
#49545=CARTESIAN_POINT('Ctrl Pts',(29.9794953753375,-13.37639320225,74.15));
#49546=CARTESIAN_POINT('Ctrl Pts',(29.9592909928131,-13.3750898546546,74.1510401268365));
#49547=CARTESIAN_POINT('Ctrl Pts',(29.8830224888261,-13.3659078861817,74.1588159892685));
#49548=CARTESIAN_POINT('Ctrl Pts',(29.8286898089983,-13.3504584038552,74.1723413828209));
#49549=CARTESIAN_POINT('Ctrl Pts',(29.7200329870219,-13.319457616754,74.2157256444075));
#49550=CARTESIAN_POINT('Ctrl Pts',(29.6643996251244,-13.3033848210483,74.2482102326836));
#49551=CARTESIAN_POINT('Ctrl Pts',(29.5791479058784,-13.298480523946,74.3199941647947));
#49552=CARTESIAN_POINT('Ctrl Pts',(29.5505013820635,-13.3029058495517,74.3506920895563));
#49553=CARTESIAN_POINT('Ctrl Pts',(29.5050267351839,-13.3246102878397,74.409048352129));
#49554=CARTESIAN_POINT('Ctrl Pts',(29.4870006484232,-13.3408915120094,74.4373454937145));
#49555=CARTESIAN_POINT('Ctrl Pts',(29.4588733912034,-13.3860723864243,74.4892250785234));
#49556=CARTESIAN_POINT('Ctrl Pts',(29.448875238238,-13.4134749329035,74.5120117456315));
#49557=CARTESIAN_POINT('Ctrl Pts',(29.4346676303895,-13.4777648036933,74.5480752194044));
#49558=CARTESIAN_POINT('Ctrl Pts',(29.4305259541235,-13.5139266743675,74.5609560195142));
#49559=CARTESIAN_POINT('Ctrl Pts',(29.4267888944086,-13.5902829562109,74.572614364528));
#49560=CARTESIAN_POINT('Ctrl Pts',(29.4270773491324,-13.6296654597012,74.5715559886456));
#49561=CARTESIAN_POINT('Ctrl Pts',(29.4326305328973,-13.7056202535665,74.554633868808));
#49562=CARTESIAN_POINT('Ctrl Pts',(29.4376557542476,-13.7415461681365,74.5395144153543));
#49563=CARTESIAN_POINT('Ctrl Pts',(29.4548984871125,-13.8038410670045,74.4983529291516));
#49564=CARTESIAN_POINT('Ctrl Pts',(29.466452665742,-13.8300026504726,74.4736261267548));
#49565=CARTESIAN_POINT('Ctrl Pts',(29.4978314302509,-13.8692698084774,74.4203192067732));
#49566=CARTESIAN_POINT('Ctrl Pts',(29.5162338339307,-13.8827010732779,74.3933136319637));
#49567=CARTESIAN_POINT('Ctrl Pts',(29.5568556753082,-13.8972216746017,74.3445242219706));
#49568=CARTESIAN_POINT('Ctrl Pts',(29.5766365525769,-13.9,74.3238607454443));
#49569=CARTESIAN_POINT('Ctrl Pts',(29.5980419823739,-13.9,74.3045454545454));
#49570=CARTESIAN_POINT('Ctrl Pts',(30.,-13.82360679775,74.15));
#49571=CARTESIAN_POINT('Ctrl Pts',(30.0139201627258,-13.82360679775,74.15));
#49572=CARTESIAN_POINT('Ctrl Pts',(30.0271307004912,-13.8242030380086,74.150481853825));
#49573=CARTESIAN_POINT('Ctrl Pts',(30.0951134270113,-13.8296487208663,74.1549872164826));
#49574=CARTESIAN_POINT('Ctrl Pts',(30.1470884450656,-13.8429898222123,74.1662249454546));
#49575=CARTESIAN_POINT('Ctrl Pts',(30.2564245659286,-13.8734934982371,74.2035250184848));
#49576=CARTESIAN_POINT('Ctrl Pts',(30.3181043027727,-13.8932621546788,74.236141432118));
#49577=CARTESIAN_POINT('Ctrl Pts',(30.4105948909293,-13.9020508296339,74.3100801712879));
#49578=CARTESIAN_POINT('Ctrl Pts',(30.4406865741523,-13.8991034314819,74.3408667023364));
#49579=CARTESIAN_POINT('Ctrl Pts',(30.4884374841349,-13.879935290849,74.3996958219046));
#49580=CARTESIAN_POINT('Ctrl Pts',(30.507427201871,-13.8649842245123,74.428279748768));
#49581=CARTESIAN_POINT('Ctrl Pts',(30.5373103969786,-13.8221497329062,74.4813585396897));
#49582=CARTESIAN_POINT('Ctrl Pts',(30.5480743028103,-13.7958333738599,74.5049645380456));
#49583=CARTESIAN_POINT('Ctrl Pts',(30.5635948407606,-13.7333355759204,74.5431596663098));
#49584=CARTESIAN_POINT('Ctrl Pts',(30.5682799532287,-13.6979191328649,74.5573393219793));
#49585=CARTESIAN_POINT('Ctrl Pts',(30.5730288490156,-13.6223329980383,74.5719664120908));
#49586=CARTESIAN_POINT('Ctrl Pts',(30.573190284946,-13.5829576742045,74.5724938084201));
#49587=CARTESIAN_POINT('Ctrl Pts',(30.5686945991741,-13.5063041854332,74.5585902148283));
#49588=CARTESIAN_POINT('Ctrl Pts',(30.5642619605433,-13.4697037615921,74.5448600382466));
#49589=CARTESIAN_POINT('Ctrl Pts',(30.5484494876966,-13.4053569359173,74.5058346202232));
#49590=CARTESIAN_POINT('Ctrl Pts',(30.5376532005426,-13.3778853487224,74.4817796353062));
#49591=CARTESIAN_POINT('Ctrl Pts',(30.5077927921875,-13.335976596918,74.4291088579952));
#49592=CARTESIAN_POINT('Ctrl Pts',(30.4901145600946,-13.3212359418054,74.4021046660281));
#49593=CARTESIAN_POINT('Ctrl Pts',(30.4463232765293,-13.3027154144527,74.3475057927709));
#49594=CARTESIAN_POINT('Ctrl Pts',(30.421280112191,-13.2991731666418,74.3211276524706));
#49595=CARTESIAN_POINT('Ctrl Pts',(30.3594460746035,-13.301324643572,74.2675478584065));
#49596=CARTESIAN_POINT('Ctrl Pts',(30.3225431038836,-13.308777580929,74.2420598906178));
#49597=CARTESIAN_POINT('Ctrl Pts',(30.2254396406629,-13.334067198621,74.1901817946429));
#49598=CARTESIAN_POINT('Ctrl Pts',(30.163336812327,-13.3549930609079,74.1688930877428));
#49599=CARTESIAN_POINT('Ctrl Pts',(30.0641239823376,-13.3732076629203,74.1524392990832));
#49600=CARTESIAN_POINT('Ctrl Pts',(30.0317030754474,-13.37639320225,74.15));
#49601=CARTESIAN_POINT('Ctrl Pts',(30.,-13.37639320225,74.15));
#49602=CARTESIAN_POINT('Origin',(30.,-13.525,74.75));
#49603=CARTESIAN_POINT('',(30.,-13.,74.15));
#49604=CARTESIAN_POINT('Origin',(30.,-13.,74.75));
#49605=CARTESIAN_POINT('',(30.,-13.525,74.15));
#49606=CARTESIAN_POINT('',(30.,-14.1,74.15));
#49607=CARTESIAN_POINT('',(30.,-13.525,74.15));
#49608=CARTESIAN_POINT('Origin',(30.,-14.1,74.75));
#49609=CARTESIAN_POINT('Origin',(30.,-14.2,75.25));
#49610=CARTESIAN_POINT('',(30.,-14.2,74.25));
#49611=CARTESIAN_POINT('Origin',(30.,-14.2,74.75));
#49612=CARTESIAN_POINT('Origin',(30.,-14.15,74.75));
#49613=CARTESIAN_POINT('',(30.,-14.15,74.2));
#49614=CARTESIAN_POINT('Origin',(30.,-13.,76.35));
#49615=CARTESIAN_POINT('',(30.,-13.,73.15));
#49616=CARTESIAN_POINT('Origin',(30.,-13.,74.75));
#49617=CARTESIAN_POINT('Origin',(30.,-12.95,74.75));
#49618=CARTESIAN_POINT('',(30.,-12.9,73.05));
#49619=CARTESIAN_POINT('Origin',(30.,-12.9,74.75));
#49620=CARTESIAN_POINT('',(30.,-12.95,73.1));
#49621=CARTESIAN_POINT('Origin',(30.,-12.6,74.75));
#49622=CARTESIAN_POINT('',(30.,-12.3,73.05));
#49623=CARTESIAN_POINT('Origin',(30.,-12.3,74.75));
#49624=CARTESIAN_POINT('',(30.,-12.6,73.05));
#49625=CARTESIAN_POINT('Origin',(30.,-12.25,74.75));
#49626=CARTESIAN_POINT('',(30.,-12.2,73.15));
#49627=CARTESIAN_POINT('Origin',(30.,-12.2,74.75));
#49628=CARTESIAN_POINT('',(30.,-12.25,73.1));
#49629=CARTESIAN_POINT('Origin',(30.,-12.2,76.));
#49630=CARTESIAN_POINT('Origin',(30.,12.425,74.75));
#49631=CARTESIAN_POINT('',(30.,12.5,73.65));
#49632=CARTESIAN_POINT('Origin',(30.,12.5,74.75));
#49633=CARTESIAN_POINT('',(30.,12.425,73.575));
#49634=CARTESIAN_POINT('Origin',(30.,12.5,74.75));
#49635=CARTESIAN_POINT('',(0.,0.,0.));
#49636=CARTESIAN_POINT('Ctrl Pts',(32.6,10.85,74.75));
#49637=CARTESIAN_POINT('Ctrl Pts',(32.2762401972932,10.85,74.7508128231767));
#49638=CARTESIAN_POINT('Ctrl Pts',(31.6096093142576,10.85,74.7508592792408));
#49639=CARTESIAN_POINT('Ctrl Pts',(30.6649845099545,10.85,74.7480354284176));
#49640=CARTESIAN_POINT('Ctrl Pts',(29.7873935141465,10.85,74.7508112397276));
#49641=CARTESIAN_POINT('Ctrl Pts',(29.0359543531313,10.85,74.7503280524995));
#49642=CARTESIAN_POINT('Ctrl Pts',(28.4690072452371,10.85,74.7453827659742));
#49643=CARTESIAN_POINT('Ctrl Pts',(28.0559136155584,10.85,74.7762871198526));
#49644=CARTESIAN_POINT('Ctrl Pts',(27.7603250073182,10.85,74.8351351843659));
#49645=CARTESIAN_POINT('Ctrl Pts',(27.4815926484957,10.85,74.9426482833623));
#49646=CARTESIAN_POINT('Ctrl Pts',(27.2349066090381,10.85,75.1047310768146));
#49647=CARTESIAN_POINT('Ctrl Pts',(27.0488833547682,10.85,75.316337989367));
#49648=CARTESIAN_POINT('Ctrl Pts',(26.9333942799495,10.85,75.6052491869369));
#49649=CARTESIAN_POINT('Ctrl Pts',(26.9691269620806,10.85,75.9631669379198));
#49650=CARTESIAN_POINT('Ctrl Pts',(27.2040779638452,10.85,76.3230245921545));
#49651=CARTESIAN_POINT('Ctrl Pts',(27.5697532039707,10.85,76.564507863235));
#49652=CARTESIAN_POINT('Ctrl Pts',(28.0086353410587,10.85,76.644046754502));
#49653=CARTESIAN_POINT('Ctrl Pts',(28.4740751575422,10.85,76.5836894126618));
#49654=CARTESIAN_POINT('Ctrl Pts',(28.9373359185006,10.85,76.4628665594052));
#49655=CARTESIAN_POINT('Ctrl Pts',(29.391243866756,10.85,76.3646478753146));
#49656=CARTESIAN_POINT('Ctrl Pts',(29.9224229501769,10.85,76.3317150468999));
#49657=CARTESIAN_POINT('Ctrl Pts',(30.3862078321633,10.85,76.4084139727046));
#49658=CARTESIAN_POINT('Ctrl Pts',(30.8370751782289,10.85,76.5088290665611));
#49659=CARTESIAN_POINT('Ctrl Pts',(31.2017423456432,10.85,76.5874722844094));
#49660=CARTESIAN_POINT('Ctrl Pts',(31.6306430333322,10.85,76.6203631077507));
#49661=CARTESIAN_POINT('Ctrl Pts',(32.057764032766,10.85,76.5556313773306));
#49662=CARTESIAN_POINT('Ctrl Pts',(32.4547567135938,10.85,76.3953576871574));
#49663=CARTESIAN_POINT('Ctrl Pts',(32.7799571046759,10.85,76.160246076731));
#49664=CARTESIAN_POINT('Ctrl Pts',(32.936764346482,10.85,75.9604837805911));
#49665=CARTESIAN_POINT('Ctrl Pts',(33.,10.85,75.85));
#49666=CARTESIAN_POINT('Ctrl Pts',(32.6000563369875,10.85,74.7724398768066));
#49667=CARTESIAN_POINT('Ctrl Pts',(32.276260929417,10.85,74.773252789372));
#49668=CARTESIAN_POINT('Ctrl Pts',(31.6095450892366,10.85,74.7733264598551));
#49669=CARTESIAN_POINT('Ctrl Pts',(30.6649680305084,10.85,74.770524214627));
#49670=CARTESIAN_POINT('Ctrl Pts',(29.7874988197858,10.85,74.7733201933816));
#49671=CARTESIAN_POINT('Ctrl Pts',(29.0357590293253,10.85,74.772827717134));
#49672=CARTESIAN_POINT('Ctrl Pts',(28.4691172918998,10.85,74.7679357482136));
#49673=CARTESIAN_POINT('Ctrl Pts',(28.0587241075366,10.85,74.7986993033607));
#49674=CARTESIAN_POINT('Ctrl Pts',(27.7664700618278,10.85,74.8569322976131));
#49675=CARTESIAN_POINT('Ctrl Pts',(27.4918367913922,10.85,74.9629249524921));
#49676=CARTESIAN_POINT('Ctrl Pts',(27.2496218968497,10.85,75.1221404024895));
#49677=CARTESIAN_POINT('Ctrl Pts',(27.0682838610513,10.85,75.3287569874176));
#49678=CARTESIAN_POINT('Ctrl Pts',(26.9567767966594,10.85,75.6081224286654));
#49679=CARTESIAN_POINT('Ctrl Pts',(26.990989309624,10.85,75.9546108087208));
#49680=CARTESIAN_POINT('Ctrl Pts',(27.2204142671727,10.85,76.3066636425127));
#49681=CARTESIAN_POINT('Ctrl Pts',(27.5782958003512,10.85,76.542870690622));
#49682=CARTESIAN_POINT('Ctrl Pts',(28.008423773198,10.85,76.6211208212145));
#49683=CARTESIAN_POINT('Ctrl Pts',(28.4690883466175,10.85,76.5616816518995));
#49684=CARTESIAN_POINT('Ctrl Pts',(28.9315833093654,10.85,76.4410887479559));
#49685=CARTESIAN_POINT('Ctrl Pts',(29.3878485867094,10.85,76.3422677074518));
#49686=CARTESIAN_POINT('Ctrl Pts',(29.9240098885591,10.85,76.3090400645788));
#49687=CARTESIAN_POINT('Ctrl Pts',(30.3908025345374,10.85,76.3863518680965));
#49688=CARTESIAN_POINT('Ctrl Pts',(30.8421588378765,10.85,76.4868839589043));
#49689=CARTESIAN_POINT('Ctrl Pts',(31.2056042124841,10.85,76.5652084041602));
#49690=CARTESIAN_POINT('Ctrl Pts',(31.6300186898376,10.85,76.597644224807));
#49691=CARTESIAN_POINT('Ctrl Pts',(32.0517912777471,10.85,76.5337352307175));
#49692=CARTESIAN_POINT('Ctrl Pts',(32.4440368335229,10.85,76.3753717458181));
#49693=CARTESIAN_POINT('Ctrl Pts',(32.7643760861828,10.85,76.1436502815021));
#49694=CARTESIAN_POINT('Ctrl Pts',(32.9183725363797,10.85,75.9474433601901));
#49695=CARTESIAN_POINT('Ctrl Pts',(32.980524424349,10.85,75.8388531081455));
#49696=CARTESIAN_POINT('Ctrl Pts',(32.6001686447022,10.8603147982162,74.8171737433964));
#49697=CARTESIAN_POINT('Ctrl Pts',(32.2763031787803,10.8603147982162,74.8179868318485));
#49698=CARTESIAN_POINT('Ctrl Pts',(31.6094377488407,10.8603147982161,74.8180197771703));
#49699=CARTESIAN_POINT('Ctrl Pts',(30.6649729046424,10.8603147982162,74.8151630306089));
#49700=CARTESIAN_POINT('Ctrl Pts',(29.7877524648402,10.8603147982162,74.8179500966226));
#49701=CARTESIAN_POINT('Ctrl Pts',(29.0354254148949,10.8603147982162,74.8174167247621));
#49702=CARTESIAN_POINT('Ctrl Pts',(28.4693985677817,10.8603147982162,74.8125554634436));
#49703=CARTESIAN_POINT('Ctrl Pts',(28.0643229618056,10.8603147982162,74.8430210576306));
#49704=CARTESIAN_POINT('Ctrl Pts',(27.7786338309861,10.8603147982162,74.9000202289801));
#49705=CARTESIAN_POINT('Ctrl Pts',(27.5120694364702,10.8603147982162,75.0030004765062));
#49706=CARTESIAN_POINT('Ctrl Pts',(27.2786525998037,10.8603147982162,75.1565559636045));
#49707=CARTESIAN_POINT('Ctrl Pts',(27.106533890621,10.8603147982162,75.3533339117745));
#49708=CARTESIAN_POINT('Ctrl Pts',(27.0028575113137,10.8603147982162,75.6138882653673));
#49709=CARTESIAN_POINT('Ctrl Pts',(27.0340645306277,10.8603147982162,75.9378170546844));
#49710=CARTESIAN_POINT('Ctrl Pts',(27.2526034559054,10.8603147982162,76.274488465086));
#49711=CARTESIAN_POINT('Ctrl Pts',(27.5951158125273,10.8603147982162,76.5002428856615));
#49712=CARTESIAN_POINT('Ctrl Pts',(28.0079879414614,10.8603147982162,76.5759141203375));
#49713=CARTESIAN_POINT('Ctrl Pts',(28.4592263548061,10.8603147982162,76.5182386328934));
#49714=CARTESIAN_POINT('Ctrl Pts',(28.9201772975586,10.8603147982162,76.3980556836469));
#49715=CARTESIAN_POINT('Ctrl Pts',(29.3810653556096,10.8603147982161,76.2980313748935));
#49716=CARTESIAN_POINT('Ctrl Pts',(29.9269962160277,10.8603147982162,76.2641971595999));
#49717=CARTESIAN_POINT('Ctrl Pts',(30.3996417432911,10.8603147982161,76.3426700071549));
#49718=CARTESIAN_POINT('Ctrl Pts',(30.8519578972724,10.8603147982161,76.443435682308));
#49719=CARTESIAN_POINT('Ctrl Pts',(31.2129494545749,10.8603147982161,76.5211163903991));
#49720=CARTESIAN_POINT('Ctrl Pts',(31.6284955249479,10.8603147982162,76.5526529958711));
#49721=CARTESIAN_POINT('Ctrl Pts',(32.0396921756707,10.8603147982161,76.4903571871348));
#49722=CARTESIAN_POINT('Ctrl Pts',(32.4225403421799,10.8603147982161,76.3357529267033));
#49723=CARTESIAN_POINT('Ctrl Pts',(32.7332695950143,10.8603147982162,76.1107032847168));
#49724=CARTESIAN_POINT('Ctrl Pts',(32.8816804851804,10.8603147982162,75.9214962201899));
#49725=CARTESIAN_POINT('Ctrl Pts',(32.9416998884375,10.8603147982162,75.816631793055));
#49726=CARTESIAN_POINT('Ctrl Pts',(32.6003507870374,10.9173779978439,74.8897237988075));
#49727=CARTESIAN_POINT('Ctrl Pts',(32.2763706833012,10.9173779978439,74.8905371750664));
#49728=CARTESIAN_POINT('Ctrl Pts',(31.6092408059009,10.9173779978439,74.8906089842051));
#49729=CARTESIAN_POINT('Ctrl Pts',(30.6649391372427,10.9173779978439,74.8877716255048));
#49730=CARTESIAN_POINT('Ctrl Pts',(29.7881155384771,10.9173779978439,74.8905984912303));
#49731=CARTESIAN_POINT('Ctrl Pts',(29.0348227573495,10.9173779978439,74.8900235131441));
#49732=CARTESIAN_POINT('Ctrl Pts',(28.4697863721622,10.9173779978439,74.8852955412753));
#49733=CARTESIAN_POINT('Ctrl Pts',(28.073407529173,10.9173779978439,74.9152969842928));
#49734=CARTESIAN_POINT('Ctrl Pts',(27.7984566406093,10.9173779978439,74.9703036077729));
#49735=CARTESIAN_POINT('Ctrl Pts',(27.5450918599662,10.9173779978439,75.0683777464734));
#49736=CARTESIAN_POINT('Ctrl Pts',(27.3260710565629,10.9173779978439,75.2126918714373));
#49737=CARTESIAN_POINT('Ctrl Pts',(27.1690376611787,10.9173779978439,75.3933923333458));
#49738=CARTESIAN_POINT('Ctrl Pts',(27.0781798920543,10.9173779978439,75.6231973743156));
#49739=CARTESIAN_POINT('Ctrl Pts',(27.1044849838054,10.9173779978439,75.9102903143264));
#49740=CARTESIAN_POINT('Ctrl Pts',(27.3052250360147,10.9173779978439,76.2218198596427));
#49741=CARTESIAN_POINT('Ctrl Pts',(27.622626334009,10.9173779978439,76.4305496821952));
#49742=CARTESIAN_POINT('Ctrl Pts',(28.0072966464833,10.9173779978439,76.5020491981849));
#49743=CARTESIAN_POINT('Ctrl Pts',(28.4431445330614,10.9173779978439,76.4473077471168));
#49744=CARTESIAN_POINT('Ctrl Pts',(28.9016105836741,10.9173779978439,76.3278431856978));
#49745=CARTESIAN_POINT('Ctrl Pts',(29.3700804966718,10.9173779978439,76.2258701284851));
#49746=CARTESIAN_POINT('Ctrl Pts',(29.9320352589329,10.9173779978439,76.1910729980464));
#49747=CARTESIAN_POINT('Ctrl Pts',(30.4143311380162,10.9173779978439,76.2714959237099));
#49748=CARTESIAN_POINT('Ctrl Pts',(30.8682204343415,10.9173779978439,76.3726400416632));
#49749=CARTESIAN_POINT('Ctrl Pts',(31.2252524300623,10.9173779978439,76.449285856095));
#49750=CARTESIAN_POINT('Ctrl Pts',(31.6263329075708,10.9173779978439,76.4793554494757));
#49751=CARTESIAN_POINT('Ctrl Pts',(32.0202822219457,10.9173779978439,76.4197056854291));
#49752=CARTESIAN_POINT('Ctrl Pts',(32.3878166590065,10.9173779978439,76.2712520604576));
#49753=CARTESIAN_POINT('Ctrl Pts',(32.6828711573204,10.9173779978439,76.0571183509728));
#49754=CARTESIAN_POINT('Ctrl Pts',(32.8222036961853,10.9173779978439,75.8793607200281));
#49755=CARTESIAN_POINT('Ctrl Pts',(32.8787336741032,10.9173779978439,75.7805929311363));
#49756=CARTESIAN_POINT('Ctrl Pts',(32.6004197403532,11.0382323039103,74.9171889506208));
#49757=CARTESIAN_POINT('Ctrl Pts',(32.2763960824041,11.0382323039103,74.9180024362257));
#49758=CARTESIAN_POINT('Ctrl Pts',(31.6091627411914,11.0382323039103,74.91810506137));
#49759=CARTESIAN_POINT('Ctrl Pts',(30.6649199575373,11.0382323039103,74.9152915856771));
#49760=CARTESIAN_POINT('Ctrl Pts',(29.7882455741809,11.0382323039103,74.918141846035));
#49761=CARTESIAN_POINT('Ctrl Pts',(29.0345851556084,11.0382323039103,74.9175549113419));
#49762=CARTESIAN_POINT('Ctrl Pts',(28.4699226877837,11.0382323039103,74.9128902134163));
#49763=CARTESIAN_POINT('Ctrl Pts',(28.0768473126076,11.0382323039103,74.9427188731477));
#49764=CARTESIAN_POINT('Ctrl Pts',(27.8059755754844,11.0382323039104,74.9969724834831));
#49765=CARTESIAN_POINT('Ctrl Pts',(27.5576251549794,11.0382323039104,75.0931861718835));
#49766=CARTESIAN_POINT('Ctrl Pts',(27.3440737596402,11.0382323039103,75.2339923011634));
#49767=CARTESIAN_POINT('Ctrl Pts',(27.1927716423468,11.0382323039103,75.4085877577714));
#49768=CARTESIAN_POINT('Ctrl Pts',(27.1067848106127,11.0382323039103,75.6267150594627));
#49769=CARTESIAN_POINT('Ctrl Pts',(27.1312299556696,11.0382323039103,75.899824991557));
#49770=CARTESIAN_POINT('Ctrl Pts',(27.3252098550035,11.0382323039103,76.2018065323155));
#49771=CARTESIAN_POINT('Ctrl Pts',(27.6330764906777,11.0382323039103,76.4040802732469));
#49772=CARTESIAN_POINT('Ctrl Pts',(28.0070373299347,11.0382323039103,76.4740021623901));
#49773=CARTESIAN_POINT('Ctrl Pts',(28.4370430349808,11.0382323039103,76.4203827524898));
#49774=CARTESIAN_POINT('Ctrl Pts',(28.8945713347287,11.0382323039104,76.3011983644768));
#49775=CARTESIAN_POINT('Ctrl Pts',(29.3659244771377,11.0382323039103,76.198487991896));
#49776=CARTESIAN_POINT('Ctrl Pts',(29.933972930673,11.0382323039104,76.1633295300463));
#49777=CARTESIAN_POINT('Ctrl Pts',(30.4199463885132,11.0382323039103,76.2445009897536));
#49778=CARTESIAN_POINT('Ctrl Pts',(30.8744337504458,11.0382323039103,76.3457883146342));
#49779=CARTESIAN_POINT('Ctrl Pts',(31.2299698631872,11.0382323039103,76.4220437523547));
#49780=CARTESIAN_POINT('Ctrl Pts',(31.6255614351983,11.0382323039103,76.4515566535074));
#49781=CARTESIAN_POINT('Ctrl Pts',(32.0129668538595,11.0382323039103,76.3929131655577));
#49782=CARTESIAN_POINT('Ctrl Pts',(32.3746928081619,11.0382323039103,76.2467962447793));
#49783=CARTESIAN_POINT('Ctrl Pts',(32.663799662923,11.0382323039103,76.0368096155983));
#49784=CARTESIAN_POINT('Ctrl Pts',(32.7996924162414,11.0382323039103,75.8634012602469));
#49785=CARTESIAN_POINT('Ctrl Pts',(32.8548966608026,11.0382323039103,75.7669497601123));
#49786=CARTESIAN_POINT('Ctrl Pts',(32.6001868385096,11.1547886743356,74.8244206129357));
#49787=CARTESIAN_POINT('Ctrl Pts',(32.2763096092205,11.1547886743356,74.8252337309206));
#49788=CARTESIAN_POINT('Ctrl Pts',(31.6094110486143,11.1547886743356,74.8253028169753));
#49789=CARTESIAN_POINT('Ctrl Pts',(30.6649567181913,11.1547886743356,74.8224811471162));
#49790=CARTESIAN_POINT('Ctrl Pts',(29.7877738826518,11.1547886743356,74.825288870932));
#49791=CARTESIAN_POINT('Ctrl Pts',(29.0353462768564,11.1547886743356,74.8247589437306));
#49792=CARTESIAN_POINT('Ctrl Pts',(28.4694162812406,11.1547886743356,74.8199366672874));
#49793=CARTESIAN_POINT('Ctrl Pts',(28.0652317101301,11.1547886743356,74.8503617671289));
#49794=CARTESIAN_POINT('Ctrl Pts',(27.7806432308789,11.1547886743356,74.9071645160077));
#49795=CARTESIAN_POINT('Ctrl Pts',(27.5154321828776,11.1547886743356,75.0096483867191));
#49796=CARTESIAN_POINT('Ctrl Pts',(27.2834924502539,11.1547886743356,75.1622617256134));
#49797=CARTESIAN_POINT('Ctrl Pts',(27.1129215593886,11.1547886743356,75.3573965112237));
#49798=CARTESIAN_POINT('Ctrl Pts',(27.0105620979254,11.1547886743356,75.614805214542));
#49799=CARTESIAN_POINT('Ctrl Pts',(27.0412709960272,11.1547886743356,75.9349781814651));
#49800=CARTESIAN_POINT('Ctrl Pts',(27.2579878317068,11.1547886743356,76.269077945434));
#49801=CARTESIAN_POINT('Ctrl Pts',(27.5979349842812,11.1547886743356,76.493109562925));
#49802=CARTESIAN_POINT('Ctrl Pts',(28.0079236688243,11.1547886743356,76.5683674061805));
#49803=CARTESIAN_POINT('Ctrl Pts',(28.4575930727758,11.1547886743356,76.5110076457537));
#49804=CARTESIAN_POINT('Ctrl Pts',(28.9183017155932,11.1547886743356,76.3909129102924));
#49805=CARTESIAN_POINT('Ctrl Pts',(29.3799731095367,11.1547886743356,76.2906947846657));
#49806=CARTESIAN_POINT('Ctrl Pts',(29.927559751678,11.1547886743356,76.2567707916463));
#49807=CARTESIAN_POINT('Ctrl Pts',(30.4012178328891,11.1547886743356,76.3354590540619));
#49808=CARTESIAN_POINT('Ctrl Pts',(30.8536961803639,11.1547886743356,76.436262411816));
#49809=CARTESIAN_POINT('Ctrl Pts',(31.2142983985893,11.1547886743356,76.513842553578));
#49810=CARTESIAN_POINT('Ctrl Pts',(31.6283741100523,11.1547886743356,76.5452299621935));
#49811=CARTESIAN_POINT('Ctrl Pts',(32.0378187127339,11.1547886743356,76.4832076107804));
#49812=CARTESIAN_POINT('Ctrl Pts',(32.4191148073684,11.1547886743356,76.3292342878522));
#49813=CARTESIAN_POINT('Ctrl Pts',(32.7282509419986,11.1547886743356,76.1053043705975));
#49814=CARTESIAN_POINT('Ctrl Pts',(32.8757489865211,11.1547886743356,75.9172707791943));
#49815=CARTESIAN_POINT('Ctrl Pts',(32.9354103282424,11.1547886743356,75.8130319483797));
#49816=CARTESIAN_POINT('Ctrl Pts',(32.5998127104383,11.1547519764034,74.675399726197));
#49817=CARTESIAN_POINT('Ctrl Pts',(32.2761703317871,11.1547519764034,74.6762122545718));
#49818=CARTESIAN_POINT('Ctrl Pts',(31.6098016250815,11.1547519764034,74.6762655556816));
#49819=CARTESIAN_POINT('Ctrl Pts',(30.6650006393167,11.1547519764034,74.6734698551145));
#49820=CARTESIAN_POINT('Ctrl Pts',(29.7869986347378,11.1547519764034,74.6762289478734));
#49821=CARTESIAN_POINT('Ctrl Pts',(29.0365465597985,11.1547519764034,74.6757995710693));
#49822=CARTESIAN_POINT('Ctrl Pts',(28.4685779768367,11.1547519764034,74.6707544766575));
#49823=CARTESIAN_POINT('Ctrl Pts',(28.0465742254224,11.1547519764034,74.7021446137878));
#49824=CARTESIAN_POINT('Ctrl Pts',(27.7399845926101,11.1547519764034,74.7630453197478));
#49825=CARTESIAN_POINT('Ctrl Pts',(27.4477301966082,11.1547519764034,74.8755940064442));
#49826=CARTESIAN_POINT('Ctrl Pts',(27.1862980568975,11.1547519764034,75.0471516780439));
#49827=CARTESIAN_POINT('Ctrl Pts',(26.9848226471612,11.1547519764034,75.2752364149403));
#49828=CARTESIAN_POINT('Ctrl Pts',(26.8562056693994,11.1547519764034,75.5956582649194));
#49829=CARTESIAN_POINT('Ctrl Pts',(26.8969665026836,11.1547519764034,75.991342012992));
#49830=CARTESIAN_POINT('Ctrl Pts',(27.1501552309397,11.1547519764034,76.3769645604685));
#49831=CARTESIAN_POINT('Ctrl Pts',(27.5415685701483,11.1547519764034,76.6359212457116));
#49832=CARTESIAN_POINT('Ctrl Pts',(28.0093531063722,11.1547519764034,76.719754552362));
#49833=CARTESIAN_POINT('Ctrl Pts',(28.4905724048262,11.1547519764034,76.6564131286137));
#49834=CARTESIAN_POINT('Ctrl Pts',(28.9563968556498,11.1547519764034,76.5348754632395));
#49835=CARTESIAN_POINT('Ctrl Pts',(29.4025464173009,11.1547519764034,76.4386618160109));
#49836=CARTESIAN_POINT('Ctrl Pts',(29.9173288517,11.1547519764034,76.4067284088812));
#49837=CARTESIAN_POINT('Ctrl Pts',(30.3712611887102,11.1547519764034,76.4814520763918));
#49838=CARTESIAN_POINT('Ctrl Pts',(30.8205182721765,11.1547519764034,76.5814778598802));
#49839=CARTESIAN_POINT('Ctrl Pts',(31.1892658528984,11.1547519764034,76.6611892897302));
#49840=CARTESIAN_POINT('Ctrl Pts',(31.6330040350096,11.1547519764034,76.6955847221156));
#49841=CARTESIAN_POINT('Ctrl Pts',(32.0778173300849,11.1547519764034,76.6281454474494));
#49842=CARTESIAN_POINT('Ctrl Pts',(32.4905239707925,11.1547519764034,76.4615713425828));
#49843=CARTESIAN_POINT('Ctrl Pts',(32.8318023169732,11.1547519764034,76.215277917134));
#49844=CARTESIAN_POINT('Ctrl Pts',(32.9979357110749,11.1547519764034,76.0037858932076));
#49845=CARTESIAN_POINT('Ctrl Pts',(33.0647455994769,11.1547519764034,75.8870572972199));
#49846=CARTESIAN_POINT('Ctrl Pts',(32.5995793969032,11.0382369119409,74.5824674055347));
#49847=CARTESIAN_POINT('Ctrl Pts',(32.2760834569175,11.0382369119409,74.5832795662643));
#49848=CARTESIAN_POINT('Ctrl Pts',(31.6100447742661,11.0382369119409,74.5833249600566));
#49849=CARTESIAN_POINT('Ctrl Pts',(30.6650272601934,11.0382369119409,74.5805474438346));
#49850=CARTESIAN_POINT('Ctrl Pts',(29.7865142837032,11.0382369119409,74.5832772107547));
#49851=CARTESIAN_POINT('Ctrl Pts',(29.0372939426096,11.0382369119409,74.582910995395));
#49852=CARTESIAN_POINT('Ctrl Pts',(28.468053931887,11.0382369119409,74.5777284883834));
#49853=CARTESIAN_POINT('Ctrl Pts',(28.0349391340773,11.0382369119409,74.6097207938168));
#49854=CARTESIAN_POINT('Ctrl Pts',(27.7146308371164,11.0382369119409,74.6731772220513));
#49855=CARTESIAN_POINT('Ctrl Pts',(27.4055137767683,11.0382369119409,74.7920021444151));
#49856=CARTESIAN_POINT('Ctrl Pts',(27.1256919469879,11.0382369119409,74.9753727265389));
#49857=CARTESIAN_POINT('Ctrl Pts',(26.9049463387008,11.0382369119409,75.2240034592021));
#49858=CARTESIAN_POINT('Ctrl Pts',(26.7599568542985,11.0382369119409,75.583717079632));
#49859=CARTESIAN_POINT('Ctrl Pts',(26.8069857607438,11.0382369119409,76.0264862337433));
#49860=CARTESIAN_POINT('Ctrl Pts',(27.0829164167005,11.0382369119409,76.444235771622));
#49861=CARTESIAN_POINT('Ctrl Pts',(27.5064216534128,11.0382369119409,76.7249710719503));
#49862=CARTESIAN_POINT('Ctrl Pts',(28.0102448183053,11.0382369119409,76.8141524030629));
#49863=CARTESIAN_POINT('Ctrl Pts',(28.5111373421305,11.0382369119409,76.7470820576527));
#49864=CARTESIAN_POINT('Ctrl Pts',(28.9801524650468,11.0382369119409,76.6246455409694));
#49865=CARTESIAN_POINT('Ctrl Pts',(29.4166238712801,11.0382369119409,76.5309292146735));
#49866=CARTESIAN_POINT('Ctrl Pts',(29.910952277248,11.0382369119409,76.5002375601232));
#49867=CARTESIAN_POINT('Ctrl Pts',(30.3525861743777,11.0382369119409,76.5724900673701));
#49868=CARTESIAN_POINT('Ctrl Pts',(30.7998347185052,11.0382369119409,76.6720309332793));
#49869=CARTESIAN_POINT('Ctrl Pts',(31.1736622761221,11.0382369119409,76.7530716442971));
#49870=CARTESIAN_POINT('Ctrl Pts',(31.6358970252485,11.0382369119409,76.789342779067));
#49871=CARTESIAN_POINT('Ctrl Pts',(32.102765168382,11.0382369119409,76.7185259550485));
#49872=CARTESIAN_POINT('Ctrl Pts',(32.5350586903318,11.0382369119409,76.5440947520284));
#49873=CARTESIAN_POINT('Ctrl Pts',(32.8963798993568,11.0382369119409,76.2838567705243));
#49874=CARTESIAN_POINT('Ctrl Pts',(33.0741342976736,11.0382369119409,76.0577374019553));
#49875=CARTESIAN_POINT('Ctrl Pts',(33.1454015877907,11.0382369119409,75.9332209431765));
#49876=CARTESIAN_POINT('Ctrl Pts',(32.5996628076132,10.8930228127602,74.6156911567283));
#49877=CARTESIAN_POINT('Ctrl Pts',(32.2761145887457,10.8930228127602,74.6165034487079));
#49878=CARTESIAN_POINT('Ctrl Pts',(31.6099595038204,10.8930228127602,74.6165440657868));
#49879=CARTESIAN_POINT('Ctrl Pts',(30.6650207633387,10.8930228127602,74.6137522372086));
#49880=CARTESIAN_POINT('Ctrl Pts',(29.7866909415064,10.8930228127602,74.6164885561164));
#49881=CARTESIAN_POINT('Ctrl Pts',(29.0370312139308,10.8930228127602,74.6160979687152));
#49882=CARTESIAN_POINT('Ctrl Pts',(28.4682462358672,10.8930228127602,74.6109585365518));
#49883=CARTESIAN_POINT('Ctrl Pts',(28.03909842628,10.8930228127602,74.6427341806224));
#49884=CARTESIAN_POINT('Ctrl Pts',(27.723688010425,10.8930228127602,74.7052763109341));
#49885=CARTESIAN_POINT('Ctrl Pts',(27.4205912155809,10.8930228127602,74.8218589376446));
#49886=CARTESIAN_POINT('Ctrl Pts',(27.1473345686385,10.8930228127602,75.0010108373297));
#49887=CARTESIAN_POINT('Ctrl Pts',(26.9334684899571,10.8930228127602,75.2423050500824));
#49888=CARTESIAN_POINT('Ctrl Pts',(26.794323653363,10.8930228127602,75.5879891555652));
#49889=CARTESIAN_POINT('Ctrl Pts',(26.8391136919026,10.8930228127602,76.0139430513525));
#49890=CARTESIAN_POINT('Ctrl Pts',(27.1069244172984,10.8930228127602,76.4202212440923));
#49891=CARTESIAN_POINT('Ctrl Pts',(27.5189700615504,10.8930228127602,76.6931758299514));
#49892=CARTESIAN_POINT('Ctrl Pts',(28.0099249004793,10.8930228127602,76.7804444358118));
#49893=CARTESIAN_POINT('Ctrl Pts',(28.5037916195392,10.8930228127602,76.7147018584722));
#49894=CARTESIAN_POINT('Ctrl Pts',(28.9716646686748,10.8930228127602,76.5925828067522));
#49895=CARTESIAN_POINT('Ctrl Pts',(29.4115899334285,10.8930228127602,76.4979734783621));
#49896=CARTESIAN_POINT('Ctrl Pts',(29.9132177445037,10.8930228127602,76.4668363814021));
#49897=CARTESIAN_POINT('Ctrl Pts',(30.3592369373731,10.8930228127602,76.539967478678));
#49898=CARTESIAN_POINT('Ctrl Pts',(30.8072023523051,10.8930228127602,76.6396817330575));
#49899=CARTESIAN_POINT('Ctrl Pts',(31.1792123387399,10.8930228127602,76.7202465580442));
#49900=CARTESIAN_POINT('Ctrl Pts',(31.634840468396,10.8930228127602,76.7558477472188));
#49901=CARTESIAN_POINT('Ctrl Pts',(32.0938307914786,10.8930228127602,76.686236256697));
#49902=CARTESIAN_POINT('Ctrl Pts',(32.5191271929452,10.8930228127602,76.5146100998322));
#49903=CARTESIAN_POINT('Ctrl Pts',(32.8732894407117,10.8930228127602,76.259350444784));
#49904=CARTESIAN_POINT('Ctrl Pts',(33.046890695164,10.8930228127602,76.0384533948912));
#49905=CARTESIAN_POINT('Ctrl Pts',(33.1165666844017,10.8930228127602,75.9167172179222));
#49906=CARTESIAN_POINT('Ctrl Pts',(32.599887326025,10.85,74.7051202463867));
#49907=CARTESIAN_POINT('Ctrl Pts',(32.2761981190515,10.85,74.7059328923275));
#49908=CARTESIAN_POINT('Ctrl Pts',(31.6097239532025,10.85,74.7059883126997));
#49909=CARTESIAN_POINT('Ctrl Pts',(30.6649922884241,10.85,74.7031863758766));
#49910=CARTESIAN_POINT('Ctrl Pts',(29.7871537227045,10.85,74.7059546354782));
#49911=CARTESIAN_POINT('Ctrl Pts',(29.0363077810949,10.85,74.7055049626261));
#49912=CARTESIAN_POINT('Ctrl Pts',(28.4687458376382,10.85,74.7005034879709));
#49913=CARTESIAN_POINT('Ctrl Pts',(28.0502952066557,10.85,74.7317009722169));
#49914=CARTESIAN_POINT('Ctrl Pts',(27.7480925595316,10.85,74.791784304059));
#49915=CARTESIAN_POINT('Ctrl Pts',(27.4612305395664,10.85,74.9023258791797));
#49916=CARTESIAN_POINT('Ctrl Pts',(27.2056790773174,10.85,75.0701059267153));
#49917=CARTESIAN_POINT('Ctrl Pts',(27.0103659152346,10.85,75.29162035776));
#49918=CARTESIAN_POINT('Ctrl Pts',(26.8869845363635,10.85,75.599477318155));
#49919=CARTESIAN_POINT('Ctrl Pts',(26.9257408959584,10.85,75.9801037358516));
#49920=CARTESIAN_POINT('Ctrl Pts',(27.1716571299138,10.85,76.355452572985));
#49921=CARTESIAN_POINT('Ctrl Pts',(27.5528079390515,10.85,76.6074445605929));
#49922=CARTESIAN_POINT('Ctrl Pts',(28.0090678688855,10.85,76.6895674829939));
#49923=CARTESIAN_POINT('Ctrl Pts',(28.4839959103718,10.85,76.6274183114511));
#49924=CARTESIAN_POINT('Ctrl Pts',(28.9487998829859,10.85,76.5061678971924));
#49925=CARTESIAN_POINT('Ctrl Pts',(29.3980442681989,10.85,76.4091555755402));
#49926=CARTESIAN_POINT('Ctrl Pts',(29.9193673683687,10.85,76.3768249643973));
#49927=CARTESIAN_POINT('Ctrl Pts',(30.3772322305165,10.85,76.4523386674084));
#49928=CARTESIAN_POINT('Ctrl Pts',(30.8271315971887,10.85,76.5525195330394));
#49929=CARTESIAN_POINT('Ctrl Pts',(31.1942544811605,10.85,76.6318058122052));
#49930=CARTESIAN_POINT('Ctrl Pts',(31.6320776318315,10.85,76.665601413321));
#49931=CARTESIAN_POINT('Ctrl Pts',(32.0698379765199,10.85,76.599242190541));
#49932=CARTESIAN_POINT('Ctrl Pts',(32.4762808561744,10.85,76.435180639965));
#49933=CARTESIAN_POINT('Ctrl Pts',(32.8111496779181,10.85,76.193346425483));
#49934=CARTESIAN_POINT('Ctrl Pts',(32.9735666558701,10.85,75.9865319681108));
#49935=CARTESIAN_POINT('Ctrl Pts',(33.038951151302,10.85,75.8722937837091));
#49936=CARTESIAN_POINT('Ctrl Pts',(32.6,10.85,74.75));
#49937=CARTESIAN_POINT('Ctrl Pts',(32.2762401972932,10.85,74.7508128231767));
#49938=CARTESIAN_POINT('Ctrl Pts',(31.6096093142576,10.85,74.7508592792408));
#49939=CARTESIAN_POINT('Ctrl Pts',(30.6649845099545,10.85,74.7480354284176));
#49940=CARTESIAN_POINT('Ctrl Pts',(29.7873935141465,10.85,74.7508112397276));
#49941=CARTESIAN_POINT('Ctrl Pts',(29.0359543531313,10.85,74.7503280524995));
#49942=CARTESIAN_POINT('Ctrl Pts',(28.4690072452371,10.85,74.7453827659742));
#49943=CARTESIAN_POINT('Ctrl Pts',(28.0559136155584,10.85,74.7762871198526));
#49944=CARTESIAN_POINT('Ctrl Pts',(27.7603250073182,10.85,74.8351351843659));
#49945=CARTESIAN_POINT('Ctrl Pts',(27.4815926484957,10.85,74.9426482833623));
#49946=CARTESIAN_POINT('Ctrl Pts',(27.2349066090381,10.85,75.1047310768146));
#49947=CARTESIAN_POINT('Ctrl Pts',(27.0488833547682,10.85,75.316337989367));
#49948=CARTESIAN_POINT('Ctrl Pts',(26.9333942799495,10.85,75.6052491869369));
#49949=CARTESIAN_POINT('Ctrl Pts',(26.9691269620806,10.85,75.9631669379198));
#49950=CARTESIAN_POINT('Ctrl Pts',(27.2040779638452,10.85,76.3230245921545));
#49951=CARTESIAN_POINT('Ctrl Pts',(27.5697532039707,10.85,76.564507863235));
#49952=CARTESIAN_POINT('Ctrl Pts',(28.0086353410587,10.85,76.644046754502));
#49953=CARTESIAN_POINT('Ctrl Pts',(28.4740751575422,10.85,76.5836894126618));
#49954=CARTESIAN_POINT('Ctrl Pts',(28.9373359185006,10.85,76.4628665594052));
#49955=CARTESIAN_POINT('Ctrl Pts',(29.391243866756,10.85,76.3646478753146));
#49956=CARTESIAN_POINT('Ctrl Pts',(29.9224229501769,10.85,76.3317150468999));
#49957=CARTESIAN_POINT('Ctrl Pts',(30.3862078321633,10.85,76.4084139727046));
#49958=CARTESIAN_POINT('Ctrl Pts',(30.8370751782289,10.85,76.5088290665611));
#49959=CARTESIAN_POINT('Ctrl Pts',(31.2017423456432,10.85,76.5874722844094));
#49960=CARTESIAN_POINT('Ctrl Pts',(31.6306430333322,10.85,76.6203631077507));
#49961=CARTESIAN_POINT('Ctrl Pts',(32.057764032766,10.85,76.5556313773306));
#49962=CARTESIAN_POINT('Ctrl Pts',(32.4547567135938,10.85,76.3953576871574));
#49963=CARTESIAN_POINT('Ctrl Pts',(32.7799571046759,10.85,76.160246076731));
#49964=CARTESIAN_POINT('Ctrl Pts',(32.936764346482,10.85,75.9604837805911));
#49965=CARTESIAN_POINT('Ctrl Pts',(33.,10.85,75.85));
#49966=CARTESIAN_POINT('',(32.6,10.85,74.75));
#49967=CARTESIAN_POINT('Origin',(32.6,11.,74.75));
#49968=CARTESIAN_POINT('',(33.,10.85,75.85));
#49969=CARTESIAN_POINT('Ctrl Pts',(32.6,10.85,74.75));
#49970=CARTESIAN_POINT('Ctrl Pts',(32.2762401972932,10.85,74.7508128231767));
#49971=CARTESIAN_POINT('Ctrl Pts',(31.6096093142576,10.85,74.7508592792408));
#49972=CARTESIAN_POINT('Ctrl Pts',(30.6649845099545,10.85,74.7480354284176));
#49973=CARTESIAN_POINT('Ctrl Pts',(29.7873935141465,10.85,74.7508112397276));
#49974=CARTESIAN_POINT('Ctrl Pts',(29.0359543531313,10.85,74.7503280524995));
#49975=CARTESIAN_POINT('Ctrl Pts',(28.4690072452371,10.85,74.7453827659742));
#49976=CARTESIAN_POINT('Ctrl Pts',(28.0559136155584,10.85,74.7762871198526));
#49977=CARTESIAN_POINT('Ctrl Pts',(27.7603250073182,10.85,74.8351351843659));
#49978=CARTESIAN_POINT('Ctrl Pts',(27.4815926484957,10.85,74.9426482833623));
#49979=CARTESIAN_POINT('Ctrl Pts',(27.2349066090381,10.85,75.1047310768146));
#49980=CARTESIAN_POINT('Ctrl Pts',(27.0488833547682,10.85,75.316337989367));
#49981=CARTESIAN_POINT('Ctrl Pts',(26.9333942799495,10.85,75.6052491869369));
#49982=CARTESIAN_POINT('Ctrl Pts',(26.9691269620806,10.85,75.9631669379198));
#49983=CARTESIAN_POINT('Ctrl Pts',(27.2040779638452,10.85,76.3230245921545));
#49984=CARTESIAN_POINT('Ctrl Pts',(27.5697532039707,10.85,76.564507863235));
#49985=CARTESIAN_POINT('Ctrl Pts',(28.0086353410587,10.85,76.644046754502));
#49986=CARTESIAN_POINT('Ctrl Pts',(28.4740751575422,10.85,76.5836894126618));
#49987=CARTESIAN_POINT('Ctrl Pts',(28.9373359185006,10.85,76.4628665594052));
#49988=CARTESIAN_POINT('Ctrl Pts',(29.391243866756,10.85,76.3646478753146));
#49989=CARTESIAN_POINT('Ctrl Pts',(29.9224229501769,10.85,76.3317150468999));
#49990=CARTESIAN_POINT('Ctrl Pts',(30.3862078321633,10.85,76.4084139727046));
#49991=CARTESIAN_POINT('Ctrl Pts',(30.8370751782289,10.85,76.5088290665611));
#49992=CARTESIAN_POINT('Ctrl Pts',(31.2017423456432,10.85,76.5874722844094));
#49993=CARTESIAN_POINT('Ctrl Pts',(31.6306430333322,10.85,76.6203631077507));
#49994=CARTESIAN_POINT('Ctrl Pts',(32.057764032766,10.85,76.5556313773306));
#49995=CARTESIAN_POINT('Ctrl Pts',(32.4547567135938,10.85,76.3953576871574));
#49996=CARTESIAN_POINT('Ctrl Pts',(32.7799571046759,10.85,76.160246076731));
#49997=CARTESIAN_POINT('Ctrl Pts',(32.936764346482,10.85,75.9604837805911));
#49998=CARTESIAN_POINT('Ctrl Pts',(33.,10.85,75.85));
#49999=CARTESIAN_POINT('Origin',(33.,11.,75.85));
#50000=CARTESIAN_POINT('Origin',(33.,11.,75.85));
#50001=CARTESIAN_POINT('Origin',(32.6,11.,74.75));
#50002=CARTESIAN_POINT('',(0.,0.,0.));
#50003=CARTESIAN_POINT('Origin',(30.75,9.51646399110419,18.4280916795304));
#50004=CARTESIAN_POINT('',(30.8,4.8,24.1560450044147));
#50005=CARTESIAN_POINT('',(30.7,4.8,24.));
#50006=CARTESIAN_POINT('',(24.6978189959578,4.8,14.6338963872653));
#50007=CARTESIAN_POINT('',(30.7,24.,1.));
#50008=CARTESIAN_POINT('',(30.7,9.4780802994519,18.3960496412816));
#50009=CARTESIAN_POINT('',(30.8,24.1302636558592,1.));
#50010=CARTESIAN_POINT('',(21.980595587918,12.6417850436725,0.999999999999998));
#50011=CARTESIAN_POINT('',(30.8,9.55484768275647,18.4601337177793));
#50012=CARTESIAN_POINT('Origin',(30.,4.8,24.));
#50013=CARTESIAN_POINT('',(29.3,4.8,24.));
#50014=CARTESIAN_POINT('',(32.,4.8,24.));
#50015=CARTESIAN_POINT('',(29.3,24.,1.));
#50016=CARTESIAN_POINT('',(29.3,9.4780802994519,18.3960496412816));
#50017=CARTESIAN_POINT('',(31.875,24.,1.));
#50018=CARTESIAN_POINT('Origin',(29.25,9.51646399110419,18.4280916795304));
#50019=CARTESIAN_POINT('',(29.2,24.1302636558592,1.));
#50020=CARTESIAN_POINT('',(39.4099093747916,10.8304624443433,1.));
#50021=CARTESIAN_POINT('',(29.2,4.8,24.1560450044147));
#50022=CARTESIAN_POINT('',(36.4666627932199,4.8,12.8167807279347));
#50023=CARTESIAN_POINT('',(29.2,9.55484768275647,18.4601337177793));
#50024=CARTESIAN_POINT('Origin',(30.75,-19.1164639911042,6.92809167953045));
#50025=CARTESIAN_POINT('',(30.8,-24.1302636558592,1.));
#50026=CARTESIAN_POINT('',(30.7,-24.,1.));
#50027=CARTESIAN_POINT('',(24.2990885150594,-15.6619386914043,1.));
#50028=CARTESIAN_POINT('',(30.7,-4.8,24.));
#50029=CARTESIAN_POINT('',(30.7,-19.0780802994519,6.89604964128158));
#50030=CARTESIAN_POINT('',(30.8,-4.8,24.1560450044147));
#50031=CARTESIAN_POINT('',(20.9212334464924,-4.8,8.74072329987777));
#50032=CARTESIAN_POINT('',(30.8,-19.1548476827565,6.96013371777932));
#50033=CARTESIAN_POINT('Origin',(30.,-24.,1.));
#50034=CARTESIAN_POINT('',(29.3,-24.,1.));
#50035=CARTESIAN_POINT('',(31.875,-24.,1.));
#50036=CARTESIAN_POINT('',(29.3,-4.8,24.));
#50037=CARTESIAN_POINT('',(29.3,-19.0780802994519,6.89604964128158));
#50038=CARTESIAN_POINT('',(28.,-4.8,24.));
#50039=CARTESIAN_POINT('Origin',(29.25,-19.1164639911042,6.92809167953045));
#50040=CARTESIAN_POINT('',(29.2,-4.8,24.1560450044147));
#50041=CARTESIAN_POINT('',(37.9142847643299,-4.8,10.5578389592083));
#50042=CARTESIAN_POINT('',(29.2,-24.1302636558592,1.));
#50043=CARTESIAN_POINT('',(37.0914164476502,-13.850616092075,0.999999999999999));
#50044=CARTESIAN_POINT('',(29.2,-19.1548476827565,6.96013371777932));
#50045=CARTESIAN_POINT('Origin',(30.75,-11.0622585189423,22.7172039543912));
#50046=CARTESIAN_POINT('',(30.7,-30.,1.));
#50047=CARTESIAN_POINT('',(30.8,-29.8675197724128,1.));
#50048=CARTESIAN_POINT('',(35.1351844799295,-24.124257507079,1.));
#50049=CARTESIAN_POINT('',(30.8,-4.8,29.847542595237));
#50050=CARTESIAN_POINT('',(30.8,-11.0245170378846,22.6844079087825));
#50051=CARTESIAN_POINT('',(30.7298992862524,-4.8,29.954416324137));
#50052=CARTESIAN_POINT('',(38.3204633389669,-4.8,18.382039362495));
#50053=CARTESIAN_POINT('',(30.7,-4.86559209121751,29.9245170378846));
#50054=CARTESIAN_POINT('',(29.1417160738286,-8.28410518097803,28.3662331117132));
#50055=CARTESIAN_POINT('',(30.7,-11.1,22.75));
#50056=CARTESIAN_POINT('Origin',(30.,-4.78279604560876,29.9622585189423));
#50057=CARTESIAN_POINT('',(30.8,-4.8,29.954416324137));
#50058=CARTESIAN_POINT('',(28.,-4.8,29.954416324137));
#50059=CARTESIAN_POINT('',(30.8,-4.7,30.));
#50060=CARTESIAN_POINT('',(30.8,-12.7352042956433,26.3372585189423));
#50061=CARTESIAN_POINT('',(29.2,-4.7,30.));
#50062=CARTESIAN_POINT('',(30.,-4.7,30.));
#50063=CARTESIAN_POINT('',(29.2,-4.8,29.954416324137));
#50064=CARTESIAN_POINT('',(29.2,-12.7352042956433,26.3372585189423));
#50065=CARTESIAN_POINT('',(29.2701007137476,-4.8,29.954416324137));
#50066=CARTESIAN_POINT('',(28.,-4.8,29.954416324137));
#50067=CARTESIAN_POINT('',(29.3,-4.86559209121751,29.9245170378846));
#50068=CARTESIAN_POINT('',(30.8582839261714,-8.28410518097803,28.3662331117132));
#50069=CARTESIAN_POINT('',(30.,-4.86559209121751,29.9245170378846));
#50070=CARTESIAN_POINT('Origin',(30.8,-17.4,15.5));
#50071=CARTESIAN_POINT('',(30.8,-4.8,29.9));
#50072=CARTESIAN_POINT('',(30.8,-4.8,8.25));
#50073=CARTESIAN_POINT('',(30.8,-11.5249999999999,23.1749999999999));
#50074=CARTESIAN_POINT('Origin',(29.25,-11.0622585189423,22.7172039543912));
#50075=CARTESIAN_POINT('',(29.2,-4.8,29.847542595237));
#50076=CARTESIAN_POINT('',(20.4762852446965,-4.8,16.547593480374));
#50077=CARTESIAN_POINT('',(29.2,-29.8675197724128,1.));
#50078=CARTESIAN_POINT('',(29.2,-11.0245170378846,22.6844079087825));
#50079=CARTESIAN_POINT('',(29.3,-30.,1.));
#50080=CARTESIAN_POINT('',(24.8648155200705,-24.124257507079,1.));
#50081=CARTESIAN_POINT('',(29.3,-11.1,22.75));
#50082=CARTESIAN_POINT('Origin',(29.2,-17.4,15.5));
#50083=CARTESIAN_POINT('',(29.2,-4.8,29.9));
#50084=CARTESIAN_POINT('',(29.2,-4.8,8.25));
#50085=CARTESIAN_POINT('',(29.2,-11.5249999999999,23.1749999999999));
#50086=CARTESIAN_POINT('Origin',(29.2,-17.4,15.5));
#50087=CARTESIAN_POINT('',(29.2,-29.7,1.));
#50088=CARTESIAN_POINT('',(29.2,-8.7,1.));
#50089=CARTESIAN_POINT('',(29.2,-29.8707106781187,0.929289321881342));
#50090=CARTESIAN_POINT('',(29.2,-21.9300622355798,4.21841360081793));
#50091=CARTESIAN_POINT('',(29.2,-29.8,1.));
#50092=CARTESIAN_POINT('',(29.2,-23.125,7.67500000000001));
#50093=CARTESIAN_POINT('',(29.2,-24.,1.));
#50094=CARTESIAN_POINT('',(29.2,-4.8,8.25));
#50095=CARTESIAN_POINT('Origin',(30.,-4.4,30.));
#50096=CARTESIAN_POINT('',(33.9,-4.7,30.));
#50097=CARTESIAN_POINT('',(28.,-4.7,30.));
#50098=CARTESIAN_POINT('',(33.9,-4.1,30.));
#50099=CARTESIAN_POINT('',(33.9,-4.6,30.));
#50100=CARTESIAN_POINT('',(26.1,-4.1,30.));
#50101=CARTESIAN_POINT('',(32.,-4.1,30.));
#50102=CARTESIAN_POINT('',(26.1,-4.7,30.));
#50103=CARTESIAN_POINT('',(26.1,-4.2,30.));
#50104=CARTESIAN_POINT('',(28.,-4.7,30.));
#50105=CARTESIAN_POINT('Origin',(33.95,-4.6,29.95));
#50106=CARTESIAN_POINT('',(33.95,-4.05,29.95));
#50107=CARTESIAN_POINT('',(33.5333333333333,-4.46666666666666,30.3666666666667));
#50108=CARTESIAN_POINT('',(33.95,-4.75,29.95));
#50109=CARTESIAN_POINT('',(32.9333333333333,-3.73333333333334,30.9666666666667));
#50110=CARTESIAN_POINT('',(34.,-4.7,29.9));
#50111=CARTESIAN_POINT('',(38.8000000000001,0.0999999999999677,25.0999999999999));
#50112=CARTESIAN_POINT('',(34.,-4.1,29.9));
#50113=CARTESIAN_POINT('',(34.,-4.6,29.9));
#50114=CARTESIAN_POINT('',(38.8666666666665,-8.96666666666676,25.0333333333335));
#50115=CARTESIAN_POINT('Origin',(32.,-4.05,29.95));
#50116=CARTESIAN_POINT('',(33.9,-4.,29.9));
#50117=CARTESIAN_POINT('',(33.9,-4.,29.9));
#50118=CARTESIAN_POINT('',(26.1,-4.,29.9));
#50119=CARTESIAN_POINT('',(32.,-4.,29.9));
#50120=CARTESIAN_POINT('',(26.05,-4.05,29.95));
#50121=CARTESIAN_POINT('',(26.,-4.1,30.));
#50122=CARTESIAN_POINT('',(27.0666666666667,-5.06666666666666,30.9666666666667));
#50123=CARTESIAN_POINT('Origin',(33.95,-4.05,1.));
#50124=CARTESIAN_POINT('',(34.,-4.1,1.));
#50125=CARTESIAN_POINT('',(34.,-4.1,1.));
#50126=CARTESIAN_POINT('',(33.9,-4.,1.));
#50127=CARTESIAN_POINT('',(32.8875,-2.98749999999995,1.));
#50128=CARTESIAN_POINT('',(33.9,-4.,1.));
#50129=CARTESIAN_POINT('Origin',(26.05,-4.2,29.95));
#50130=CARTESIAN_POINT('',(26.05,-4.75,29.95));
#50131=CARTESIAN_POINT('',(26.4666666666667,-4.33333333333334,30.3666666666667));
#50132=CARTESIAN_POINT('',(26.,-4.1,29.9));
#50133=CARTESIAN_POINT('',(21.1999999999999,-8.89999999999997,25.0999999999999));
#50134=CARTESIAN_POINT('',(26.,-4.7,29.9));
#50135=CARTESIAN_POINT('',(26.,-4.2,29.9));
#50136=CARTESIAN_POINT('',(21.1333333333333,0.166666666666632,25.0333333333333));
#50137=CARTESIAN_POINT('Origin',(28.,-4.75,29.95));
#50138=CARTESIAN_POINT('',(26.1,-4.8,29.9));
#50139=CARTESIAN_POINT('',(26.1,-4.8,29.9));
#50140=CARTESIAN_POINT('',(28.,-4.8,29.9));
#50141=CARTESIAN_POINT('Origin',(26.05,-4.75,1.));
#50142=CARTESIAN_POINT('',(26.,-4.7,1.));
#50143=CARTESIAN_POINT('',(26.,-4.7,1.));
#50144=CARTESIAN_POINT('',(26.1,-4.8,1.));
#50145=CARTESIAN_POINT('',(26.7875,-5.48750000000002,1.));
#50146=CARTESIAN_POINT('',(26.1,-4.8,1.));
#50147=CARTESIAN_POINT('Origin',(30.75,23.6622585189423,8.21720395439124));
#50148=CARTESIAN_POINT('',(30.7,4.86559209121751,29.9245170378846));
#50149=CARTESIAN_POINT('',(30.7298992862524,4.8,29.954416324137));
#50150=CARTESIAN_POINT('',(26.0488170169426,15.0692075193245,25.2733340548267));
#50151=CARTESIAN_POINT('',(30.8,4.8,29.847542595237));
#50152=CARTESIAN_POINT('',(42.8486479166477,4.8,11.4784866724842));
#50153=CARTESIAN_POINT('',(30.8,29.8675197724128,1.));
#50154=CARTESIAN_POINT('',(30.8,23.6245170378846,8.18440790878249));
#50155=CARTESIAN_POINT('',(30.7,30.,1.));
#50156=CARTESIAN_POINT('',(33.548365194882,26.2264793073069,1.));
#50157=CARTESIAN_POINT('',(30.7,23.7,8.25));
#50158=CARTESIAN_POINT('Origin',(30.,4.78279604560876,29.9622585189423));
#50159=CARTESIAN_POINT('',(30.8,4.8,29.954416324137));
#50160=CARTESIAN_POINT('',(32.,4.8,29.954416324137));
#50161=CARTESIAN_POINT('',(29.3,4.86559209121751,29.9245170378846));
#50162=CARTESIAN_POINT('',(30.,4.86559209121751,29.9245170378846));
#50163=CARTESIAN_POINT('',(29.2701007137476,4.8,29.954416324137));
#50164=CARTESIAN_POINT('',(33.9511829830574,15.0692075193245,25.2733340548267));
#50165=CARTESIAN_POINT('',(29.2,4.8,29.954416324137));
#50166=CARTESIAN_POINT('',(32.,4.8,29.954416324137));
#50167=CARTESIAN_POINT('',(29.2,4.7,30.));
#50168=CARTESIAN_POINT('',(29.2,12.7352042956433,26.3372585189421));
#50169=CARTESIAN_POINT('',(30.8,4.7,30.));
#50170=CARTESIAN_POINT('',(30.,4.7,30.));
#50171=CARTESIAN_POINT('',(30.8,12.7352042956433,26.3372585189421));
#50172=CARTESIAN_POINT('Origin',(30.,30.,1.));
#50173=CARTESIAN_POINT('',(29.3,30.,1.));
#50174=CARTESIAN_POINT('',(30.,30.,1.));
#50175=CARTESIAN_POINT('',(29.3,23.7,8.25));
#50176=CARTESIAN_POINT('Origin',(30.8,17.4,15.5));
#50177=CARTESIAN_POINT('',(30.8,29.7,1.));
#50178=CARTESIAN_POINT('',(30.8,8.7,1.));
#50179=CARTESIAN_POINT('',(30.8,29.8707106781187,0.929289321881342));
#50180=CARTESIAN_POINT('',(30.8,21.9300622355798,4.21841360081793));
#50181=CARTESIAN_POINT('',(30.8,29.8,1.));
#50182=CARTESIAN_POINT('',(30.8,23.125,7.67500000000001));
#50183=CARTESIAN_POINT('',(30.8,24.,1.));
#50184=CARTESIAN_POINT('',(30.8,4.8,8.25));
#50185=CARTESIAN_POINT('Origin',(30.,24.,1.));
#50186=CARTESIAN_POINT('',(29.2,29.8,1.));
#50187=CARTESIAN_POINT('',(38.125,29.8,1.));
#50188=CARTESIAN_POINT('',(29.2,29.8675197724128,1.));
#50189=CARTESIAN_POINT('',(29.2,24.,1.));
#50190=CARTESIAN_POINT('',(26.451634805118,26.2264793073069,1.));
#50191=CARTESIAN_POINT('Origin',(29.25,23.6622585189423,8.21720395439124));
#50192=CARTESIAN_POINT('',(29.2,4.8,29.847542595237));
#50193=CARTESIAN_POINT('',(29.2,23.6245170378846,8.18440790878249));
#50194=CARTESIAN_POINT('',(18.3546034996889,4.8,13.3129325546051));
#50195=CARTESIAN_POINT('Origin',(29.2,17.4,15.5));
#50196=CARTESIAN_POINT('',(29.2,4.8,8.25));
#50197=CARTESIAN_POINT('',(29.2,29.8707106781187,0.929289321881342));
#50198=CARTESIAN_POINT('',(29.2,23.125,7.67500000000001));
#50199=CARTESIAN_POINT('',(29.2,29.7,1.));
#50200=CARTESIAN_POINT('',(29.2,21.9300622355798,4.21841360081793));
#50201=CARTESIAN_POINT('',(29.2,8.7,1.));
#50202=CARTESIAN_POINT('Origin',(29.2,17.4,15.5));
#50203=CARTESIAN_POINT('',(29.2,4.8,29.9));
#50204=CARTESIAN_POINT('',(29.2,4.8,8.25));
#50205=CARTESIAN_POINT('',(29.2,11.5249999999999,23.1749999999999));
#50206=CARTESIAN_POINT('Origin',(30.8,17.4,15.5));
#50207=CARTESIAN_POINT('',(30.8,4.8,29.9));
#50208=CARTESIAN_POINT('',(30.8,4.8,8.25));
#50209=CARTESIAN_POINT('',(30.8,11.5249999999999,23.1749999999999));
#50210=CARTESIAN_POINT('Origin',(30.,4.4,30.));
#50211=CARTESIAN_POINT('',(26.1,4.7,30.));
#50212=CARTESIAN_POINT('',(32.,4.7,30.));
#50213=CARTESIAN_POINT('',(26.1,4.1,30.));
#50214=CARTESIAN_POINT('',(26.1,4.6,30.));
#50215=CARTESIAN_POINT('',(33.9,4.1,30.));
#50216=CARTESIAN_POINT('',(28.,4.1,30.));
#50217=CARTESIAN_POINT('',(33.9,4.7,30.));
#50218=CARTESIAN_POINT('',(33.9,4.2,30.));
#50219=CARTESIAN_POINT('',(32.,4.7,30.));
#50220=CARTESIAN_POINT('Origin',(33.95,4.2,29.95));
#50221=CARTESIAN_POINT('',(33.95,4.75,29.95));
#50222=CARTESIAN_POINT('',(33.5333333333333,4.33333333333334,30.3666666666667));
#50223=CARTESIAN_POINT('',(33.95,4.05,29.95));
#50224=CARTESIAN_POINT('',(32.9333333333333,5.06666666666666,30.9666666666667));
#50225=CARTESIAN_POINT('',(34.,4.1,29.9));
#50226=CARTESIAN_POINT('',(38.8000000000001,8.89999999999997,25.0999999999999));
#50227=CARTESIAN_POINT('',(34.,4.7,29.9));
#50228=CARTESIAN_POINT('',(34.,4.2,29.9));
#50229=CARTESIAN_POINT('',(38.8666666666665,-0.166666666666758,25.0333333333335));
#50230=CARTESIAN_POINT('Origin',(33.95,4.05,1.));
#50231=CARTESIAN_POINT('',(33.9,4.,29.9));
#50232=CARTESIAN_POINT('',(34.,4.1,30.));
#50233=CARTESIAN_POINT('',(33.9,4.,1.));
#50234=CARTESIAN_POINT('',(33.9,4.,1.));
#50235=CARTESIAN_POINT('',(34.,4.1,1.));
#50236=CARTESIAN_POINT('',(32.8875,2.98750000000002,1.));
#50237=CARTESIAN_POINT('',(34.,4.1,1.));
#50238=CARTESIAN_POINT('Origin',(28.,4.05,29.95));
#50239=CARTESIAN_POINT('',(26.05,4.05,29.95));
#50240=CARTESIAN_POINT('',(26.4666666666667,4.46666666666666,30.3666666666667));
#50241=CARTESIAN_POINT('',(26.1,4.,29.9));
#50242=CARTESIAN_POINT('',(26.1,4.,29.9));
#50243=CARTESIAN_POINT('',(28.,4.,29.9));
#50244=CARTESIAN_POINT('Origin',(26.05,4.6,29.95));
#50245=CARTESIAN_POINT('',(26.05,4.75,29.95));
#50246=CARTESIAN_POINT('',(27.0666666666667,3.73333333333334,30.9666666666667));
#50247=CARTESIAN_POINT('',(26.,4.7,29.9));
#50248=CARTESIAN_POINT('',(21.1999999999999,-0.0999999999999677,25.0999999999999));
#50249=CARTESIAN_POINT('',(26.,4.1,29.9));
#50250=CARTESIAN_POINT('',(26.,4.6,29.9));
#50251=CARTESIAN_POINT('',(21.1333333333333,8.96666666666663,25.0333333333333));
#50252=CARTESIAN_POINT('Origin',(26.05,4.05,1.));
#50253=CARTESIAN_POINT('',(26.,4.1,1.));
#50254=CARTESIAN_POINT('',(26.,4.1,1.));
#50255=CARTESIAN_POINT('',(26.1,4.,1.));
#50256=CARTESIAN_POINT('',(28.9875,1.11250000000002,1.));
#50257=CARTESIAN_POINT('',(26.1,4.,1.));
#50258=CARTESIAN_POINT('Origin',(26.5,-28.5,0.05));
#50259=CARTESIAN_POINT('',(26.5,-29.9,0.));
#50260=CARTESIAN_POINT('',(26.5,-30.,0.1));
#50261=CARTESIAN_POINT('',(26.5,-29.9,0.));
#50262=CARTESIAN_POINT('',(25.,-28.5,0.1));
#50263=CARTESIAN_POINT('Origin',(26.5,-28.5,0.1));
#50264=CARTESIAN_POINT('',(25.1,-28.5,0.));
#50265=CARTESIAN_POINT('',(25.,-28.5,0.1));
#50266=CARTESIAN_POINT('Origin',(26.5,-28.5,0.));
#50267=CARTESIAN_POINT('Origin',(29.375,-29.95,0.05));
#50268=CARTESIAN_POINT('',(41.,-29.9,0.));
#50269=CARTESIAN_POINT('',(41.,-30.,0.1));
#50270=CARTESIAN_POINT('',(41.,-29.9,0.));
#50271=CARTESIAN_POINT('',(29.375,-30.,0.1));
#50272=CARTESIAN_POINT('',(29.375,-29.9,0.));
#50273=CARTESIAN_POINT('Origin',(41.,-28.5,0.05));
#50274=CARTESIAN_POINT('',(42.4,-28.5,0.));
#50275=CARTESIAN_POINT('',(42.5,-28.5,0.1));
#50276=CARTESIAN_POINT('',(42.4,-28.5,0.));
#50277=CARTESIAN_POINT('Origin',(41.,-28.5,0.1));
#50278=CARTESIAN_POINT('Origin',(41.,-28.5,0.));
#50279=CARTESIAN_POINT('Origin',(42.45,-15.,0.05));
#50280=CARTESIAN_POINT('',(42.4,28.5,0.));
#50281=CARTESIAN_POINT('',(42.5,28.5,0.1));
#50282=CARTESIAN_POINT('',(42.4,28.5,0.));
#50283=CARTESIAN_POINT('',(42.5,-15.,0.1));
#50284=CARTESIAN_POINT('',(42.4,-15.,0.));
#50285=CARTESIAN_POINT('Origin',(41.,28.5,0.05));
#50286=CARTESIAN_POINT('',(41.,29.9,0.));
#50287=CARTESIAN_POINT('',(41.,30.,0.1));
#50288=CARTESIAN_POINT('',(41.,29.9,0.));
#50289=CARTESIAN_POINT('Origin',(41.,28.5,0.1));
#50290=CARTESIAN_POINT('Origin',(41.,28.5,0.));
#50291=CARTESIAN_POINT('Origin',(38.125,29.95,0.05));
#50292=CARTESIAN_POINT('',(26.5,29.9,0.));
#50293=CARTESIAN_POINT('',(26.5,30.,0.1));
#50294=CARTESIAN_POINT('',(26.5,29.9,0.));
#50295=CARTESIAN_POINT('',(38.125,30.,0.1));
#50296=CARTESIAN_POINT('',(38.125,29.9,0.));
#50297=CARTESIAN_POINT('Origin',(26.5,28.5,0.05));
#50298=CARTESIAN_POINT('',(25.1,28.5,0.));
#50299=CARTESIAN_POINT('',(25.,28.5,0.1));
#50300=CARTESIAN_POINT('',(25.1,28.5,0.));
#50301=CARTESIAN_POINT('Origin',(26.5,28.5,0.1));
#50302=CARTESIAN_POINT('Origin',(26.5,28.5,0.));
#50303=CARTESIAN_POINT('Origin',(25.05,15.,0.05));
#50304=CARTESIAN_POINT('',(25.,15.,0.1));
#50305=CARTESIAN_POINT('',(25.1,15.,0.));
#50306=CARTESIAN_POINT('Origin',(42.5,30.,0.));
#50307=CARTESIAN_POINT('',(26.5,30.,0.8));
#50308=CARTESIAN_POINT('',(26.5,30.,0.));
#50309=CARTESIAN_POINT('',(41.,30.,0.8));
#50310=CARTESIAN_POINT('',(38.125,30.,0.8));
#50311=CARTESIAN_POINT('',(41.,30.,0.));
#50312=CARTESIAN_POINT('Origin',(26.5,28.5,0.));
#50313=CARTESIAN_POINT('',(25.,28.5,0.8));
#50314=CARTESIAN_POINT('',(25.,28.5,0.));
#50315=CARTESIAN_POINT('Origin',(26.5,28.5,0.8));
#50316=CARTESIAN_POINT('Origin',(25.,30.,0.));
#50317=CARTESIAN_POINT('',(25.,-28.5,0.8));
#50318=CARTESIAN_POINT('',(25.,-28.5,0.));
#50319=CARTESIAN_POINT('',(25.,15.,0.8));
#50320=CARTESIAN_POINT('Origin',(26.5,-28.5,0.));
#50321=CARTESIAN_POINT('',(26.5,-30.,0.8));
#50322=CARTESIAN_POINT('',(26.5,-30.,0.));
#50323=CARTESIAN_POINT('Origin',(26.5,-28.5,0.8));
#50324=CARTESIAN_POINT('Origin',(33.75,0.,0.));
#50325=CARTESIAN_POINT('',(38.5,-25.5,0.));
#50326=CARTESIAN_POINT('Origin',(39.5,-25.5,0.));
#50327=CARTESIAN_POINT('',(38.5,25.5,0.));
#50328=CARTESIAN_POINT('Origin',(39.5,25.5,0.));
#50329=CARTESIAN_POINT('Origin',(26.,4.8,1.));
#50330=CARTESIAN_POINT('',(26.,4.7,1.));
#50331=CARTESIAN_POINT('',(26.,4.7,1.));
#50332=CARTESIAN_POINT('',(26.,2.4,1.));
#50333=CARTESIAN_POINT('Origin',(34.,4.,1.));
#50334=CARTESIAN_POINT('',(34.,4.7,1.));
#50335=CARTESIAN_POINT('',(34.,2.,1.));
#50336=CARTESIAN_POINT('',(34.,4.7,1.));
#50337=CARTESIAN_POINT('Origin',(26.05,4.75,1.));
#50338=CARTESIAN_POINT('',(26.1,4.8,29.9));
#50339=CARTESIAN_POINT('',(26.,4.7,30.));
#50340=CARTESIAN_POINT('',(26.1,4.8,1.));
#50341=CARTESIAN_POINT('',(26.1,4.8,1.));
#50342=CARTESIAN_POINT('',(26.7875,5.48750000000002,1.));
#50343=CARTESIAN_POINT('Origin',(32.,4.75,29.95));
#50344=CARTESIAN_POINT('',(32.,4.8,29.9));
#50345=CARTESIAN_POINT('Origin',(34.,4.8,1.));
#50346=CARTESIAN_POINT('',(33.9,4.8,29.9));
#50347=CARTESIAN_POINT('',(32.,4.8,29.9));
#50348=CARTESIAN_POINT('',(33.9,4.8,1.));
#50349=CARTESIAN_POINT('',(33.9,4.8,1.));
#50350=CARTESIAN_POINT('',(33.875,4.8,1.));
#50351=CARTESIAN_POINT('',(29.025,4.8,17.));
#50352=CARTESIAN_POINT('Origin',(30.,4.8,17.));
#50353=CARTESIAN_POINT('',(29.025,4.8,6.));
#50354=CARTESIAN_POINT('Origin',(30.,4.8,6.));
#50355=CARTESIAN_POINT('Origin',(33.95,4.75,1.));
#50356=CARTESIAN_POINT('',(35.0875,3.61249999999994,1.));
#50357=CARTESIAN_POINT('',(33.9,4.8,29.9));
#50358=CARTESIAN_POINT('Origin',(32.,4.75,29.95));
#50359=CARTESIAN_POINT('Origin',(33.95,-4.75,1.));
#50360=CARTESIAN_POINT('',(33.9,-4.8,29.9));
#50361=CARTESIAN_POINT('',(34.,-4.7,30.));
#50362=CARTESIAN_POINT('',(33.9,-4.8,1.));
#50363=CARTESIAN_POINT('',(33.9,-4.8,1.));
#50364=CARTESIAN_POINT('',(34.,-4.7,1.));
#50365=CARTESIAN_POINT('',(35.0875,-3.61250000000002,1.));
#50366=CARTESIAN_POINT('',(34.,-4.7,1.));
#50367=CARTESIAN_POINT('Origin',(28.,-4.75,29.95));
#50368=CARTESIAN_POINT('',(28.,-4.8,29.9));
#50369=CARTESIAN_POINT('Origin',(26.,-4.8,1.));
#50370=CARTESIAN_POINT('',(30.8,-4.8,8.25));
#50371=CARTESIAN_POINT('',(29.875,-4.8,1.));
#50372=CARTESIAN_POINT('',(29.025,-4.8,17.));
#50373=CARTESIAN_POINT('Origin',(30.,-4.8,17.));
#50374=CARTESIAN_POINT('',(29.025,-4.8,6.));
#50375=CARTESIAN_POINT('Origin',(30.,-4.8,6.));
#50376=CARTESIAN_POINT('Origin',(26.,-4.,1.));
#50377=CARTESIAN_POINT('',(26.,-4.1,1.));
#50378=CARTESIAN_POINT('',(26.,-4.1,1.));
#50379=CARTESIAN_POINT('',(26.,-2.,1.));
#50380=CARTESIAN_POINT('Origin',(26.05,-4.05,1.));
#50381=CARTESIAN_POINT('',(26.1,-4.,1.));
#50382=CARTESIAN_POINT('',(26.1,-4.,1.));
#50383=CARTESIAN_POINT('',(28.9875,-1.11250000000002,1.));
#50384=CARTESIAN_POINT('Origin',(34.,-4.8,1.));
#50385=CARTESIAN_POINT('',(34.,-2.4,1.));
#50386=CARTESIAN_POINT('Origin',(30.,-4.05,17.));
#50387=CARTESIAN_POINT('',(29.025,-4.,17.));
#50388=CARTESIAN_POINT('Origin',(30.,-4.,17.));
#50389=CARTESIAN_POINT('',(29.125,-4.1,17.));
#50390=CARTESIAN_POINT('',(29.075,-4.05,17.));
#50391=CARTESIAN_POINT('Origin',(30.,-4.1,17.));
#50392=CARTESIAN_POINT('Origin',(30.,0.,17.));
#50393=CARTESIAN_POINT('',(29.125,-4.7,17.));
#50394=CARTESIAN_POINT('Origin',(30.,-4.7,17.));
#50395=CARTESIAN_POINT('',(29.125,0.,17.));
#50396=CARTESIAN_POINT('Origin',(34.,-4.,1.));
#50397=CARTESIAN_POINT('',(33.875,-4.,1.));
#50398=CARTESIAN_POINT('',(29.025,-4.,6.));
#50399=CARTESIAN_POINT('Origin',(30.,-4.,6.));
#50400=CARTESIAN_POINT('Origin',(30.,-4.75,17.));
#50401=CARTESIAN_POINT('',(29.075,-4.75,17.));
#50402=CARTESIAN_POINT('Origin',(30.,4.75,17.));
#50403=CARTESIAN_POINT('',(29.125,4.7,17.));
#50404=CARTESIAN_POINT('',(29.075,4.75,17.));
#50405=CARTESIAN_POINT('Origin',(30.,4.7,17.));
#50406=CARTESIAN_POINT('Origin',(30.,0.,17.));
#50407=CARTESIAN_POINT('',(29.125,4.1,17.));
#50408=CARTESIAN_POINT('Origin',(30.,4.1,17.));
#50409=CARTESIAN_POINT('',(29.125,0.,17.));
#50410=CARTESIAN_POINT('Origin',(30.,4.05,17.));
#50411=CARTESIAN_POINT('',(29.025,4.,17.));
#50412=CARTESIAN_POINT('Origin',(30.,4.,17.));
#50413=CARTESIAN_POINT('',(29.075,4.05,17.));
#50414=CARTESIAN_POINT('Origin',(26.,4.,1.));
#50415=CARTESIAN_POINT('',(29.875,4.,1.));
#50416=CARTESIAN_POINT('',(29.025,4.,6.));
#50417=CARTESIAN_POINT('Origin',(30.,4.,6.));
#50418=CARTESIAN_POINT('Origin',(30.,-4.05,6.));
#50419=CARTESIAN_POINT('',(29.125,-4.1,6.));
#50420=CARTESIAN_POINT('',(29.075,-4.05,6.));
#50421=CARTESIAN_POINT('Origin',(30.,-4.1,6.));
#50422=CARTESIAN_POINT('Origin',(30.,0.,6.));
#50423=CARTESIAN_POINT('',(29.125,-4.7,6.));
#50424=CARTESIAN_POINT('Origin',(30.,-4.7,6.));
#50425=CARTESIAN_POINT('',(29.125,0.,6.));
#50426=CARTESIAN_POINT('Origin',(30.,-4.75,6.));
#50427=CARTESIAN_POINT('',(29.075,-4.75,6.));
#50428=CARTESIAN_POINT('Origin',(30.,4.75,6.));
#50429=CARTESIAN_POINT('',(29.125,4.7,6.));
#50430=CARTESIAN_POINT('',(29.075,4.75,6.));
#50431=CARTESIAN_POINT('Origin',(30.,4.7,6.));
#50432=CARTESIAN_POINT('Origin',(30.,0.,6.));
#50433=CARTESIAN_POINT('',(29.125,4.1,6.));
#50434=CARTESIAN_POINT('Origin',(30.,4.1,6.));
#50435=CARTESIAN_POINT('',(29.125,0.,6.));
#50436=CARTESIAN_POINT('Origin',(30.,4.05,6.));
#50437=CARTESIAN_POINT('',(29.075,4.05,6.));
#50438=CARTESIAN_POINT('Origin',(39.5,-25.5,0.05));
#50439=CARTESIAN_POINT('',(38.6,-25.5,0.1));
#50440=CARTESIAN_POINT('',(38.55,-25.5,0.05));
#50441=CARTESIAN_POINT('Origin',(39.5,-25.5,0.1));
#50442=CARTESIAN_POINT('Origin',(39.5,-25.5,0.));
#50443=CARTESIAN_POINT('',(38.6,-25.5,0.9));
#50444=CARTESIAN_POINT('',(38.6,-25.5,0.));
#50445=CARTESIAN_POINT('Origin',(39.5,-25.5,0.9));
#50446=CARTESIAN_POINT('Origin',(39.5,25.5,0.05));
#50447=CARTESIAN_POINT('',(38.6,25.5,0.1));
#50448=CARTESIAN_POINT('',(38.55,25.5,0.05));
#50449=CARTESIAN_POINT('Origin',(39.5,25.5,0.1));
#50450=CARTESIAN_POINT('Origin',(39.5,25.5,0.));
#50451=CARTESIAN_POINT('',(38.6,25.5,0.9));
#50452=CARTESIAN_POINT('',(38.6,25.5,0.));
#50453=CARTESIAN_POINT('Origin',(39.5,25.5,0.9));
#50454=CARTESIAN_POINT('Origin',(31.5625,-29.7853553390593,0.964644660940671));
#50455=CARTESIAN_POINT('',(26.5,-29.7,1.));
#50456=CARTESIAN_POINT('',(31.5625,-29.7,1.));
#50457=CARTESIAN_POINT('',(26.5,-29.8707106781187,0.929289321881342));
#50458=CARTESIAN_POINT('',(26.5,-29.7,1.));
#50459=CARTESIAN_POINT('',(31.5625,-29.8707106781187,0.929289321881342));
#50460=CARTESIAN_POINT('Origin',(26.5,-28.5,0.964644660940672));
#50461=CARTESIAN_POINT('',(25.3,-28.5,1.));
#50462=CARTESIAN_POINT('',(25.1292893218813,-28.5,0.929289321881344));
#50463=CARTESIAN_POINT('',(25.3,-28.5,1.));
#50464=CARTESIAN_POINT('Origin',(26.5,-28.5,0.929289321881344));
#50465=CARTESIAN_POINT('Origin',(26.5,-28.5,1.));
#50466=CARTESIAN_POINT('Origin',(25.2146446609407,7.5,0.964644660940672));
#50467=CARTESIAN_POINT('',(25.3,28.5,1.));
#50468=CARTESIAN_POINT('',(25.1292893218813,28.5,0.929289321881344));
#50469=CARTESIAN_POINT('',(25.3,28.5,1.));
#50470=CARTESIAN_POINT('',(25.1292893218813,7.5,0.929289321881344));
#50471=CARTESIAN_POINT('',(25.3,7.5,1.));
#50472=CARTESIAN_POINT('Origin',(26.5,28.5,0.964644660940672));
#50473=CARTESIAN_POINT('',(26.5,29.7,1.));
#50474=CARTESIAN_POINT('',(26.5,29.8707106781187,0.929289321881344));
#50475=CARTESIAN_POINT('',(26.5,29.7,1.));
#50476=CARTESIAN_POINT('Origin',(26.5,28.5,0.929289321881344));
#50477=CARTESIAN_POINT('Origin',(26.5,28.5,1.));
#50478=CARTESIAN_POINT('Origin',(35.9375,29.7853553390593,0.964644660940671));
#50479=CARTESIAN_POINT('',(35.9375,29.8707106781187,0.929289321881342));
#50480=CARTESIAN_POINT('',(35.9375,29.7,1.));
#50481=CARTESIAN_POINT('Origin',(33.75,0.,1.));
#50482=CARTESIAN_POINT('',(30.8,-29.7,1.));
#50483=CARTESIAN_POINT('',(30.8,-8.7,1.));
#50484=CARTESIAN_POINT('',(41.,-29.7,1.));
#50485=CARTESIAN_POINT('',(31.5625,-29.7,1.));
#50486=CARTESIAN_POINT('',(42.2,-28.5,1.));
#50487=CARTESIAN_POINT('Origin',(41.,-28.5,1.));
#50488=CARTESIAN_POINT('',(42.2,28.5,1.));
#50489=CARTESIAN_POINT('',(42.2,-7.5,1.));
#50490=CARTESIAN_POINT('',(41.,29.7,1.));
#50491=CARTESIAN_POINT('Origin',(41.,28.5,1.));
#50492=CARTESIAN_POINT('',(35.9375,29.7,1.));
#50493=CARTESIAN_POINT('',(38.5,-25.5,1.));
#50494=CARTESIAN_POINT('Origin',(39.5,-25.5,1.));
#50495=CARTESIAN_POINT('',(38.5,25.5,1.));
#50496=CARTESIAN_POINT('Origin',(39.5,25.5,1.));
#50497=CARTESIAN_POINT('Origin',(35.9375,29.7853553390593,0.964644660940671));
#50498=CARTESIAN_POINT('',(41.,29.8707106781187,0.929289321881343));
#50499=CARTESIAN_POINT('',(41.,29.7,1.));
#50500=CARTESIAN_POINT('',(35.9375,29.8707106781187,0.929289321881342));
#50501=CARTESIAN_POINT('Origin',(41.,28.5,0.964644660940673));
#50502=CARTESIAN_POINT('',(42.3707106781187,28.5,0.929289321881346));
#50503=CARTESIAN_POINT('',(42.2,28.5,1.));
#50504=CARTESIAN_POINT('Origin',(41.,28.5,0.929289321881346));
#50505=CARTESIAN_POINT('Origin',(42.2853553390593,-7.5,0.964644660940672));
#50506=CARTESIAN_POINT('',(42.3707106781187,-28.5,0.929289321881343));
#50507=CARTESIAN_POINT('',(42.2,-28.5,1.));
#50508=CARTESIAN_POINT('',(42.3707106781187,-7.5,0.929289321881343));
#50509=CARTESIAN_POINT('Origin',(41.,-28.5,0.964644660940673));
#50510=CARTESIAN_POINT('',(41.,-29.8707106781187,0.929289321881346));
#50511=CARTESIAN_POINT('',(41.,-29.7,1.));
#50512=CARTESIAN_POINT('Origin',(41.,-28.5,0.929289321881346));
#50513=CARTESIAN_POINT('Origin',(31.5625,-29.7853553390593,0.964644660940671));
#50514=CARTESIAN_POINT('',(30.8,-29.8707106781187,0.929289321881342));
#50515=CARTESIAN_POINT('',(30.8,-21.9300622355798,4.21841360081793));
#50516=CARTESIAN_POINT('',(31.5625,-29.8707106781187,0.929289321881342));
#50517=CARTESIAN_POINT('Origin',(39.5,25.5,0.95));
#50518=CARTESIAN_POINT('',(38.55,25.5,0.95));
#50519=CARTESIAN_POINT('Origin',(39.5,-25.5,0.95));
#50520=CARTESIAN_POINT('',(38.55,-25.5,0.95));
#50521=CARTESIAN_POINT('Origin',(30.,-4.8,30.));
#50522=CARTESIAN_POINT('',(30.,-30.,1.));
#50523=CARTESIAN_POINT('Origin',(30.,-30.,1.));
#50524=CARTESIAN_POINT('',(30.8,-29.8,1.));
#50525=CARTESIAN_POINT('',(29.375,-29.8,1.));
#50526=CARTESIAN_POINT('',(30.8,-24.,1.));
#50527=CARTESIAN_POINT('Origin',(30.8,-17.4,15.5));
#50528=CARTESIAN_POINT('',(30.8,-23.125,7.67500000000001));
#50529=CARTESIAN_POINT('Origin',(26.5,-28.5,0.9));
#50530=CARTESIAN_POINT('',(25.2,-28.5,1.));
#50531=CARTESIAN_POINT('',(26.5,-30.,0.8));
#50532=CARTESIAN_POINT('Origin',(25.1,15.,0.9));
#50533=CARTESIAN_POINT('',(25.2,28.5,1.));
#50534=CARTESIAN_POINT('Origin',(26.5,28.5,0.9));
#50535=CARTESIAN_POINT('',(26.5,29.8,1.));
#50536=CARTESIAN_POINT('Origin',(38.125,29.9,0.9));
#50537=CARTESIAN_POINT('',(41.,29.8,1.));
#50538=CARTESIAN_POINT('Origin',(41.,28.5,0.9));
#50539=CARTESIAN_POINT('',(42.5,28.5,0.8));
#50540=CARTESIAN_POINT('',(42.3,28.5,1.));
#50541=CARTESIAN_POINT('Origin',(41.,28.5,0.8));
#50542=CARTESIAN_POINT('Origin',(42.4,-15.,0.9));
#50543=CARTESIAN_POINT('',(42.5,-28.5,0.8));
#50544=CARTESIAN_POINT('',(42.3,-28.5,1.));
#50545=CARTESIAN_POINT('',(42.5,-15.,0.8));
#50546=CARTESIAN_POINT('Origin',(41.,-28.5,0.9));
#50547=CARTESIAN_POINT('',(41.,-30.,0.8));
#50548=CARTESIAN_POINT('',(41.,-29.8,1.));
#50549=CARTESIAN_POINT('Origin',(41.,-28.5,0.8));
#50550=CARTESIAN_POINT('Origin',(29.375,-29.9,0.9));
#50551=CARTESIAN_POINT('',(29.375,-30.,0.8));
#50552=CARTESIAN_POINT('Origin',(42.5,-30.,0.));
#50553=CARTESIAN_POINT('',(42.5,28.5,0.));
#50554=CARTESIAN_POINT('',(42.5,-28.5,0.));
#50555=CARTESIAN_POINT('Origin',(41.,-28.5,0.));
#50556=CARTESIAN_POINT('',(41.,-30.,0.));
#50557=CARTESIAN_POINT('Origin',(25.,-30.,0.));
#50558=CARTESIAN_POINT('Origin',(41.,28.5,0.));
#50559=CARTESIAN_POINT('',(0.,0.,0.));
#50560=CARTESIAN_POINT('Origin',(18.5,0.,112.2));
#50561=CARTESIAN_POINT('',(18.5,-1.3471114790621E-16,111.1));
#50562=CARTESIAN_POINT('Origin',(18.5,-1.59204083889157E-16,110.9));
#50563=CARTESIAN_POINT('Origin',(18.5,0.,112.2));
#50564=CARTESIAN_POINT('',(18.4890127645178,1.40327133104537,112.729078050442));
#50565=CARTESIAN_POINT('',(18.319456010528,1.28858936270501,112.710548943691));
#50566=CARTESIAN_POINT('Ctrl Pts',(18.4890127645179,1.40327133104537,112.729078050442));
#50567=CARTESIAN_POINT('Ctrl Pts',(18.4690263934393,1.40191965211474,112.729546131244));
#50568=CARTESIAN_POINT('Ctrl Pts',(18.4493212209946,1.39790528142896,112.728584539615));
#50569=CARTESIAN_POINT('Ctrl Pts',(18.4209570524527,1.38778681836775,112.725655461841));
#50570=CARTESIAN_POINT('Ctrl Pts',(18.4116376687533,1.38366754929998,112.724420014907));
#50571=CARTESIAN_POINT('Ctrl Pts',(18.3896234532527,1.37182981375427,112.721060426925));
#50572=CARTESIAN_POINT('Ctrl Pts',(18.3774391567708,1.36337398597481,112.718799423342));
#50573=CARTESIAN_POINT('Ctrl Pts',(18.3498687355444,1.33884907188722,112.713621176115));
#50574=CARTESIAN_POINT('Ctrl Pts',(18.336256526853,1.32144069956727,112.710998260207));
#50575=CARTESIAN_POINT('Ctrl Pts',(18.3235239190592,1.29743221003086,112.710422570251));
#50576=CARTESIAN_POINT('Ctrl Pts',(18.3214048000438,1.29303642396641,112.710425791665));
#50577=CARTESIAN_POINT('Ctrl Pts',(18.3194560105972,1.28858936267476,112.710548943694));
#50578=CARTESIAN_POINT('',(18.5113942828676,1.21414296988455,113.080274071063));
#50579=CARTESIAN_POINT('Ctrl Pts',(18.5113942828676,1.21414296988456,113.080274071063));
#50580=CARTESIAN_POINT('Ctrl Pts',(18.5088122202491,1.24297666449313,113.040755400683));
#50581=CARTESIAN_POINT('Ctrl Pts',(18.5062148178964,1.26920627329322,113.000607351763));
#50582=CARTESIAN_POINT('Ctrl Pts',(18.4991940978944,1.33379276118183,112.891190706973));
#50583=CARTESIAN_POINT('Ctrl Pts',(18.4941783520461,1.37233329581525,112.811940460321));
#50584=CARTESIAN_POINT('Ctrl Pts',(18.4890127645178,1.40327133104537,112.729078050442));
#50585=CARTESIAN_POINT('Ctrl Pts',(18.3194560105972,1.28858936267476,112.710548943694));
#50586=CARTESIAN_POINT('Ctrl Pts',(18.3125847874797,1.27290950028387,112.710983164576));
#50587=CARTESIAN_POINT('Ctrl Pts',(18.3078358917878,1.25658996219521,112.712903987457));
#50588=CARTESIAN_POINT('Ctrl Pts',(18.3004473473152,1.21660861827732,112.722513325201));
#50589=CARTESIAN_POINT('Ctrl Pts',(18.2997088045305,1.19414451241967,112.731937704259));
#50590=CARTESIAN_POINT('Ctrl Pts',(18.3004369338146,1.15445099754945,112.757978862924));
#50591=CARTESIAN_POINT('Ctrl Pts',(18.3017489050252,1.13676465318605,112.774251060074));
#50592=CARTESIAN_POINT('Ctrl Pts',(18.302877988022,1.10764815299686,112.813536422119));
#50593=CARTESIAN_POINT('Ctrl Pts',(18.3026076034137,1.09682243884728,112.835175108492));
#50594=CARTESIAN_POINT('Ctrl Pts',(18.3011018541119,1.08399515770366,112.877971837947));
#50595=CARTESIAN_POINT('Ctrl Pts',(18.3000617770382,1.08107707365306,112.8987227829));
#50596=CARTESIAN_POINT('Ctrl Pts',(18.2999496538779,1.08205742545304,112.937854988679));
#50597=CARTESIAN_POINT('Ctrl Pts',(18.3007063184796,1.08525286840353,112.955989495));
#50598=CARTESIAN_POINT('Ctrl Pts',(18.3061260446686,1.096731305641,112.989071009869));
#50599=CARTESIAN_POINT('Ctrl Pts',(18.3103918083809,1.10435368484628,113.003441617128));
#50600=CARTESIAN_POINT('Ctrl Pts',(18.3243235188135,1.12376946338441,113.030471066797));
#50601=CARTESIAN_POINT('Ctrl Pts',(18.3341715042768,1.13533680110265,113.041892724703));
#50602=CARTESIAN_POINT('Ctrl Pts',(18.3597300671205,1.15942054077883,113.060869791061));
#50603=CARTESIAN_POINT('Ctrl Pts',(18.3754928067062,1.17154637795889,113.06771640348));
#50604=CARTESIAN_POINT('Ctrl Pts',(18.4086123435342,1.19100145104539,113.076651626788));
#50605=CARTESIAN_POINT('Ctrl Pts',(18.42545279698,1.1986529463623,113.079161175487));
#50606=CARTESIAN_POINT('Ctrl Pts',(18.456006836579,1.20821075735755,113.081440251631));
#50607=CARTESIAN_POINT('Ctrl Pts',(18.4692450945303,1.21109268178609,113.081759893621));
#50608=CARTESIAN_POINT('Ctrl Pts',(18.4885594461377,1.21339556016075,113.081448360779));
#50609=CARTESIAN_POINT('Ctrl Pts',(18.4944680194924,1.21385046309689,113.081249263501));
#50610=CARTESIAN_POINT('Ctrl Pts',(18.5013683698457,1.2140880273455,113.080899240207));
#50611=CARTESIAN_POINT('Ctrl Pts',(18.5023515795956,1.21411493937423,113.080846578183));
#50612=CARTESIAN_POINT('Ctrl Pts',(18.5036186445213,1.21414067372742,113.080775120454));
#50613=CARTESIAN_POINT('Ctrl Pts',(18.5039024894183,1.21414586005045,113.080758880334));
#50614=CARTESIAN_POINT('Ctrl Pts',(18.5043601203964,1.21415328867356,113.080732322449));
#50615=CARTESIAN_POINT('Ctrl Pts',(18.5045339082962,1.21415589277799,113.080722149835));
#50616=CARTESIAN_POINT('Ctrl Pts',(18.5048650036164,1.21416044065514,113.080702603299));
#50617=CARTESIAN_POINT('Ctrl Pts',(18.5050223111988,1.2141624236228,113.080693245104));
#50618=CARTESIAN_POINT('Ctrl Pts',(18.5053777240491,1.21416650212218,113.080671940352));
#50619=CARTESIAN_POINT('Ctrl Pts',(18.5055758277641,1.21416849343679,113.080659952045));
#50620=CARTESIAN_POINT('Ctrl Pts',(18.506090684748,1.21417293573454,113.080628500922));
#50621=CARTESIAN_POINT('Ctrl Pts',(18.5064074300013,1.21417494759492,113.080608862259));
#50622=CARTESIAN_POINT('Ctrl Pts',(18.508281420334,1.21418258364059,113.080490957723));
#50623=CARTESIAN_POINT('Ctrl Pts',(18.5098382130404,1.21417149237957,113.080386007052));
#50624=CARTESIAN_POINT('Ctrl Pts',(18.5113942828676,1.21414296988457,113.080274071063));
#50625=CARTESIAN_POINT('',(18.4283983699428,-1.10353994944975,113.19629633455));
#50626=CARTESIAN_POINT('Ctrl Pts',(18.4283983699428,-1.10353994944975,113.19629633455));
#50627=CARTESIAN_POINT('Ctrl Pts',(18.4105198342568,-1.10089569222145,113.188995676694));
#50628=CARTESIAN_POINT('Ctrl Pts',(18.3941523472385,-1.0974343046632,113.178993223828));
#50629=CARTESIAN_POINT('Ctrl Pts',(18.3704482929768,-1.0926857775768,113.157487700559));
#50630=CARTESIAN_POINT('Ctrl Pts',(18.3621213729005,-1.09112416856474,113.147761481668));
#50631=CARTESIAN_POINT('Ctrl Pts',(18.3449405301417,-1.08954139537506,113.121843290511));
#50632=CARTESIAN_POINT('Ctrl Pts',(18.3377217530226,-1.09048349674533,113.105395217439));
#50633=CARTESIAN_POINT('Ctrl Pts',(18.3272950132282,-1.09831932583815,113.070458177645));
#50634=CARTESIAN_POINT('Ctrl Pts',(18.3245022186406,-1.105373859452,113.052740657108));
#50635=CARTESIAN_POINT('Ctrl Pts',(18.3225000351569,-1.12537512884119,113.019809315101));
#50636=CARTESIAN_POINT('Ctrl Pts',(18.3233523412292,-1.13826827821126,113.004880872036));
#50637=CARTESIAN_POINT('Ctrl Pts',(18.3289022498025,-1.16639544953706,112.981146943516));
#50638=CARTESIAN_POINT('Ctrl Pts',(18.3332624135526,-1.18111489654657,112.972087482887));
#50639=CARTESIAN_POINT('Ctrl Pts',(18.3462969200968,-1.21017577871147,112.95892257907));
#50640=CARTESIAN_POINT('Ctrl Pts',(18.354504490354,-1.22399099626671,112.954742637065));
#50641=CARTESIAN_POINT('Ctrl Pts',(18.3751075959529,-1.24919519347668,112.949602689716));
#50642=CARTESIAN_POINT('Ctrl Pts',(18.3870279922863,-1.26018142477218,112.948629677876));
#50643=CARTESIAN_POINT('Ctrl Pts',(18.4129303458512,-1.27763043969617,112.948272440024));
#50644=CARTESIAN_POINT('Ctrl Pts',(18.4264110510245,-1.28422160833404,112.948763783935));
#50645=CARTESIAN_POINT('Ctrl Pts',(18.4512911255684,-1.29245398632846,112.949998556834));
#50646=CARTESIAN_POINT('Ctrl Pts',(18.4623104342892,-1.29489482010847,112.950651159398));
#50647=CARTESIAN_POINT('Ctrl Pts',(18.4780470056916,-1.29677491735672,112.951605478321));
#50648=CARTESIAN_POINT('Ctrl Pts',(18.4826341413343,-1.29713514230962,112.9518872744));
#50649=CARTESIAN_POINT('Ctrl Pts',(18.4880284340617,-1.29734074235437,112.952220771697));
#50650=CARTESIAN_POINT('Ctrl Pts',(18.488827627531,-1.2973655996001,112.952270241262));
#50651=CARTESIAN_POINT('Ctrl Pts',(18.4898693403749,-1.29739070377487,112.952334798159));
#50652=CARTESIAN_POINT('Ctrl Pts',(18.4901116962636,-1.29739602991256,112.952349822748));
#50653=CARTESIAN_POINT('Ctrl Pts',(18.4905041039374,-1.29740382086684,112.952374158247));
#50654=CARTESIAN_POINT('Ctrl Pts',(18.4906541429139,-1.29740660272727,112.952383465081));
#50655=CARTESIAN_POINT('Ctrl Pts',(18.4909280661229,-1.2974113217336,112.952400460104));
#50656=CARTESIAN_POINT('Ctrl Pts',(18.4910519467619,-1.29741332159137,112.952408147421));
#50657=CARTESIAN_POINT('Ctrl Pts',(18.4913236721632,-1.29741741357458,112.952425012176));
#50658=CARTESIAN_POINT('Ctrl Pts',(18.4914715201352,-1.29741944881729,112.952434190402));
#50659=CARTESIAN_POINT('Ctrl Pts',(18.4918604345446,-1.2974242994241,112.952458338957));
#50660=CARTESIAN_POINT('Ctrl Pts',(18.4921015111322,-1.29742679784955,112.952473313199));
#50661=CARTESIAN_POINT('Ctrl Pts',(18.4932714054423,-1.29743645539092,112.952546005746));
#50662=CARTESIAN_POINT('Ctrl Pts',(18.4942003175021,-1.29743657969559,112.952603802859));
#50663=CARTESIAN_POINT('Ctrl Pts',(18.5075944890952,-1.29732965474523,112.953438376998));
#50664=CARTESIAN_POINT('Ctrl Pts',(18.5200262878613,-1.29587261084622,112.954217675423));
#50665=CARTESIAN_POINT('Ctrl Pts',(18.5512344998855,-1.28871955431818,112.956380272165));
#50666=CARTESIAN_POINT('Ctrl Pts',(18.5693512045022,-1.28113646088861,112.957809120227));
#50667=CARTESIAN_POINT('Ctrl Pts',(18.6029398590356,-1.25971666804792,112.96256925626));
#50668=CARTESIAN_POINT('Ctrl Pts',(18.6176809713591,-1.24594235305202,112.965938249525));
#50669=CARTESIAN_POINT('Ctrl Pts',(18.6422007479794,-1.21409417011734,112.977393937126));
#50670=CARTESIAN_POINT('Ctrl Pts',(18.6512073945201,-1.19667462941293,112.985433472284));
#50671=CARTESIAN_POINT('Ctrl Pts',(18.6635070263108,-1.16275079443269,113.007644142204));
#50672=CARTESIAN_POINT('Ctrl Pts',(18.6667151219446,-1.14676806040784,113.021491299409));
#50673=CARTESIAN_POINT('Ctrl Pts',(18.6681181165073,-1.12186304344204,113.05156803892));
#50674=CARTESIAN_POINT('Ctrl Pts',(18.6669824740447,-1.11233764280274,113.067026820135));
#50675=CARTESIAN_POINT('Ctrl Pts',(18.6608198607348,-1.0995005522286,113.097149717965));
#50676=CARTESIAN_POINT('Ctrl Pts',(18.6563998349178,-1.09560335823169,113.111344641313));
#50677=CARTESIAN_POINT('Ctrl Pts',(18.6435144213581,-1.09173897964326,113.138488335518));
#50678=CARTESIAN_POINT('Ctrl Pts',(18.6354331643911,-1.09172221268073,113.150854236727));
#50679=CARTESIAN_POINT('Ctrl Pts',(18.6166910806198,-1.09379506873728,113.171324492591));
#50680=CARTESIAN_POINT('Ctrl Pts',(18.6068447744918,-1.09554575910708,113.179430674276));
#50681=CARTESIAN_POINT('Ctrl Pts',(18.5825339836664,-1.09986755155098,113.194519964973));
#50682=CARTESIAN_POINT('Ctrl Pts',(18.5678269514339,-1.10245959900021,113.200594508659));
#50683=CARTESIAN_POINT('Ctrl Pts',(18.5399706841515,-1.10605222763602,113.20788137288));
#50684=CARTESIAN_POINT('Ctrl Pts',(18.5271604037061,-1.10726480039516,113.209790754062));
#50685=CARTESIAN_POINT('Ctrl Pts',(18.5080211320997,-1.10820521807391,113.210786846784));
#50686=CARTESIAN_POINT('Ctrl Pts',(18.5017820858503,-1.10837943502796,113.210822647527));
#50687=CARTESIAN_POINT('Ctrl Pts',(18.4945234270871,-1.1084222163849,113.210536072413));
#50688=CARTESIAN_POINT('Ctrl Pts',(18.4934948042869,-1.10842454994123,113.210487758034));
#50689=CARTESIAN_POINT('Ctrl Pts',(18.4921729528856,-1.10842274722134,113.210415775184));
#50690=CARTESIAN_POINT('Ctrl Pts',(18.4918793902317,-1.10842204234513,113.210399161215));
#50691=CARTESIAN_POINT('Ctrl Pts',(18.4914080950982,-1.10842042156096,113.210371480633));
#50692=CARTESIAN_POINT('Ctrl Pts',(18.491230346989,-1.10841969856969,113.210360810743));
#50693=CARTESIAN_POINT('Ctrl Pts',(18.4908911653357,-1.10841810568575,113.210340010881));
#50694=CARTESIAN_POINT('Ctrl Pts',(18.4907297304023,-1.10841725535653,113.210329921146));
#50695=CARTESIAN_POINT('Ctrl Pts',(18.4903662148411,-1.10841513294104,113.210306773437));
#50696=CARTESIAN_POINT('Ctrl Pts',(18.4901641385227,-1.1084138085915,113.210293608004));
#50697=CARTESIAN_POINT('Ctrl Pts',(18.4896414017413,-1.10841000877977,113.210258780781));
#50698=CARTESIAN_POINT('Ctrl Pts',(18.489320764701,-1.10840731400558,113.210236668325));
#50699=CARTESIAN_POINT('Ctrl Pts',(18.4874654483094,-1.10838961412012,113.210104375723));
#50700=CARTESIAN_POINT('Ctrl Pts',(18.4859319332317,-1.10836663760827,113.20997783395));
#50701=CARTESIAN_POINT('Ctrl Pts',(18.4650966690796,-1.10794123351876,113.208024364095));
#50702=CARTESIAN_POINT('Ctrl Pts',(18.4461433726562,-1.10616445698858,113.203542464532));
#50703=CARTESIAN_POINT('Ctrl Pts',(18.4283983699427,-1.10353994944975,113.19629633455));
#50704=CARTESIAN_POINT('',(18.3123644474208,1.23076923076922,111.6));
#50705=CARTESIAN_POINT('',(18.3,1.3,112.2));
#50706=CARTESIAN_POINT('Ctrl Pts',(18.3123644474208,1.23076923076924,111.6));
#50707=CARTESIAN_POINT('Ctrl Pts',(18.2984337402964,1.26852550530057,111.763610522969));
#50708=CARTESIAN_POINT('Ctrl Pts',(18.3000000038754,1.29968079467276,111.965095195088));
#50709=CARTESIAN_POINT('Ctrl Pts',(18.299999999995,1.29999918730283,112.197626492492));
#50710=CARTESIAN_POINT('Ctrl Pts',(18.3,1.3,112.198813368143));
#50711=CARTESIAN_POINT('Ctrl Pts',(18.3,1.3,112.2));
#50712=CARTESIAN_POINT('',(18.6876355525792,1.23076923076922,111.6));
#50713=CARTESIAN_POINT('Ctrl Pts',(18.6876355525792,1.23076923076922,111.6));
#50714=CARTESIAN_POINT('Ctrl Pts',(18.6863212589794,1.23473208763278,111.6));
#50715=CARTESIAN_POINT('Ctrl Pts',(18.6849243200251,1.23859136984675,111.6));
#50716=CARTESIAN_POINT('Ctrl Pts',(18.6737631989001,1.26715167689378,111.6));
#50717=CARTESIAN_POINT('Ctrl Pts',(18.6568893055075,1.29433425576249,111.6));
#50718=CARTESIAN_POINT('Ctrl Pts',(18.6213508157909,1.3318682066872,111.6));
#50719=CARTESIAN_POINT('Ctrl Pts',(18.5969013940152,1.3493098388476,111.6));
#50720=CARTESIAN_POINT('Ctrl Pts',(18.5520128528442,1.3688365799757,111.6));
#50721=CARTESIAN_POINT('Ctrl Pts',(18.5239242084953,1.37477270848677,111.6));
#50722=CARTESIAN_POINT('Ctrl Pts',(18.5,1.37477270848677,111.6));
#50723=CARTESIAN_POINT('Ctrl Pts',(18.4760757915047,1.37477270848677,111.6));
#50724=CARTESIAN_POINT('Ctrl Pts',(18.4479871471558,1.3688365799757,111.6));
#50725=CARTESIAN_POINT('Ctrl Pts',(18.4030986059848,1.3493098388476,111.6));
#50726=CARTESIAN_POINT('Ctrl Pts',(18.3786491842091,1.3318682066872,111.6));
#50727=CARTESIAN_POINT('Ctrl Pts',(18.3431106944925,1.29433425576249,111.6));
#50728=CARTESIAN_POINT('Ctrl Pts',(18.3262368010999,1.26715167689378,111.6));
#50729=CARTESIAN_POINT('Ctrl Pts',(18.3150756799749,1.23859136984675,111.6));
#50730=CARTESIAN_POINT('Ctrl Pts',(18.3136787410206,1.23473208763278,111.6));
#50731=CARTESIAN_POINT('Ctrl Pts',(18.3123644474208,1.23076923076922,111.6));
#50732=CARTESIAN_POINT('',(18.7,1.3,112.2));
#50733=CARTESIAN_POINT('Ctrl Pts',(18.7,1.3,112.2));
#50734=CARTESIAN_POINT('Ctrl Pts',(18.7,1.3,112.198813368143));
#50735=CARTESIAN_POINT('Ctrl Pts',(18.700000000005,1.29999918730283,112.197626492492));
#50736=CARTESIAN_POINT('Ctrl Pts',(18.6999999961246,1.29968079467278,111.965095195094));
#50737=CARTESIAN_POINT('Ctrl Pts',(18.7015662597039,1.26852550530162,111.763610522974));
#50738=CARTESIAN_POINT('Ctrl Pts',(18.6876355525792,1.23076923076923,111.6));
#50739=CARTESIAN_POINT('',(18.6999907542242,1.29807692307696,112.3));
#50740=CARTESIAN_POINT('Ctrl Pts',(18.6999907542242,1.29807692307696,112.3));
#50741=CARTESIAN_POINT('Ctrl Pts',(18.7000026383082,1.29931281067831,112.267866922365));
#50742=CARTESIAN_POINT('Ctrl Pts',(18.6999999994485,1.29995353020451,112.235718199897));
#50743=CARTESIAN_POINT('Ctrl Pts',(18.700000000005,1.29999918730283,112.202373507508));
#50744=CARTESIAN_POINT('Ctrl Pts',(18.7,1.3,112.201186631857));
#50745=CARTESIAN_POINT('Ctrl Pts',(18.7,1.3,112.2));
#50746=CARTESIAN_POINT('',(18.3000092457758,1.29807692307696,112.3));
#50747=CARTESIAN_POINT('Ctrl Pts',(18.3000092457758,1.29807692307696,112.3));
#50748=CARTESIAN_POINT('Ctrl Pts',(18.3002426875627,1.32242567789215,112.3));
#50749=CARTESIAN_POINT('Ctrl Pts',(18.3060316768999,1.35067447040255,112.3));
#50750=CARTESIAN_POINT('Ctrl Pts',(18.3247081897855,1.39582998875735,112.3));
#50751=CARTESIAN_POINT('Ctrl Pts',(18.3411747406685,1.42052008010624,112.3));
#50752=CARTESIAN_POINT('Ctrl Pts',(18.3760974271551,1.45549178160028,112.3));
#50753=CARTESIAN_POINT('Ctrl Pts',(18.4007210413769,1.47197246341128,112.3));
#50754=CARTESIAN_POINT('Ctrl Pts',(18.4463107520171,1.49088031549837,112.3));
#50755=CARTESIAN_POINT('Ctrl Pts',(18.4753365162084,1.49666295470959,112.3));
#50756=CARTESIAN_POINT('Ctrl Pts',(18.5,1.49666295470959,112.3));
#50757=CARTESIAN_POINT('Ctrl Pts',(18.5246634837916,1.49666295470959,112.3));
#50758=CARTESIAN_POINT('Ctrl Pts',(18.5536892479829,1.49088031549837,112.3));
#50759=CARTESIAN_POINT('Ctrl Pts',(18.5992789586231,1.47197246341128,112.3));
#50760=CARTESIAN_POINT('Ctrl Pts',(18.6239025728449,1.45549178160028,112.3));
#50761=CARTESIAN_POINT('Ctrl Pts',(18.6588252593315,1.42052008010624,112.3));
#50762=CARTESIAN_POINT('Ctrl Pts',(18.6752918102145,1.39582998875735,112.3));
#50763=CARTESIAN_POINT('Ctrl Pts',(18.6939683231001,1.35067447040255,112.3));
#50764=CARTESIAN_POINT('Ctrl Pts',(18.6997573124373,1.32242567789215,112.3));
#50765=CARTESIAN_POINT('Ctrl Pts',(18.6999907542242,1.29807692307696,112.3));
#50766=CARTESIAN_POINT('Ctrl Pts',(18.3,1.3,112.2));
#50767=CARTESIAN_POINT('Ctrl Pts',(18.3,1.3,112.201186631857));
#50768=CARTESIAN_POINT('Ctrl Pts',(18.299999999995,1.29999918730283,112.202373507508));
#50769=CARTESIAN_POINT('Ctrl Pts',(18.3000000005515,1.29995353020451,112.235718199897));
#50770=CARTESIAN_POINT('Ctrl Pts',(18.2999973616918,1.2993128106783,112.267866922365));
#50771=CARTESIAN_POINT('Ctrl Pts',(18.3000092457758,1.29807692307696,112.3));
#50772=CARTESIAN_POINT('Origin',(18.5,1.3,112.3));
#50773=CARTESIAN_POINT('Origin',(18.5,1.3,112.3));
#50774=CARTESIAN_POINT('Origin',(18.5,1.3,111.6));
#50775=CARTESIAN_POINT('Origin',(18.5,1.3,111.6));
#50776=CARTESIAN_POINT('Origin',(18.5,1.3,111.6));
#50777=CARTESIAN_POINT('Origin',(18.5,1.3,112.9));
#50778=CARTESIAN_POINT('Origin',(18.5,1.3,112.9));
#50779=CARTESIAN_POINT('Origin',(18.5,0.,128.8));
#50780=CARTESIAN_POINT('',(18.5,-1.34711147906207E-16,127.7));
#50781=CARTESIAN_POINT('Origin',(18.5,-1.59204083889153E-16,127.5));
#50782=CARTESIAN_POINT('Origin',(18.5,0.,128.8));
#50783=CARTESIAN_POINT('',(18.7,1.3,128.8));
#50784=CARTESIAN_POINT('',(18.3,1.3,128.8));
#50785=CARTESIAN_POINT('Origin',(18.5,1.3,128.8));
#50786=CARTESIAN_POINT('',(18.3235897901759,1.20576923076922,128.1));
#50787=CARTESIAN_POINT('Ctrl Pts',(18.3235897901759,1.20576923076922,128.1));
#50788=CARTESIAN_POINT('Ctrl Pts',(18.2973822762268,1.25483253644383,128.282235135363));
#50789=CARTESIAN_POINT('Ctrl Pts',(18.3000000041203,1.29963250090516,128.518892224432));
#50790=CARTESIAN_POINT('Ctrl Pts',(18.2999999999958,1.29999925015416,128.797720020479));
#50791=CARTESIAN_POINT('Ctrl Pts',(18.3,1.3,128.798860078224));
#50792=CARTESIAN_POINT('Ctrl Pts',(18.3,1.3,128.8));
#50793=CARTESIAN_POINT('',(18.5002243000221,1.32664977393096,128.1));
#50794=CARTESIAN_POINT('Ctrl Pts',(18.5002243000221,1.32664977393096,128.1));
#50795=CARTESIAN_POINT('Ctrl Pts',(18.5001494926749,1.32664986879001,128.1));
#50796=CARTESIAN_POINT('Ctrl Pts',(18.5000747258889,1.32664991614213,128.1));
#50797=CARTESIAN_POINT('Ctrl Pts',(18.5,1.32664991614213,128.1));
#50798=CARTESIAN_POINT('Ctrl Pts',(18.4763894791635,1.32664991614213,128.1));
#50799=CARTESIAN_POINT('Ctrl Pts',(18.4486985736677,1.32065396814081,128.1));
#50800=CARTESIAN_POINT('Ctrl Pts',(18.4041135913171,1.30087556631979,128.1));
#50801=CARTESIAN_POINT('Ctrl Pts',(18.3797528378326,1.28303070674698,128.1));
#50802=CARTESIAN_POINT('Ctrl Pts',(18.3476245045884,1.24833850134275,128.1));
#50803=CARTESIAN_POINT('Ctrl Pts',(18.3333992207159,1.22700388737273,128.1));
#50804=CARTESIAN_POINT('Ctrl Pts',(18.3235897901759,1.20576923076922,128.1));
#50805=CARTESIAN_POINT('',(18.4886057170625,1.21414296988327,127.919725928942));
#50806=CARTESIAN_POINT('Ctrl Pts',(18.4886057170625,1.21414296988326,127.919725928942));
#50807=CARTESIAN_POINT('Ctrl Pts',(18.4911877797212,1.24297666476934,127.9592445997));
#50808=CARTESIAN_POINT('Ctrl Pts',(18.4937851821151,1.26920627380217,127.999392649018));
#50809=CARTESIAN_POINT('Ctrl Pts',(18.4975804224297,1.30412024852119,128.058540778958));
#50810=CARTESIAN_POINT('Ctrl Pts',(18.4988856330623,1.31555196810735,128.078964066341));
#50811=CARTESIAN_POINT('Ctrl Pts',(18.5002243000221,1.32664977393097,128.1));
#50812=CARTESIAN_POINT('',(18.6702841632836,1.12955615107723,127.964633341575));
#50813=CARTESIAN_POINT('Ctrl Pts',(18.6702841630468,1.12955615106615,127.964633341765));
#50814=CARTESIAN_POINT('Ctrl Pts',(18.6653387332645,1.13522043042002,127.958790838693));
#50815=CARTESIAN_POINT('Ctrl Pts',(18.6597721606308,1.14104363370426,127.953610539743));
#50816=CARTESIAN_POINT('Ctrl Pts',(18.6402703998699,1.15942016474004,127.939130439405));
#50817=CARTESIAN_POINT('Ctrl Pts',(18.6245076173094,1.17154609064284,127.932283746225));
#50818=CARTESIAN_POINT('Ctrl Pts',(18.5913880187093,1.19100127211283,127.923348439596));
#50819=CARTESIAN_POINT('Ctrl Pts',(18.5745475659151,1.19865280082519,127.920838868829));
#50820=CARTESIAN_POINT('Ctrl Pts',(18.5439935651917,1.2082106549485,127.918559765759));
#50821=CARTESIAN_POINT('Ctrl Pts',(18.5307553501655,1.2110925974478,127.918240112273));
#50822=CARTESIAN_POINT('Ctrl Pts',(18.5114409726006,1.21339552395061,127.918551626728));
#50823=CARTESIAN_POINT('Ctrl Pts',(18.5055323311222,1.21385044304153,127.918750721917));
#50824=CARTESIAN_POINT('Ctrl Pts',(18.4986318935235,1.21408801960182,127.919100745897));
#50825=CARTESIAN_POINT('Ctrl Pts',(18.4976486652827,1.21411493333287,127.919153408432));
#50826=CARTESIAN_POINT('Ctrl Pts',(18.4963815755996,1.21414066956251,127.919224867006));
#50827=CARTESIAN_POINT('Ctrl Pts',(18.4960977244373,1.21414585629502,127.919241107366));
#50828=CARTESIAN_POINT('Ctrl Pts',(18.4956400831649,1.21415328554028,127.919267665666));
#50829=CARTESIAN_POINT('Ctrl Pts',(18.495466291215,1.21415588987324,127.91927783845));
#50830=CARTESIAN_POINT('Ctrl Pts',(18.4951351880664,1.21416043816795,127.919297385324));
#50831=CARTESIAN_POINT('Ctrl Pts',(18.4949778766776,1.21416242132666,127.919306743687));
#50832=CARTESIAN_POINT('Ctrl Pts',(18.4946224550266,1.2141665002405,127.919328048841));
#50833=CARTESIAN_POINT('Ctrl Pts',(18.4944243463601,1.21416849177246,127.919340037381));
#50834=CARTESIAN_POINT('Ctrl Pts',(18.4939094760844,1.21417293460233,127.919371489148));
#50835=CARTESIAN_POINT('Ctrl Pts',(18.4935927224993,1.21417494675346,127.919391128233));
#50836=CARTESIAN_POINT('Ctrl Pts',(18.4917186757302,1.21418258432441,127.9195090358));
#50837=CARTESIAN_POINT('Ctrl Pts',(18.490161834936,1.21417149325911,127.919613989496));
#50838=CARTESIAN_POINT('Ctrl Pts',(18.4886057170625,1.21414296988326,127.919725928942));
#50839=CARTESIAN_POINT('',(18.6933911448853,1.24901112788112,128.285080457724));
#50840=CARTESIAN_POINT('Ctrl Pts',(18.6933911448858,1.24901112788106,128.285080457724));
#50841=CARTESIAN_POINT('Ctrl Pts',(18.6941695295676,1.2455347549892,128.284393845319));
#50842=CARTESIAN_POINT('Ctrl Pts',(18.6948689918491,1.2420448951124,128.28362015538));
#50843=CARTESIAN_POINT('Ctrl Pts',(18.6991384438423,1.2181470596441,128.277703499066));
#50844=CARTESIAN_POINT('Ctrl Pts',(18.700090555879,1.19846217194705,128.269752590558));
#50845=CARTESIAN_POINT('Ctrl Pts',(18.6998883984898,1.16039199645397,128.246791255634));
#50846=CARTESIAN_POINT('Ctrl Pts',(18.6985769622911,1.14211768289233,128.231171889393));
#50847=CARTESIAN_POINT('Ctrl Pts',(18.6971943128989,1.1116295024956,128.1930989791));
#50848=CARTESIAN_POINT('Ctrl Pts',(18.6972376067016,1.10002920430251,128.171906869082));
#50849=CARTESIAN_POINT('Ctrl Pts',(18.6986757815866,1.08449168880853,128.12634150471));
#50850=CARTESIAN_POINT('Ctrl Pts',(18.6999332936667,1.08103423817092,128.102989944245));
#50851=CARTESIAN_POINT('Ctrl Pts',(18.7000503625628,1.08205735198823,128.062145569422));
#50852=CARTESIAN_POINT('Ctrl Pts',(18.6992937255094,1.08525274687609,128.044011007997));
#50853=CARTESIAN_POINT('Ctrl Pts',(18.69387406073,1.09673110860034,128.01092941677));
#50854=CARTESIAN_POINT('Ctrl Pts',(18.6896083372694,1.104353449732,127.996558781634));
#50855=CARTESIAN_POINT('Ctrl Pts',(18.6793930756325,1.11858988928783,127.976739577122));
#50856=CARTESIAN_POINT('Ctrl Pts',(18.6751379969018,1.12399678168825,127.97036763392));
#50857=CARTESIAN_POINT('Ctrl Pts',(18.6702841630468,1.12955615106615,127.964633341765));
#50858=CARTESIAN_POINT('Ctrl Pts',(18.7,1.3,128.8));
#50859=CARTESIAN_POINT('Ctrl Pts',(18.7,1.3,128.798860078224));
#50860=CARTESIAN_POINT('Ctrl Pts',(18.7000000000042,1.29999925015416,128.797720020479));
#50861=CARTESIAN_POINT('Ctrl Pts',(18.699999997155,1.29974590119044,128.605106856646));
#50862=CARTESIAN_POINT('Ctrl Pts',(18.7011229833964,1.27833652849495,128.433154157275));
#50863=CARTESIAN_POINT('Ctrl Pts',(18.6933911448853,1.24901112788118,128.285080457724));
#50864=CARTESIAN_POINT('',(18.3892924448916,-1.25128032625762,128.035075233373));
#50865=CARTESIAN_POINT('Ctrl Pts',(18.3892924448916,-1.25128032625762,128.035075233373));
#50866=CARTESIAN_POINT('Ctrl Pts',(18.3798994606449,-1.24247387220421,128.03263906063));
#50867=CARTESIAN_POINT('Ctrl Pts',(18.3716813533086,-1.23279082229575,128.029561362241));
#50868=CARTESIAN_POINT('Ctrl Pts',(18.3585843738093,-1.21376562057004,128.022036324831));
#50869=CARTESIAN_POINT('Ctrl Pts',(18.3534816661773,-1.2047112654056,128.017901894435));
#50870=CARTESIAN_POINT('Ctrl Pts',(18.3416272087126,-1.17934898870496,128.004113103988));
#50871=CARTESIAN_POINT('Ctrl Pts',(18.3368687162988,-1.1633410963693,127.99285169318));
#50872=CARTESIAN_POINT('Ctrl Pts',(18.3319858487178,-1.13523495824815,127.96592156058));
#50873=CARTESIAN_POINT('Ctrl Pts',(18.3316753585454,-1.12317339172176,127.950591366736));
#50874=CARTESIAN_POINT('Ctrl Pts',(18.3352116622682,-1.10601113755093,127.919878737263));
#50875=CARTESIAN_POINT('Ctrl Pts',(18.3384075916268,-1.10019403805833,127.905051434488));
#50876=CARTESIAN_POINT('Ctrl Pts',(18.3486564892805,-1.09329953675059,127.87665371864));
#50877=CARTESIAN_POINT('Ctrl Pts',(18.3552149615871,-1.09196650404974,127.86356771344));
#50878=CARTESIAN_POINT('Ctrl Pts',(18.3728912616988,-1.09222750541447,127.838810790113));
#50879=CARTESIAN_POINT('Ctrl Pts',(18.383771728885,-1.09393068606538,127.8279088649));
#50880=CARTESIAN_POINT('Ctrl Pts',(18.409424692351,-1.09840208445071,127.809605483562));
#50881=CARTESIAN_POINT('Ctrl Pts',(18.4238896729194,-1.10110524006805,127.802632548698));
#50882=CARTESIAN_POINT('Ctrl Pts',(18.4522867719007,-1.10518160358501,127.793659605297));
#50883=CARTESIAN_POINT('Ctrl Pts',(18.4658454196017,-1.10668775670786,127.791095337941));
#50884=CARTESIAN_POINT('Ctrl Pts',(18.4876523176408,-1.10806135716137,127.789283776043));
#50885=CARTESIAN_POINT('Ctrl Pts',(18.4957622801494,-1.10835349387855,127.789104107661));
#50886=CARTESIAN_POINT('Ctrl Pts',(18.5050575455568,-1.10842097725468,127.789444840517));
#50887=CARTESIAN_POINT('Ctrl Pts',(18.5062500731142,-1.10842463446296,127.789498891965));
#50888=CARTESIAN_POINT('Ctrl Pts',(18.5077522181175,-1.10842290541232,127.789580034198));
#50889=CARTESIAN_POINT('Ctrl Pts',(18.5080615324343,-1.10842221190459,127.78959743825));
#50890=CARTESIAN_POINT('Ctrl Pts',(18.50855223089,-1.10842057420063,127.789626155808));
#50891=CARTESIAN_POINT('Ctrl Pts',(18.5087335224116,-1.10841985313119,127.789637004744));
#50892=CARTESIAN_POINT('Ctrl Pts',(18.5090592733913,-1.10841834823437,127.789656929655));
#50893=CARTESIAN_POINT('Ctrl Pts',(18.5092037035598,-1.10841760733907,127.789665915658));
#50894=CARTESIAN_POINT('Ctrl Pts',(18.509514596913,-1.10841585336197,127.789685586428));
#50895=CARTESIAN_POINT('Ctrl Pts',(18.509681076526,-1.10841481622478,127.789696321608));
#50896=CARTESIAN_POINT('Ctrl Pts',(18.5101596687195,-1.10841155216991,127.789727764983));
#50897=CARTESIAN_POINT('Ctrl Pts',(18.510471882263,-1.10840907831999,127.789748987171));
#50898=CARTESIAN_POINT('Ctrl Pts',(18.5118942490537,-1.10839623268546,127.789848916666));
#50899=CARTESIAN_POINT('Ctrl Pts',(18.5130045279313,-1.10838184132914,127.789935912113));
#50900=CARTESIAN_POINT('Ctrl Pts',(18.5289010892121,-1.10811313058816,127.791310872672));
#50901=CARTESIAN_POINT('Ctrl Pts',(18.5435288883242,-1.10706679477448,127.794167098735));
#50902=CARTESIAN_POINT('Ctrl Pts',(18.5780645770096,-1.10298841376075,127.805135758393));
#50903=CARTESIAN_POINT('Ctrl Pts',(18.5963905684292,-1.09938262181171,127.814741468509));
#50904=CARTESIAN_POINT('Ctrl Pts',(18.6270867645603,-1.09315777119027,127.838998624416));
#50905=CARTESIAN_POINT('Ctrl Pts',(18.6395729240457,-1.09053042151983,127.853385617341));
#50906=CARTESIAN_POINT('Ctrl Pts',(18.6587003172132,-1.08984138593605,127.885720048849));
#50907=CARTESIAN_POINT('Ctrl Pts',(18.6651532160224,-1.09158743291629,127.90246539444));
#50908=CARTESIAN_POINT('Ctrl Pts',(18.6742126672308,-1.10122999609394,127.937592024301));
#50909=CARTESIAN_POINT('Ctrl Pts',(18.6764218952049,-1.10933821221676,127.95526698208));
#50910=CARTESIAN_POINT('Ctrl Pts',(18.6772210972485,-1.13106051535397,127.987174545981));
#50911=CARTESIAN_POINT('Ctrl Pts',(18.6758404085021,-1.14447798380644,128.001238995918));
#50912=CARTESIAN_POINT('Ctrl Pts',(18.6691623998671,-1.17314306545758,128.023265178206));
#50913=CARTESIAN_POINT('Ctrl Pts',(18.6642428497083,-1.18785848703717,128.031478436654));
#50914=CARTESIAN_POINT('Ctrl Pts',(18.6500295363492,-1.21660724198031,128.043222559086));
#50915=CARTESIAN_POINT('Ctrl Pts',(18.6412150739195,-1.23011383168726,128.046802507509));
#50916=CARTESIAN_POINT('Ctrl Pts',(18.6195527785074,-1.25435939432101,128.050987824865));
#50917=CARTESIAN_POINT('Ctrl Pts',(18.6071944358135,-1.26474856820655,128.051626762945));
#50918=CARTESIAN_POINT('Ctrl Pts',(18.5809477583168,-1.28077826412714,128.05155359561));
#50919=CARTESIAN_POINT('Ctrl Pts',(18.5675600416982,-1.28666191306148,128.050974310672));
#50920=CARTESIAN_POINT('Ctrl Pts',(18.5435683232137,-1.29363459637126,128.049701976543));
#50921=CARTESIAN_POINT('Ctrl Pts',(18.5333148146624,-1.29560082132902,128.049086890045));
#50922=CARTESIAN_POINT('Ctrl Pts',(18.5190012477797,-1.29700506719052,128.048213240759));
#50923=CARTESIAN_POINT('Ctrl Pts',(18.5150412649157,-1.29725470226466,128.047969337274));
#50924=CARTESIAN_POINT('Ctrl Pts',(18.5106959483058,-1.29737719199358,128.047700235014));
#50925=CARTESIAN_POINT('Ctrl Pts',(18.5103183510609,-1.29738658894726,128.047676837662));
#50926=CARTESIAN_POINT('Ctrl Pts',(18.5097606195382,-1.2973986209018,128.047642259385));
#50927=CARTESIAN_POINT('Ctrl Pts',(18.5095806912436,-1.29740221955525,128.047631101249));
#50928=CARTESIAN_POINT('Ctrl Pts',(18.5092748392951,-1.29740785409831,128.047612129049));
#50929=CARTESIAN_POINT('Ctrl Pts',(18.5091489697301,-1.29741003450508,128.047604319845));
#50930=CARTESIAN_POINT('Ctrl Pts',(18.5088930397262,-1.29741418546983,128.047588438508));
#50931=CARTESIAN_POINT('Ctrl Pts',(18.5087629747962,-1.29741614724726,128.047580366003));
#50932=CARTESIAN_POINT('Ctrl Pts',(18.5084551210459,-1.29742043962893,128.047561255371));
#50933=CARTESIAN_POINT('Ctrl Pts',(18.508277286455,-1.29742264299259,128.047550213079));
#50934=CARTESIAN_POINT('Ctrl Pts',(18.5076554909947,-1.2974293779868,128.047511593851));
#50935=CARTESIAN_POINT('Ctrl Pts',(18.5072112685641,-1.29743246690907,128.047483985686));
#50936=CARTESIAN_POINT('Ctrl Pts',(18.5021353719972,-1.29744801399593,128.047168313941));
#50937=CARTESIAN_POINT('Ctrl Pts',(18.4975003376624,-1.29727471082049,128.04687828474));
#50938=CARTESIAN_POINT('Ctrl Pts',(18.4722386482183,-1.29530419319829,128.045279066271));
#50939=CARTESIAN_POINT('Ctrl Pts',(18.4520327626891,-1.28998020248121,128.044002189889));
#50940=CARTESIAN_POINT('Ctrl Pts',(18.4170565203638,-1.27354147714406,128.040503340081));
#50941=CARTESIAN_POINT('Ctrl Pts',(18.4022413006459,-1.2634206109904,128.038433660112));
#50942=CARTESIAN_POINT('Ctrl Pts',(18.3892924448916,-1.25128032625768,128.035075233373));
#50943=CARTESIAN_POINT('Origin',(18.5,1.30000000000003,128.1));
#50944=CARTESIAN_POINT('',(18.5016832568904,1.49999291649016,128.1));
#50945=CARTESIAN_POINT('',(18.5,1.30000000000001,128.1));
#50946=CARTESIAN_POINT('Origin',(18.5,1.30000000000003,128.1));
#50947=CARTESIAN_POINT('Origin',(18.5,1.3,128.1));
#50948=CARTESIAN_POINT('Origin',(18.5,1.3,128.1));
#50949=CARTESIAN_POINT('Origin',(18.5,1.3,128.1));
#50950=CARTESIAN_POINT('Ctrl Pts',(18.5016832568899,1.49999291649016,128.1));
#50951=CARTESIAN_POINT('Ctrl Pts',(18.5019060534612,1.49999104130443,128.100197947578));
#50952=CARTESIAN_POINT('Ctrl Pts',(18.5021288480507,1.49998879380848,128.100395894012));
#50953=CARTESIAN_POINT('Ctrl Pts',(18.5332913213164,1.49962235392642,128.128082945286));
#50954=CARTESIAN_POINT('Ctrl Pts',(18.5643676714885,1.49207596231939,128.155707919539));
#50955=CARTESIAN_POINT('Ctrl Pts',(18.6158401718151,1.46508561658941,128.202366702973));
#50956=CARTESIAN_POINT('Ctrl Pts',(18.6373473722111,1.44811312339091,128.222225381534));
#50957=CARTESIAN_POINT('Ctrl Pts',(18.6687008379444,1.40953464131882,128.252332431214));
#50958=CARTESIAN_POINT('Ctrl Pts',(18.6801090859612,1.39004658705681,128.263746708316));
#50959=CARTESIAN_POINT('Ctrl Pts',(18.6945636658313,1.35009248507517,128.279386999448));
#50960=CARTESIAN_POINT('Ctrl Pts',(18.69864622317,1.33076612999911,128.284423898441));
#50961=CARTESIAN_POINT('Ctrl Pts',(18.7007458372437,1.29129390710522,128.289049365168));
#50962=CARTESIAN_POINT('Ctrl Pts',(18.6989593474376,1.27195776119289,128.288754201356));
#50963=CARTESIAN_POINT('Ctrl Pts',(18.6941136437467,1.25181280973272,128.285570187084));
#50964=CARTESIAN_POINT('Ctrl Pts',(18.6937594098627,1.25040788726464,128.285332422228));
#50965=CARTESIAN_POINT('Ctrl Pts',(18.6933911448853,1.24901112788109,128.285080457724));
#50966=CARTESIAN_POINT('Ctrl Pts',(18.488182152249,1.29990053410893,112.700349483895));
#50967=CARTESIAN_POINT('Ctrl Pts',(18.3444976430382,1.29869120157713,112.70885515658));
#50968=CARTESIAN_POINT('Ctrl Pts',(18.1626414086569,1.26954424100949,112.72020028386));
#50969=CARTESIAN_POINT('Ctrl Pts',(17.9105741471188,1.1715572059241,112.7372275449));
#50970=CARTESIAN_POINT('Ctrl Pts',(17.7147016928909,1.05680544825268,112.75142581384));
#50971=CARTESIAN_POINT('Ctrl Pts',(17.5092914781924,0.870936460786282,112.768496063499));
#50972=CARTESIAN_POINT('Ctrl Pts',(17.3452643787265,0.645338607702756,112.785608543142));
#50973=CARTESIAN_POINT('Ctrl Pts',(17.1949694671818,0.305633664533222,112.808486356608));
#50974=CARTESIAN_POINT('Ctrl Pts',(17.1504041586296,-0.163958059400556,
112.8371493128));
#50975=CARTESIAN_POINT('Ctrl Pts',(17.3295581344551,-0.704127606930189,
112.871679546659));
#50976=CARTESIAN_POINT('Ctrl Pts',(17.7163063911852,-1.12497913550319,112.906352649458));
#50977=CARTESIAN_POINT('Ctrl Pts',(18.2431925961433,-1.35205912276461,112.941152109412));
#50978=CARTESIAN_POINT('Ctrl Pts',(18.8187741112765,-1.34427642838518,112.976089285723));
#50979=CARTESIAN_POINT('Ctrl Pts',(19.3432395618757,-1.10098396627254,113.011156346434));
#50980=CARTESIAN_POINT('Ctrl Pts',(19.7238494382154,-0.663159822701633,
113.046357078694));
#50981=CARTESIAN_POINT('Ctrl Pts',(19.8931314314799,-0.105956319615994,
113.08168722595));
#50982=CARTESIAN_POINT('Ctrl Pts',(19.8197719071333,0.473908286429459,113.117148366555));
#50983=CARTESIAN_POINT('Ctrl Pts',(19.514861434432,0.975046989864885,113.152737815001));
#50984=CARTESIAN_POINT('Ctrl Pts',(19.0301258646803,1.30913564752012,113.188455340763));
#50985=CARTESIAN_POINT('Ctrl Pts',(18.4491549165285,1.416472562517,113.224299311997));
#50986=CARTESIAN_POINT('Ctrl Pts',(17.8730091730699,1.27666467315962,113.260268611474));
#50987=CARTESIAN_POINT('Ctrl Pts',(17.4026034483492,0.912474225359778,113.296361769111));
#50988=CARTESIAN_POINT('Ctrl Pts',(17.1210280345443,0.386131812194797,113.332577359437));
#50989=CARTESIAN_POINT('Ctrl Pts',(17.0788544181136,-0.211299879373549,
113.368913814958));
#50990=CARTESIAN_POINT('Ctrl Pts',(17.2850565553758,-0.775695991436841,
113.405369493798));
#50991=CARTESIAN_POINT('Ctrl Pts',(17.705146965038,-1.20803167965084,113.441942712263));
#50992=CARTESIAN_POINT('Ctrl Pts',(18.2669652505624,-1.43177932086286,113.478631613973));
#50993=CARTESIAN_POINT('Ctrl Pts',(18.8730309513044,-1.40645905314605,113.51543444437));
#50994=CARTESIAN_POINT('Ctrl Pts',(19.4175618056869,-1.13497091574588,113.55234907248));
#50995=CARTESIAN_POINT('Ctrl Pts',(19.8048480383929,-0.663350581086933,
113.589373656825));
#50996=CARTESIAN_POINT('Ctrl Pts',(19.966197057422,-0.0729778537808475,
113.626505971993));
#50997=CARTESIAN_POINT('Ctrl Pts',(19.8720657245217,0.533549954628291,113.663743893195));
#50998=CARTESIAN_POINT('Ctrl Pts',(19.5374817640394,1.0501311842453,113.701085198819));
#50999=CARTESIAN_POINT('Ctrl Pts',(19.0196808505253,1.38594482959087,113.738527490934));
#51000=CARTESIAN_POINT('Ctrl Pts',(18.5101754020758,1.46526119175664,113.769811704289));
#51001=CARTESIAN_POINT('Ctrl Pts',(18.1090240872925,1.39960741569811,113.794887075397));
#51002=CARTESIAN_POINT('Ctrl Pts',(17.729655069815,1.25220225914757,113.819994103033));
#51003=CARTESIAN_POINT('Ctrl Pts',(17.3289300722954,0.923586877948104,113.851436567131));
#51004=CARTESIAN_POINT('Ctrl Pts',(17.0504721252432,0.365805609893722,113.889258509496));
#51005=CARTESIAN_POINT('Ctrl Pts',(17.0240290762783,-0.258477757917008,
113.927168961164));
#51006=CARTESIAN_POINT('Ctrl Pts',(17.2554238425403,-0.840447617959809,
113.965165177094));
#51007=CARTESIAN_POINT('Ctrl Pts',(17.7053131011304,-1.27808626113464,114.003244380208));
#51008=CARTESIAN_POINT('Ctrl Pts',(18.2959641544648,-1.49425702735341,114.041403784502));
#51009=CARTESIAN_POINT('Ctrl Pts',(18.9246622805112,-1.4502272181577,114.079640512388));
#51010=CARTESIAN_POINT('Ctrl Pts',(19.4816239236303,-1.15267110135651,114.117951609114));
#51011=CARTESIAN_POINT('Ctrl Pts',(19.8691907107327,-0.652639427392253,
114.156334167846));
#51012=CARTESIAN_POINT('Ctrl Pts',(20.0189810591327,-0.03683256961316,114.194785080069));
#51013=CARTESIAN_POINT('Ctrl Pts',(19.9039833865991,0.587522999416328,114.2333013558));
#51014=CARTESIAN_POINT('Ctrl Pts',(19.5434230734537,1.11127572106957,114.271879839515));
#51015=CARTESIAN_POINT('Ctrl Pts',(18.9995399107886,1.44259279852258,114.310517384521));
#51016=CARTESIAN_POINT('Ctrl Pts',(18.3668596633944,1.52297273199859,114.349210799966));
#51017=CARTESIAN_POINT('Ctrl Pts',(17.7556977562459,1.33767203016567,114.387956849117));
#51018=CARTESIAN_POINT('Ctrl Pts',(17.272914349715,0.918370107647551,114.426752263094));
#51019=CARTESIAN_POINT('Ctrl Pts',(17.0031861863323,0.337753138207008,114.46559374694));
#51020=CARTESIAN_POINT('Ctrl Pts',(16.9941242219495,-0.303088855509916,
114.504477951706));
#51021=CARTESIAN_POINT('Ctrl Pts',(17.2478715429229,-0.892350566926149,
114.543401543985));
#51022=CARTESIAN_POINT('Ctrl Pts',(17.720592505509,-1.32694200600498,114.582361077963));
#51023=CARTESIAN_POINT('Ctrl Pts',(18.3301332049521,-1.53077558802408,114.621353247865));
#51024=CARTESIAN_POINT('Ctrl Pts',(18.8635057740616,-1.47820468577621,114.653870882415));
#51025=CARTESIAN_POINT('Ctrl Pts',(19.2496685905278,-1.30821665552171,114.679897931973));
#51026=CARTESIAN_POINT('Ctrl Pts',(19.5923918636366,-1.06191387672613,114.705932982827));
#51027=CARTESIAN_POINT('Ctrl Pts',(19.9091081456583,-0.628734129737697,
114.738490494062));
#51028=CARTESIAN_POINT('Ctrl Pts',(20.0436482399265,0.00136013336455928,
114.777578396996));
#51029=CARTESIAN_POINT('Ctrl Pts',(19.9090928165798,0.631655323772199,114.816681421648));
#51030=CARTESIAN_POINT('Ctrl Pts',(19.5286868815429,1.1521949790643,114.855796201813));
#51031=CARTESIAN_POINT('Ctrl Pts',(18.9687372623033,1.47200625927751,114.894919129408));
#51032=CARTESIAN_POINT('Ctrl Pts',(18.3269247722238,1.53523233022917,114.934046750203));
#51033=CARTESIAN_POINT('Ctrl Pts',(17.7152334288248,1.33076841613399,114.973175454517));
#51034=CARTESIAN_POINT('Ctrl Pts',(17.2404725580255,0.894349558877001,115.012301840373));
#51035=CARTESIAN_POINT('Ctrl Pts',(16.9853446354984,0.302108848816737,115.051422158546));
#51036=CARTESIAN_POINT('Ctrl Pts',(16.9934993376988,-0.27079628228924,115.086187634404));
#51037=CARTESIAN_POINT('Ctrl Pts',(17.1704122775008,-0.733300276011371,
115.116598560424));
#51038=CARTESIAN_POINT('Ctrl Pts',(17.3615831320585,-0.98758491633179,115.136144037193));
#51039=CARTESIAN_POINT('Ctrl Pts',(17.5154254407977,-1.13081668225498,115.149171118788));
#51040=CARTESIAN_POINT('Ctrl Pts',(17.5970581795022,-1.19692836165928,115.155684477762));
#51041=CARTESIAN_POINT('Ctrl Pts',(17.6831967780099,-1.25709479715135,115.162197134421));
#51042=CARTESIAN_POINT('Ctrl Pts',(17.8633620834074,-1.36516570458449,115.175222025971));
#51043=CARTESIAN_POINT('Ctrl Pts',(18.1604819038664,-1.47854845945174,115.194753812955));
#51044=CARTESIAN_POINT('Ctrl Pts',(18.582786890695,-1.51417568969967,115.220787745291));
#51045=CARTESIAN_POINT('Ctrl Pts',(18.9983836416472,-1.43149328105734,115.246809679889));
#51046=CARTESIAN_POINT('Ctrl Pts',(19.374473528925,-1.23714016652633,115.27282057109));
#51047=CARTESIAN_POINT('Ctrl Pts',(19.6822598946567,-0.946311359030486,
115.298817689622));
#51048=CARTESIAN_POINT('Ctrl Pts',(19.8967480474023,-0.582015055171165,
115.324801432878));
#51049=CARTESIAN_POINT('Ctrl Pts',(20.0386193688326,-0.0359715504243672,
115.359425895719));
#51050=CARTESIAN_POINT('Ctrl Pts',(19.941536265269,0.535299448860012,115.394018366274));
#51051=CARTESIAN_POINT('Ctrl Pts',(19.6668198938765,0.944384240575756,115.424255526598));
#51052=CARTESIAN_POINT('Ctrl Pts',(19.4671125145751,1.13894829771433,115.44152396901));
#51053=CARTESIAN_POINT('Ctrl Pts',(19.2416596715355,1.3035791132569,115.458786271138));
#51054=CARTESIAN_POINT('Ctrl Pts',(19.0175256336374,1.40399060754221,115.473882214218));
#51055=CARTESIAN_POINT('Ctrl Pts',(18.8150509122225,1.45460978349152,115.486814484407));
#51056=CARTESIAN_POINT('Ctrl Pts',(18.7124011810244,1.4728082953005,115.493279478184));
#51057=CARTESIAN_POINT('Ctrl Pts',(18.6259805295674,1.48196183269604,115.498665769091));
#51058=CARTESIAN_POINT('Ctrl Pts',(18.5565983881251,1.48554743331276,115.502974301951));
#51059=CARTESIAN_POINT('Ctrl Pts',(18.275006635137,1.49093350233563,115.520445423601));
#51060=CARTESIAN_POINT('Ctrl Pts',(17.7643189677256,1.36044159259875,115.552131188091));
#51061=CARTESIAN_POINT('Ctrl Pts',(17.3297966145357,0.957318076594017,115.587783846009));
#51062=CARTESIAN_POINT('Ctrl Pts',(17.1366050542202,0.593850002954031,115.613220643608));
#51063=CARTESIAN_POINT('Ctrl Pts',(17.0708721336454,0.399095376421441,115.625931295202));
#51064=CARTESIAN_POINT('Ctrl Pts',(17.0385717481457,0.238286256682236,115.636095006768));
#51065=CARTESIAN_POINT('Ctrl Pts',(17.0000053948983,-0.0873641069959773,
115.656416799589));
#51066=CARTESIAN_POINT('Ctrl Pts',(17.0954817402936,-0.627463061463085,
115.689403138097));
#51067=CARTESIAN_POINT('Ctrl Pts',(17.5683032047114,-1.2202390337612,115.734986014693));
#51068=CARTESIAN_POINT('Ctrl Pts',(18.2073749791171,-1.48915585063008,115.776682365231));
#51069=CARTESIAN_POINT('Ctrl Pts',(18.827714255502,-1.46536270236631,115.81451460932));
#51070=CARTESIAN_POINT('Ctrl Pts',(19.3387291215206,-1.24252555435953,115.848504801486));
#51071=CARTESIAN_POINT('Ctrl Pts',(19.7323390465761,-0.84870905484788,115.882433969696));
#51072=CARTESIAN_POINT('Ctrl Pts',(19.917317868452,-0.424382854990528,115.910656120296));
#51073=CARTESIAN_POINT('Ctrl Pts',(19.9647758151583,-0.0623666971425709,
115.933200950891));
#51074=CARTESIAN_POINT('Ctrl Pts',(19.9494967945027,0.210678396553568,115.950093741532));
#51075=CARTESIAN_POINT('Ctrl Pts',(19.8946537689314,0.431722595099945,115.964156440341));
#51076=CARTESIAN_POINT('Ctrl Pts',(19.8267524040723,0.599946781165768,115.975398400255));
#51077=CARTESIAN_POINT('Ctrl Pts',(19.7020401592803,0.841706463647344,115.992253058882));
#51078=CARTESIAN_POINT('Ctrl Pts',(19.4317853790293,1.15561589179994,116.017502153899));
#51079=CARTESIAN_POINT('Ctrl Pts',(18.9444409086331,1.41307035879397,116.051097502054));
#51080=CARTESIAN_POINT('Ctrl Pts',(18.3979015457458,1.47453073660614,116.084620132269));
#51081=CARTESIAN_POINT('Ctrl Pts',(18.0004069582635,1.36793073631313,116.1097063674));
#51082=CARTESIAN_POINT('Ctrl Pts',(17.763366663899,1.23962198295239,116.126406802779));
#51083=CARTESIAN_POINT('Ctrl Pts',(17.6140480708204,1.1398854968943,116.137534246267));
#51084=CARTESIAN_POINT('Ctrl Pts',(17.3790836560323,0.929981622126309,116.156989690435));
#51085=CARTESIAN_POINT('Ctrl Pts',(17.2215832331742,0.679602546844773,116.175024509631));
#51086=CARTESIAN_POINT('Ctrl Pts',(17.1450352066694,0.469669982396278,116.188878617737));
#51087=CARTESIAN_POINT('Ctrl Pts',(17.1249441446997,0.405767087289566,116.193033537477));
#51088=CARTESIAN_POINT('Ctrl Pts',(17.1079301441042,0.340970796669862,116.197187251518));
#51089=CARTESIAN_POINT('Ctrl Pts',(17.0939473695056,0.275494153967272,116.201339691278));
#51090=CARTESIAN_POINT('Ctrl Pts',(17.0830227708597,0.209443458520346,116.205490910608));
#51091=CARTESIAN_POINT('Ctrl Pts',(17.0726655652121,0.120824547382831,116.211024197657));
#51092=CARTESIAN_POINT('Ctrl Pts',(17.0610173800014,-0.124379540531134,
116.226234061721));
#51093=CARTESIAN_POINT('Ctrl Pts',(17.1369245229291,-0.5249310381429,116.251084258337));
#51094=CARTESIAN_POINT('Ctrl Pts',(17.4255200195769,-0.984001270082908,
116.284135719174));
#51095=CARTESIAN_POINT('Ctrl Pts',(17.8607605682645,-1.30506353431624,116.317102617813));
#51096=CARTESIAN_POINT('Ctrl Pts',(18.3818866043649,-1.44455243472689,116.349983938512));
#51097=CARTESIAN_POINT('Ctrl Pts',(18.916470350186,-1.38418902476214,116.382777928971));
#51098=CARTESIAN_POINT('Ctrl Pts',(19.3908578736671,-1.13333494037052,116.415483428707));
#51099=CARTESIAN_POINT('Ctrl Pts',(19.662129258784,-0.817824110576332,116.440850810503));
#51100=CARTESIAN_POINT('Ctrl Pts',(19.7921004518703,-0.556121431420674,
116.458936888485));
#51101=CARTESIAN_POINT('Ctrl Pts',(19.8690655500124,-0.335782443963777,
116.473391787428));
#51102=CARTESIAN_POINT('Ctrl Pts',(19.9308282800101,0.0701141608640084,
116.498652513443));
#51103=CARTESIAN_POINT('Ctrl Pts',(19.7975561020439,0.653379656102897,116.534635638022));
#51104=CARTESIAN_POINT('Ctrl Pts',(19.3238121146665,1.18955843336623,116.577647401962));
#51105=CARTESIAN_POINT('Ctrl Pts',(18.6542573597491,1.43288587092525,116.620488268205));
#51106=CARTESIAN_POINT('Ctrl Pts',(17.9525424324882,1.32679118729713,116.663155847902));
#51107=CARTESIAN_POINT('Ctrl Pts',(17.4716228570456,0.961996366384522,116.699450989897));
#51108=CARTESIAN_POINT('Ctrl Pts',(17.2242845453766,0.540894020126181,116.729451046567));
#51109=CARTESIAN_POINT('Ctrl Pts',(17.0944240343639,0.041457592091441,116.761140226464));
#51110=CARTESIAN_POINT('Ctrl Pts',(17.2055334687691,-0.610901669378824,
116.8006093271));
#51111=CARTESIAN_POINT('Ctrl Pts',(17.7327235525077,-1.19996474577183,116.847741724244));
#51112=CARTESIAN_POINT('Ctrl Pts',(18.4886274023919,-1.41711476065944,116.894641370113));
#51113=CARTESIAN_POINT('Ctrl Pts',(19.2403913761961,-1.19999329817096,116.941306241231));
#51114=CARTESIAN_POINT('Ctrl Pts',(19.7589583230562,-0.618976305235332,
116.987734609023));
#51115=CARTESIAN_POINT('Ctrl Pts',(19.866303857657,0.0173456111094613,117.026226666982));
#51116=CARTESIAN_POINT('Ctrl Pts',(19.7405351404932,0.500732911611066,117.05690073817));
#51117=CARTESIAN_POINT('Ctrl Pts',(19.5511427517233,0.822664799957136,117.079846452937));
#51118=CARTESIAN_POINT('Ctrl Pts',(19.2800271222083,1.07822752115069,117.102732140544));
#51119=CARTESIAN_POINT('Ctrl Pts',(18.840099008821,1.30647550082486,117.13316636068));
#51120=CARTESIAN_POINT('Ctrl Pts',(18.2057864265544,1.34185814168128,117.171058787474));
#51121=CARTESIAN_POINT('Ctrl Pts',(17.5421074842011,0.974328602971076,117.216288928054));
#51122=CARTESIAN_POINT('Ctrl Pts',(17.1777038347398,0.313792671011465,117.261278280207));
#51123=CARTESIAN_POINT('Ctrl Pts',(17.2203225463522,-0.435464225919962,
117.306027156934));
#51124=CARTESIAN_POINT('Ctrl Pts',(17.652724667813,-1.04386133116569,117.350536141848));
#51125=CARTESIAN_POINT('Ctrl Pts',(18.3388239098277,-1.32745573236693,117.39480611765));
#51126=CARTESIAN_POINT('Ctrl Pts',(19.0667149711576,-1.20320856043253,117.438838249758));
#51127=CARTESIAN_POINT('Ctrl Pts',(19.6139786084161,-0.713397943859653,
117.482633994782));
#51128=CARTESIAN_POINT('Ctrl Pts',(19.8156811381899,-0.0112791664943189,
117.526195091984));
#51129=CARTESIAN_POINT('Ctrl Pts',(19.6140022601783,0.686784214414896,117.569523562413));
#51130=CARTESIAN_POINT('Ctrl Pts',(19.0747275941947,1.16798331893147,117.612621710931));
#51131=CARTESIAN_POINT('Ctrl Pts',(18.3658643708616,1.28788138840837,117.655492120034));
#51132=CARTESIAN_POINT('Ctrl Pts',(17.7053431257873,1.01371279747136,117.69813764302));
#51133=CARTESIAN_POINT('Ctrl Pts',(17.2940790801678,0.433188982502828,117.740561406275));
#51134=CARTESIAN_POINT('Ctrl Pts',(17.2549003691858,-0.273508324804743,
117.782766808914));
#51135=CARTESIAN_POINT('Ctrl Pts',(17.5959737510632,-0.889574255288579,
117.824757505323));
#51136=CARTESIAN_POINT('Ctrl Pts',(18.2094168755739,-1.22806570874149,117.866537413039));
#51137=CARTESIAN_POINT('Ctrl Pts',(18.9055013390443,-1.18847566627298,117.908110699435));
#51138=CARTESIAN_POINT('Ctrl Pts',(19.4709991235593,-0.786645501256251,
117.949481800211));
#51139=CARTESIAN_POINT('Ctrl Pts',(19.7349121554302,-0.148494032303403,
117.990655350317));
#51140=CARTESIAN_POINT('Ctrl Pts',(19.6384296844279,0.41595364745626,118.024806143826));
#51141=CARTESIAN_POINT('Ctrl Pts',(19.3912822005401,0.783910465160815,118.052032979065));
#51142=CARTESIAN_POINT('Ctrl Pts',(19.0539455301924,1.06997780245999,118.079198326187));
#51143=CARTESIAN_POINT('Ctrl Pts',(18.5086041618223,1.22692728472169,118.113040992046));
#51144=CARTESIAN_POINT('Ctrl Pts',(17.8570681242743,1.03871258992206,118.153475788182));
#51145=CARTESIAN_POINT('Ctrl Pts',(17.4074661243136,0.535028360348281,118.193739748399));
#51146=CARTESIAN_POINT('Ctrl Pts',(17.295184410072,-0.12802353903353,118.233838994046));
#51147=CARTESIAN_POINT('Ctrl Pts',(17.5518536435643,-0.746678185841251,
118.273779650817));
#51148=CARTESIAN_POINT('Ctrl Pts',(18.09623557474,-1.13252353284961,118.313568149567));
#51149=CARTESIAN_POINT('Ctrl Pts',(18.7600131800788,-1.16944565236424,118.353211038631));
#51150=CARTESIAN_POINT('Ctrl Pts',(19.3396804878931,-0.848740522078599,
118.392715097256));
#51151=CARTESIAN_POINT('Ctrl Pts',(19.6587833880623,-0.270665095166121,
118.432087186673));
#51152=CARTESIAN_POINT('Ctrl Pts',(19.6216208701028,0.386364157140476,118.471334476116));
#51153=CARTESIAN_POINT('Ctrl Pts',(19.2416211971827,0.921545428620454,118.510464030869));
#51154=CARTESIAN_POINT('Ctrl Pts',(18.7378784200697,1.12977499085113,118.542980260458));
#51155=CARTESIAN_POINT('Ctrl Pts',(18.3152260681784,1.11706291748731,118.56894164302));
#51156=CARTESIAN_POINT('Ctrl Pts',(18.013631331558,1.02122659296196,118.588388203893));
#51157=CARTESIAN_POINT('Ctrl Pts',(17.7507020897944,0.845342251383026,118.607810663731));
#51158=CARTESIAN_POINT('Ctrl Pts',(17.5469576086983,0.604112404067775,118.62721063314));
#51159=CARTESIAN_POINT('Ctrl Pts',(17.418115189222,0.316066123273868,118.646588439489));
#51160=CARTESIAN_POINT('Ctrl Pts',(17.3740914074908,0.00406156609269027,
118.665945648007));
#51161=CARTESIAN_POINT('Ctrl Pts',(17.418105330468,-0.307731076500601,118.68528270408));
#51162=CARTESIAN_POINT('Ctrl Pts',(17.5252095909573,-0.546868258948941,
118.701381492349));
#51163=CARTESIAN_POINT('Ctrl Pts',(17.6479384162453,-0.714878730507821,
118.714251085885));
#51164=CARTESIAN_POINT('Ctrl Pts',(17.7929243818857,-0.863723509943578,
118.727115583167));
#51165=CARTESIAN_POINT('Ctrl Pts',(18.0972164483336,-1.06793358028532,118.74961267773));
#51166=CARTESIAN_POINT('Ctrl Pts',(18.6276378637832,-1.15815365828481,118.781712261723));
#51167=CARTESIAN_POINT('Ctrl Pts',(19.2238118827329,-0.91106020954,118.820176086249));
#51168=CARTESIAN_POINT('Ctrl Pts',(19.5340790733567,-0.473298914368946,
118.852189669591));
#51169=CARTESIAN_POINT('Ctrl Pts',(19.6045033571726,-0.115359348913955,
118.874582530202));
#51170=CARTESIAN_POINT('Ctrl Pts',(19.6017475647411,0.0911640829913528,
118.88737350014));
#51171=CARTESIAN_POINT('Ctrl Pts',(19.5700196370974,0.29559108219492,118.900162446911));
#51172=CARTESIAN_POINT('Ctrl Pts',(19.4770780543413,0.538342967989427,118.916143236651));
#51173=CARTESIAN_POINT('Ctrl Pts',(19.2273588011135,0.871529045839169,118.941704029868));
#51174=CARTESIAN_POINT('Ctrl Pts',(18.7588367207674,1.13058490335296,118.973640684375));
#51175=CARTESIAN_POINT('Ctrl Pts',(18.1172887995021,1.09452313569986,119.011950738852));
#51176=CARTESIAN_POINT('Ctrl Pts',(17.593388380079,0.722780783019972,119.050254797413));
#51177=CARTESIAN_POINT('Ctrl Pts',(17.3886684004257,0.228286678671025,119.082177254148));
#51178=CARTESIAN_POINT('Ctrl Pts',(17.4011923319186,-0.187547154371747,
119.107720239302));
#51179=CARTESIAN_POINT('Ctrl Pts',(17.479741012236,-0.43518291567232,119.123688362763));
#51180=CARTESIAN_POINT('Ctrl Pts',(17.5695979738663,-0.592074644579124,
119.134867535548));
#51181=CARTESIAN_POINT('Ctrl Pts',(17.6297289359476,-0.675697287840335,
119.1412564699));
#51182=CARTESIAN_POINT('Ctrl Pts',(17.6957161316275,-0.754921963867992,
119.147645877012));
#51183=CARTESIAN_POINT('Ctrl Pts',(17.7882499830905,-0.84489988474299,119.155633946795));
#51184=CARTESIAN_POINT('Ctrl Pts',(17.9550205699679,-0.966828303763707,
119.168415926821));
#51185=CARTESIAN_POINT('Ctrl Pts',(18.1925073400234,-1.07312652027406,119.184398568056));
#51186=CARTESIAN_POINT('Ctrl Pts',(18.5018237176362,-1.11680179614521,119.203585076302));
#51187=CARTESIAN_POINT('Ctrl Pts',(18.8112727437243,-1.07312083019676,119.222781017226));
#51188=CARTESIAN_POINT('Ctrl Pts',(19.0966922989243,-0.945425429896232,
119.241986576724));
#51189=CARTESIAN_POINT('Ctrl Pts',(19.3357397025375,-0.743574694906012,
119.261203548649));
#51190=CARTESIAN_POINT('Ctrl Pts',(19.5096763702265,-0.483296157484075,
119.280432047793));
#51191=CARTESIAN_POINT('Ctrl Pts',(19.604829263032,-0.184805761734769,119.299674358162));
#51192=CARTESIAN_POINT('Ctrl Pts',(19.6136282032755,0.128548869667553,119.318929822438));
#51193=CARTESIAN_POINT('Ctrl Pts',(19.5483562428395,0.381754662526241,119.334989622353));
#51194=CARTESIAN_POINT('Ctrl Pts',(19.4555027014667,0.567586338753027,119.347844753828));
#51195=CARTESIAN_POINT('Ctrl Pts',(19.3083285466207,0.781707993580481,119.363921119013));
#51196=CARTESIAN_POINT('Ctrl Pts',(19.0213883195784,1.0173014385066,119.386447876364));
#51197=CARTESIAN_POINT('Ctrl Pts',(18.5601806816014,1.14326482672377,119.415452744608));
#51198=CARTESIAN_POINT('Ctrl Pts',(18.0870469004768,1.06976794361554,119.444502870166));
#51199=CARTESIAN_POINT('Ctrl Pts',(17.6845073765261,0.809000046868888,119.473601565479));
#51200=CARTESIAN_POINT('Ctrl Pts',(17.4231181242213,0.405838898540841,119.502752060927));
#51201=CARTESIAN_POINT('Ctrl Pts',(17.3490598832109,-0.0697983875198877,
119.531957712525));
#51202=CARTESIAN_POINT('Ctrl Pts',(17.4759534440631,-0.535171725229621,
119.561221496182));
#51203=CARTESIAN_POINT('Ctrl Pts',(17.7314548399343,-0.846550437506931,
119.58565944407));
#51204=CARTESIAN_POINT('Ctrl Pts',(17.999207559364,-1.0170868157945,119.605241751292));
#51205=CARTESIAN_POINT('Ctrl Pts',(18.2967905723551,-1.12863703662001,119.624846422395));
#51206=CARTESIAN_POINT('Ctrl Pts',(18.701022235534,-1.14581433888424,119.649394327387));
#51207=CARTESIAN_POINT('Ctrl Pts',(19.1533010528138,-0.965969567310355,
119.678922596865));
#51208=CARTESIAN_POINT('Ctrl Pts',(19.4935242230618,-0.616264784255005,
119.708524488639));
#51209=CARTESIAN_POINT('Ctrl Pts',(19.6616806751607,-0.15688731828813,119.738203011753));
#51210=CARTESIAN_POINT('Ctrl Pts',(19.6274500840142,0.332402173060607,119.767961008938));
#51211=CARTESIAN_POINT('Ctrl Pts',(19.3957290628344,0.766238455283539,119.797801335606));
#51212=CARTESIAN_POINT('Ctrl Pts',(19.0059018782433,1.06845895995986,119.827726746298));
#51213=CARTESIAN_POINT('Ctrl Pts',(18.5252515327408,1.18543071772727,119.857739979944));
#51214=CARTESIAN_POINT('Ctrl Pts',(18.037234743022,1.09564506473,119.887843657137));
#51215=CARTESIAN_POINT('Ctrl Pts',(17.6956019306827,0.860470084296629,119.913007640695));
#51216=CARTESIAN_POINT('Ctrl Pts',(17.4972936032911,0.600305772965447,119.93318661626));
#51217=CARTESIAN_POINT('Ctrl Pts',(17.3569038509229,0.304279815543778,119.953397785618));
#51218=CARTESIAN_POINT('Ctrl Pts',(17.3041660284991,-0.109796929925252,
119.978723169803));
#51219=CARTESIAN_POINT('Ctrl Pts',(17.4498994353956,-0.59078091166106,120.009214030095));
#51220=CARTESIAN_POINT('Ctrl Pts',(17.7804655429487,-0.971566966837065,
120.039807705564));
#51221=CARTESIAN_POINT('Ctrl Pts',(18.2393086861239,-1.18486584665598,120.07050641441));
#51222=CARTESIAN_POINT('Ctrl Pts',(18.7470163437987,-1.1921729938516,120.101312384752));
#51223=CARTESIAN_POINT('Ctrl Pts',(19.215087635489,-0.990765643040621,120.132227714623));
#51224=CARTESIAN_POINT('Ctrl Pts',(19.5613155231427,-0.614392148089554,
120.163254460057));
#51225=CARTESIAN_POINT('Ctrl Pts',(19.7242152497417,-0.127659401515012,
120.194394583265));
#51226=CARTESIAN_POINT('Ctrl Pts',(19.6739207775415,0.385049104109546,120.225649979257));
#51227=CARTESIAN_POINT('Ctrl Pts',(19.4176458057697,0.834175476321175,120.257022460356));
#51228=CARTESIAN_POINT('Ctrl Pts',(18.998699632526,1.14061462596676,120.288513762116));
#51229=CARTESIAN_POINT('Ctrl Pts',(18.4891879156563,1.24962833189955,120.320125537776));
#51230=CARTESIAN_POINT('Ctrl Pts',(17.9776202690671,1.14060959036587,120.351859359126));
#51231=CARTESIAN_POINT('Ctrl Pts',(17.5535525982464,0.830952823101709,120.383716714854));
#51232=CARTESIAN_POINT('Ctrl Pts',(17.2919248389954,0.373308289212946,120.415699010712));
#51233=CARTESIAN_POINT('Ctrl Pts',(17.2398314509524,-0.153353235375788,
120.447807567348));
#51234=CARTESIAN_POINT('Ctrl Pts',(17.4080575955601,-0.657352082285856,
120.480043619757));
#51235=CARTESIAN_POINT('Ctrl Pts',(17.7689006127485,-1.05024513051325,120.512408315922));
#51236=CARTESIAN_POINT('Ctrl Pts',(18.2607097297302,-1.26233444597482,120.544902716827));
#51237=CARTESIAN_POINT('Ctrl Pts',(18.7984052352737,-1.25502080659343,120.577527795704));
#51238=CARTESIAN_POINT('Ctrl Pts',(19.2881848794747,-1.0278144553583,120.610284437319));
#51239=CARTESIAN_POINT('Ctrl Pts',(19.6438781749597,-0.61873033468329,120.643173436616));
#51240=CARTESIAN_POINT('Ctrl Pts',(19.8020987090859,-0.0979461688159152,
120.676195498978));
#51241=CARTESIAN_POINT('Ctrl Pts',(19.7335320823132,0.444227716269205,120.709351239055));
#51242=CARTESIAN_POINT('Ctrl Pts',(19.4483480211883,0.912997875362089,120.742641182014));
#51243=CARTESIAN_POINT('Ctrl Pts',(18.9947430992497,1.22566304840365,120.776065760162));
#51244=CARTESIAN_POINT('Ctrl Pts',(18.4508057834443,1.32618611440986,120.809625317582));
#51245=CARTESIAN_POINT('Ctrl Pts',(17.9110852264692,1.19525527808251,120.843320100399));
#51246=CARTESIAN_POINT('Ctrl Pts',(17.4701505494149,0.853917314146234,120.877150274951));
#51247=CARTESIAN_POINT('Ctrl Pts',(17.2060388865232,0.360310149126953,120.911115893666));
#51248=CARTESIAN_POINT('Ctrl Pts',(17.1664153816519,-0.200398871563149,
120.945216959522));
#51249=CARTESIAN_POINT('Ctrl Pts',(17.3116264220795,-0.597882955951257,
120.970894211169));
#51250=CARTESIAN_POINT('Ctrl Pts',(17.4713230749973,-0.824292723162997,
120.988054644643));
#51251=CARTESIAN_POINT('Ctrl Pts',(17.5930295495418,-0.963403094471689,
120.999506127854));
#51252=CARTESIAN_POINT('Ctrl Pts',(17.8429222056168,-1.17180944522949,121.019575839724));
#51253=CARTESIAN_POINT('Ctrl Pts',(18.2831358555107,-1.3472696457857,121.048331046648));
#51254=CARTESIAN_POINT('Ctrl Pts',(18.8536622082132,-1.32345121615729,121.082971735828));
#51255=CARTESIAN_POINT('Ctrl Pts',(19.3666123501032,-1.06776818445665,121.11774633767));
#51256=CARTESIAN_POINT('Ctrl Pts',(19.7318189194698,-0.623135744515387,
121.152654299799));
#51257=CARTESIAN_POINT('Ctrl Pts',(19.8841229814082,-0.0660261383455702,
121.187694946127));
#51258=CARTESIAN_POINT('Ctrl Pts',(19.7952691811095,0.506861240356869,121.22286752838));
#51259=CARTESIAN_POINT('Ctrl Pts',(19.4789909654556,0.995298037449156,121.258171199464));
#51260=CARTESIAN_POINT('Ctrl Pts',(18.9889997447394,1.31312136899922,121.293605027892));
#51261=CARTESIAN_POINT('Ctrl Pts',(18.4098258930854,1.40341469896206,121.329167991327));
#51262=CARTESIAN_POINT('Ctrl Pts',(17.8422514541543,1.2487159173822,121.364858980876));
#51263=CARTESIAN_POINT('Ctrl Pts',(17.3857498366357,0.874358654879244,121.400676801254));
#51264=CARTESIAN_POINT('Ctrl Pts',(17.1210452069084,0.344343613450397,121.436620170121));
#51265=CARTESIAN_POINT('Ctrl Pts',(17.0958251015548,-0.249607404749667,
121.472687721701));
#51266=CARTESIAN_POINT('Ctrl Pts',(17.3161507636215,-0.803935931388206,
121.508878001574));
#51267=CARTESIAN_POINT('Ctrl Pts',(17.7451068582081,-1.22131693446959,121.545189480257));
#51268=CARTESIAN_POINT('Ctrl Pts',(18.3089795239874,-1.42776624833079,121.581620531396));
#51269=CARTESIAN_POINT('Ctrl Pts',(18.9099344796403,-1.38575758159487,121.618169476059));
#51270=CARTESIAN_POINT('Ctrl Pts',(19.443003408243,-1.10105588624391,121.654834501032));
#51271=CARTESIAN_POINT('Ctrl Pts',(19.814447080578,-0.621956720707161,121.691613814933));
#51272=CARTESIAN_POINT('Ctrl Pts',(19.9582412943487,-0.0311460741792062,
121.728505359742));
#51273=CARTESIAN_POINT('Ctrl Pts',(19.8478423707596,0.568675584892993,121.765507307081));
#51274=CARTESIAN_POINT('Ctrl Pts',(19.5010738542693,1.07254435780881,121.802617407826));
#51275=CARTESIAN_POINT('Ctrl Pts',(18.9772465487843,1.39174398963045,121.839833580231));
#51276=CARTESIAN_POINT('Ctrl Pts',(18.3670349923433,1.46935809393124,121.877153590267));
#51277=CARTESIAN_POINT('Ctrl Pts',(17.7767415245785,1.29047771303663,121.91457510912));
#51278=CARTESIAN_POINT('Ctrl Pts',(17.3097639110163,0.88502066898406,121.952095792454));
#51279=CARTESIAN_POINT('Ctrl Pts',(17.0484530789278,0.322744770605088,121.98971320241));
#51280=CARTESIAN_POINT('Ctrl Pts',(17.0395741793232,-0.29877511550778,122.027424807101));
#51281=CARTESIAN_POINT('Ctrl Pts',(17.2859276060077,-0.871100232399064,
122.065228088574));
#51282=CARTESIAN_POINT('Ctrl Pts',(17.7456411246251,-1.29387701195727,122.103120366714));
#51283=CARTESIAN_POINT('Ctrl Pts',(18.3392916665445,-1.49245955151488,122.141098983942));
#51284=CARTESIAN_POINT('Ctrl Pts',(18.9636467540723,-1.43110986029732,122.179161195417));
#51285=CARTESIAN_POINT('Ctrl Pts',(19.5096427527803,-1.11943132446743,122.217304158637));
#51286=CARTESIAN_POINT('Ctrl Pts',(19.8814701962045,-0.610888906864692,
122.255525076564));
#51287=CARTESIAN_POINT('Ctrl Pts',(20.0134084028596,0.00638374819795061,
122.293820960483));
#51288=CARTESIAN_POINT('Ctrl Pts',(19.8814680357448,0.624863883396621,122.332188933733));
#51289=CARTESIAN_POINT('Ctrl Pts',(19.5077372244298,1.13643840843378,122.370625859871));
#51290=CARTESIAN_POINT('Ctrl Pts',(18.9567207702999,1.45127557085421,122.409128868261));
#51291=CARTESIAN_POINT('Ctrl Pts',(18.3241217337611,1.51368240153528,122.447694658652));
#51292=CARTESIAN_POINT('Ctrl Pts',(17.7202826349282,1.31196813537611,122.486320211507));
#51293=CARTESIAN_POINT('Ctrl Pts',(17.2508103246174,0.880536550537675,122.525002285958));
#51294=CARTESIAN_POINT('Ctrl Pts',(16.9981604164449,0.294249197224712,122.563737660687));
#51295=CARTESIAN_POINT('Ctrl Pts',(17.0060423714049,-0.274042958784632,
122.598213625129));
#51296=CARTESIAN_POINT('Ctrl Pts',(17.1818706810392,-0.73303144472968,122.628410343682));
#51297=CARTESIAN_POINT('Ctrl Pts',(17.5191721715142,-1.18310393837461,122.662947355674));
#51298=CARTESIAN_POINT('Ctrl Pts',(18.1531350042187,-1.53390972067408,122.706165522702));
#51299=CARTESIAN_POINT('Ctrl Pts',(19.0227874461394,-1.48519217492529,122.758094642985));
#51300=CARTESIAN_POINT('Ctrl Pts',(19.7338192740336,-0.980774656373063,
122.810082875595));
#51301=CARTESIAN_POINT('Ctrl Pts',(20.067922277282,-0.174626022127283,122.862122158172));
#51302=CARTESIAN_POINT('Ctrl Pts',(19.921708544036,0.68662933685667,122.914204231648));
#51303=CARTESIAN_POINT('Ctrl Pts',(19.4364076102001,1.22943043838242,122.957634782588));
#51304=CARTESIAN_POINT('Ctrl Pts',(18.9192757117743,1.45961435937841,122.992392354061));
#51305=CARTESIAN_POINT('Ctrl Pts',(18.5146998498917,1.51727349960696,123.017500336371));
#51306=CARTESIAN_POINT('Ctrl Pts',(18.1254479581993,1.46800683442712,123.041646590114));
#51307=CARTESIAN_POINT('Ctrl Pts',(17.65765089863,1.28524666288511,123.072557499479));
#51308=CARTESIAN_POINT('Ctrl Pts',(17.1864413110902,0.84817385210292,123.111201426539));
#51309=CARTESIAN_POINT('Ctrl Pts',(16.9818560590682,0.238917012125818,123.149847159061));
#51310=CARTESIAN_POINT('Ctrl Pts',(17.0077477842283,-0.262729802221198,
123.180762273051));
#51311=CARTESIAN_POINT('Ctrl Pts',(17.1549558342261,-0.742832495303323,
123.211674984775));
#51312=CARTESIAN_POINT('Ctrl Pts',(17.5555345576308,-1.24539323375308,123.250310351106));
#51313=CARTESIAN_POINT('Ctrl Pts',(18.2066766855254,-1.51951236558385,123.292795159863));
#51314=CARTESIAN_POINT('Ctrl Pts',(18.8397001520098,-1.49532848220801,123.331402485356));
#51315=CARTESIAN_POINT('Ctrl Pts',(19.361933038917,-1.2676766648096,123.36613474992));
#51316=CARTESIAN_POINT('Ctrl Pts',(19.7646594303858,-0.864798752237798,
123.400850262946));
#51317=CARTESIAN_POINT('Ctrl Pts',(19.992247479715,-0.343129638214644,123.435546682762));
#51318=CARTESIAN_POINT('Ctrl Pts',(20.0134975784261,0.225403110709894,123.470221342828));
#51319=CARTESIAN_POINT('Ctrl Pts',(19.8256820027275,0.761912608646907,123.504872214536));
#51320=CARTESIAN_POINT('Ctrl Pts',(19.516918297423,1.12076930887003,123.533725575818));
#51321=CARTESIAN_POINT('Ctrl Pts',(19.2041810039955,1.32499554631978,123.556794181975));
#51322=CARTESIAN_POINT('Ctrl Pts',(18.8020588760868,1.49233095074489,123.583695662073));
#51323=CARTESIAN_POINT('Ctrl Pts',(18.1960164011262,1.52254678614699,123.620174599657));
#51324=CARTESIAN_POINT('Ctrl Pts',(17.6216673694243,1.24564088295246,123.658522649907));
#51325=CARTESIAN_POINT('Ctrl Pts',(17.2833151529131,0.880111521286915,123.689167672577));
#51326=CARTESIAN_POINT('Ctrl Pts',(17.1050831264071,0.552606139546885,123.712134313292));
#51327=CARTESIAN_POINT('Ctrl Pts',(16.9816547923198,0.0706959663075114,
123.742732173804));
#51328=CARTESIAN_POINT('Ctrl Pts',(17.0529092044043,-0.496279877167484,
123.777112906262));
#51329=CARTESIAN_POINT('Ctrl Pts',(17.3864957981709,-1.02604026133052,123.815255128178));
#51330=CARTESIAN_POINT('Ctrl Pts',(17.857593613417,-1.37397111071324,123.850964243175));
#51331=CARTESIAN_POINT('Ctrl Pts',(18.4515962038669,-1.51829287387834,123.888044644597));
#51332=CARTESIAN_POINT('Ctrl Pts',(19.0746522170704,-1.40326627781162,123.926485479005));
#51333=CARTESIAN_POINT('Ctrl Pts',(19.5520449521414,-1.07433327180886,123.961659739466));
#51334=CARTESIAN_POINT('Ctrl Pts',(19.7870135179904,-0.729922634281818,
123.987199138138));
#51335=CARTESIAN_POINT('Ctrl Pts',(19.9172825726675,-0.412389600249223,
124.008461419526));
#51336=CARTESIAN_POINT('Ctrl Pts',(19.9813821346012,-0.0901260863987032,
124.028642265937));
#51337=CARTESIAN_POINT('Ctrl Pts',(19.9464919895927,0.322871316840072,124.054100150558));
#51338=CARTESIAN_POINT('Ctrl Pts',(19.7988560610193,0.709540527634926,124.079522689038));
#51339=CARTESIAN_POINT('Ctrl Pts',(19.5502809158787,1.03976970882056,124.104909666808));
#51340=CARTESIAN_POINT('Ctrl Pts',(19.2205019215012,1.28789198571529,124.130259814538));
#51341=CARTESIAN_POINT('Ctrl Pts',(18.8675304954949,1.42261786918923,124.153463104108));
#51342=CARTESIAN_POINT('Ctrl Pts',(18.5284830739033,1.46304402439271,124.174529127565));
#51343=CARTESIAN_POINT('Ctrl Pts',(18.1207874834896,1.4260614944801,124.199779233887));
#51344=CARTESIAN_POINT('Ctrl Pts',(17.6438940253866,1.2206283929953,124.231286143554));
#51345=CARTESIAN_POINT('Ctrl Pts',(17.2233006573008,0.762755887841534,124.269003086711));
#51346=CARTESIAN_POINT('Ctrl Pts',(17.0268753162689,0.174604680404742,124.306625880741));
#51347=CARTESIAN_POINT('Ctrl Pts',(17.0876702801681,-0.440949978759675,
124.344152137287));
#51348=CARTESIAN_POINT('Ctrl Pts',(17.3937696919832,-0.976537539345891,
124.381579352596));
#51349=CARTESIAN_POINT('Ctrl Pts',(17.8905867113653,-1.33941486357803,124.41890518565));
#51350=CARTESIAN_POINT('Ctrl Pts',(18.4906153716989,-1.46735186134762,124.456127313473));
#51351=CARTESIAN_POINT('Ctrl Pts',(19.0888593629504,-1.33941777641846,124.493243511411));
#51352=CARTESIAN_POINT('Ctrl Pts',(19.5812312587733,-0.97933823951139,124.530251612046));
#51353=CARTESIAN_POINT('Ctrl Pts',(19.8826841702414,-0.45113379238791,124.567149528264));
#51354=CARTESIAN_POINT('Ctrl Pts',(19.9419184246875,0.15228968271957,124.603935243626));
#51355=CARTESIAN_POINT('Ctrl Pts',(19.7501149544944,0.72549274055214,124.640606820178));
#51356=CARTESIAN_POINT('Ctrl Pts',(19.3422099788232,1.16895227798287,124.677162396834));
#51357=CARTESIAN_POINT('Ctrl Pts',(18.7905344628525,1.4063573661534,124.713600191806));
#51358=CARTESIAN_POINT('Ctrl Pts',(18.1919768114847,1.39775285517752,124.749918502117));
#51359=CARTESIAN_POINT('Ctrl Pts',(17.650949463827,1.14625964667207,124.786115706138));
#51360=CARTESIAN_POINT('Ctrl Pts',(17.2611574231578,0.697245715919318,124.822190264427));
#51361=CARTESIAN_POINT('Ctrl Pts',(17.0893550841156,0.130141700592976,124.858140721292));
#51362=CARTESIAN_POINT('Ctrl Pts',(17.1639091103876,-0.45562104348777,124.893965705161));
#51363=CARTESIAN_POINT('Ctrl Pts',(17.4701273616986,-0.958058662722596,
124.929663929076));
#51364=CARTESIAN_POINT('Ctrl Pts',(17.9531200725725,-1.29040433417455,124.965234192037));
#51365=CARTESIAN_POINT('Ctrl Pts',(18.5276405431088,-1.39610073357796,125.000675380104));
#51366=CARTESIAN_POINT('Ctrl Pts',(19.0931401580165,-1.25842381920182,125.035986467183));
#51367=CARTESIAN_POINT('Ctrl Pts',(19.5513770476802,-0.903101174061878,
125.071166515444));
#51368=CARTESIAN_POINT('Ctrl Pts',(19.8234925261704,-0.393520928653388,
125.106214675531));
#51369=CARTESIAN_POINT('Ctrl Pts',(19.863585446952,0.18057846519377,125.141130187601));
#51370=CARTESIAN_POINT('Ctrl Pts',(19.6664477552688,0.718918428921209,125.175912381995));
#51371=CARTESIAN_POINT('Ctrl Pts',(19.2681597354425,1.12820343239091,125.210560679702));
#51372=CARTESIAN_POINT('Ctrl Pts',(18.7394968083553,1.33829386724977,125.245074592494));
#51373=CARTESIAN_POINT('Ctrl Pts',(18.1733515600056,1.31422440666254,125.279453723019));
#51374=CARTESIAN_POINT('Ctrl Pts',(17.6684072336029,1.06200918227394,125.313697765461));
#51375=CARTESIAN_POINT('Ctrl Pts',(17.3119333434095,0.62727345561428,125.347806505814));
#51376=CARTESIAN_POINT('Ctrl Pts',(17.164703194465,0.0870075502303987,125.381779821996));
#51377=CARTESIAN_POINT('Ctrl Pts',(17.2506394082675,-0.464067284867245,
125.415617683646));
#51378=CARTESIAN_POINT('Ctrl Pts',(17.5529500312885,-0.93010635281992,125.449320152153));
#51379=CARTESIAN_POINT('Ctrl Pts',(18.0173742562096,-1.23080998259887,125.482887380882));
#51380=CARTESIAN_POINT('Ctrl Pts',(18.5619148970354,-1.31525442806852,125.516319615136));
#51381=CARTESIAN_POINT('Ctrl Pts',(19.0913123481237,-1.17050448618906,125.54961719185));
#51382=CARTESIAN_POINT('Ctrl Pts',(19.5137054329361,-0.823554001177106,
125.582780539051));
#51383=CARTESIAN_POINT('Ctrl Pts',(19.7565657136191,-0.336311890299757,
125.615810175785));
#51384=CARTESIAN_POINT('Ctrl Pts',(19.7791421686803,0.205437475860851,125.64870671201));
#51385=CARTESIAN_POINT('Ctrl Pts',(19.5792831503527,0.707131271594729,125.681470848156));
#51386=CARTESIAN_POINT('Ctrl Pts',(19.1934974783569,1.08192650056308,125.714103374504));
#51387=CARTESIAN_POINT('Ctrl Pts',(18.6903000531182,1.26572269937722,125.74660517022));
#51388=CARTESIAN_POINT('Ctrl Pts',(18.1580528586921,1.22811231780654,125.778977203127));
#51389=CARTESIAN_POINT('Ctrl Pts',(17.6894582924859,0.977390643756032,125.811220529498));
#51390=CARTESIAN_POINT('Ctrl Pts',(17.3654249182296,0.55880467658169,125.843336292948));
#51391=CARTESIAN_POINT('Ctrl Pts',(17.2411113552341,0.0464007134562138,
125.875325723779));
#51392=CARTESIAN_POINT('Ctrl Pts',(17.3365525714722,-0.470062155704644,
125.907190137343));
#51393=CARTESIAN_POINT('Ctrl Pts',(17.6334582774054,-0.900821679431447,
125.938930933878));
#51394=CARTESIAN_POINT('Ctrl Pts',(18.078689306533,-1.17169762162142,125.970549597961));
#51395=CARTESIAN_POINT('Ctrl Pts',(18.593754716555,-1.23684923441498,126.002047697117));
#51396=CARTESIAN_POINT('Ctrl Pts',(19.0886338471913,-1.0865147767173,126.033426880753));
#51397=CARTESIAN_POINT('Ctrl Pts',(19.4774918201155,-0.748430497103195,
126.064688878174));
#51398=CARTESIAN_POINT('Ctrl Pts',(19.6935481589647,-0.282732209663939,
126.095835498253));
#51399=CARTESIAN_POINT('Ctrl Pts',(19.7005261381603,0.228725868558277,126.126868628752));
#51400=CARTESIAN_POINT('Ctrl Pts',(19.4987238371462,0.696739517761545,126.157790234506));
#51401=CARTESIAN_POINT('Ctrl Pts',(19.1246955649095,1.04029099805458,126.188602356125));
#51402=CARTESIAN_POINT('Ctrl Pts',(18.6446468213007,1.20055180571536,126.219307107577));
#51403=CARTESIAN_POINT('Ctrl Pts',(18.1427337757278,1.15093580581614,126.24990667576));
#51404=CARTESIAN_POINT('Ctrl Pts',(17.7063324713574,0.901488522300449,126.280403319565));
#51405=CARTESIAN_POINT('Ctrl Pts',(17.4108529526162,0.496892712939118,126.310799367952));
#51406=CARTESIAN_POINT('Ctrl Pts',(17.3067328954843,0.0084812245335301,
126.34109721811));
#51407=CARTESIAN_POINT('Ctrl Pts',(17.4108490145204,-0.47831756693869,126.371299332964));
#51408=CARTESIAN_POINT('Ctrl Pts',(17.7038045321021,-0.878895943230857,
126.401408240409));
#51409=CARTESIAN_POINT('Ctrl Pts',(18.1335240920449,-1.12414442958507,126.431426532286));
#51410=CARTESIAN_POINT('Ctrl Pts',(18.6244919535479,-1.17234924842773,126.461356862258));
#51411=CARTESIAN_POINT('Ctrl Pts',(19.0909970917821,-1.01626672882518,126.491201943604));
#51412=CARTESIAN_POINT('Ctrl Pts',(19.4520665620905,-0.684179402726174,
126.520964546554));
#51413=CARTESIAN_POINT('Ctrl Pts',(19.6454906893739,-0.234786668051046,
126.550647497157));
#51414=CARTESIAN_POINT('Ctrl Pts',(19.6385159835268,0.253149219888882,126.580253676135));
#51415=CARTESIAN_POINT('Ctrl Pts',(19.4333722711128,0.694578566817253,126.609786017081));
#51416=CARTESIAN_POINT('Ctrl Pts',(19.0667063558325,1.01295613554844,126.639247502871));
#51417=CARTESIAN_POINT('Ctrl Pts',(18.6030514946211,1.1534838541102,126.668641164986));
#51418=CARTESIAN_POINT('Ctrl Pts',(18.1234957510667,1.09251755167767,126.697970077986));
#51419=CARTESIAN_POINT('Ctrl Pts',(17.7115308462464,0.841530068193854,126.727237365886));
#51420=CARTESIAN_POINT('Ctrl Pts',(17.4385535098235,0.444964463531077,126.756446186453));
#51421=CARTESIAN_POINT('Ctrl Pts',(17.3515170588706,-0.0276122872710075,
126.785599752877));
#51422=CARTESIAN_POINT('Ctrl Pts',(17.4648884689082,-0.493692017961726,
126.814701285522));
#51423=CARTESIAN_POINT('Ctrl Pts',(17.7582364067503,-0.872180645238306,
126.843754094616));
#51424=CARTESIAN_POINT('Ctrl Pts',(18.1799399597792,-1.09750112430032,126.872761421116));
#51425=CARTESIAN_POINT('Ctrl Pts',(18.6561791423461,-1.13087232076486,126.901726730967));
#51426=CARTESIAN_POINT('Ctrl Pts',(19.1039589342991,-0.967064360638307,
126.930653153623));
#51427=CARTESIAN_POINT('Ctrl Pts',(19.3883902256841,-0.690354148280827,
126.954729317772));
#51428=CARTESIAN_POINT('Ctrl Pts',(19.5332457227074,-0.414056911611768,
126.973973920849));
#51429=CARTESIAN_POINT('Ctrl Pts',(19.6177437769726,-0.113905111418309,
126.993208932229));
#51430=CARTESIAN_POINT('Ctrl Pts',(19.6011038359952,0.281732384417546,127.017234385341));
#51431=CARTESIAN_POINT('Ctrl Pts',(19.3890514321733,0.706565085330299,127.04604027079));
#51432=CARTESIAN_POINT('Ctrl Pts',(19.0223011451343,1.00751421476368,127.074824428941));
#51433=CARTESIAN_POINT('Ctrl Pts',(18.5648792017946,1.13234542273552,127.103590628698));
#51434=CARTESIAN_POINT('Ctrl Pts',(18.0966155583551,1.05950100369092,127.13234222422));
#51435=CARTESIAN_POINT('Ctrl Pts',(17.6990872091144,0.801854248777839,127.161082806753));
#51436=CARTESIAN_POINT('Ctrl Pts',(17.4415305074347,0.404417889894389,127.18981585486));
#51437=CARTESIAN_POINT('Ctrl Pts',(17.3687695530042,-0.0634870235218906,
127.218544916761));
#51438=CARTESIAN_POINT('Ctrl Pts',(17.4934609062107,-0.520295799873725,
127.247273508358));
#51439=CARTESIAN_POINT('Ctrl Pts',(17.7938846953223,-0.886376575644098,
127.276005163098));
#51440=CARTESIAN_POINT('Ctrl Pts',(18.2177247634987,-1.0978765550393,127.304743403475));
#51441=CARTESIAN_POINT('Ctrl Pts',(18.6911508939668,-1.11782834790528,127.333491753923));
#51442=CARTESIAN_POINT('Ctrl Pts',(19.1316465689169,-0.942594483611371,
127.362253727978));
#51443=CARTESIAN_POINT('Ctrl Pts',(19.4623516371648,-0.602527764442204,
127.391032833955));
#51444=CARTESIAN_POINT('Ctrl Pts',(19.6254375334004,-0.156728820867022,
127.419832557726));
#51445=CARTESIAN_POINT('Ctrl Pts',(19.5921943171502,0.317197263638082,127.448656399276));
#51446=CARTESIAN_POINT('Ctrl Pts',(19.368068361135,0.736614311055538,127.477507771776));
#51447=CARTESIAN_POINT('Ctrl Pts',(18.9917822982762,1.02822677014049,127.506390229474));
#51448=CARTESIAN_POINT('Ctrl Pts',(18.5286553795516,1.1408523543525,127.535306988223));
#51449=CARTESIAN_POINT('Ctrl Pts',(18.0593071007243,1.05438854513454,127.564261845145));
#51450=CARTESIAN_POINT('Ctrl Pts',(17.665645179454,0.78337931240486,127.593257348673));
#51451=CARTESIAN_POINT('Ctrl Pts',(17.4166255106301,0.374596672588247,127.622298651964));
#51452=CARTESIAN_POINT('Ctrl Pts',(17.356168808789,-0.10102697056375,127.651385319048));
#51453=CARTESIAN_POINT('Ctrl Pts',(17.4955452283241,-0.560666528004949,
127.680527574784));
#51454=CARTESIAN_POINT('Ctrl Pts',(17.8109503297906,-0.923997881438208,
127.709717292561));
#51455=CARTESIAN_POINT('Ctrl Pts',(18.2483725221223,-1.12713601481138,127.738975362331));
#51456=CARTESIAN_POINT('Ctrl Pts',(18.7311725427411,-1.13411043401417,127.768275574607));
#51457=CARTESIAN_POINT('Ctrl Pts',(19.1762783013378,-0.942422457862223,
127.797675015527));
#51458=CARTESIAN_POINT('Ctrl Pts',(19.5046484170361,-0.585761601815651,
127.827081897376));
#51459=CARTESIAN_POINT('Ctrl Pts',(19.6582495271737,-0.123680562238502,
127.85662756148));
#51460=CARTESIAN_POINT('Ctrl Pts',(19.6201095104048,0.280620801278878,127.881304584504));
#51461=CARTESIAN_POINT('Ctrl Pts',(19.4907597078714,0.572725205601487,127.900977353949));
#51462=CARTESIAN_POINT('Ctrl Pts',(19.3483928135265,0.768967247407983,127.915853796736));
#51463=CARTESIAN_POINT('Ctrl Pts',(19.1686762334047,0.931517072832566,127.930784609013));
#51464=CARTESIAN_POINT('Ctrl Pts',(18.9634686971736,1.051701521621,127.945656286825));
#51465=CARTESIAN_POINT('Ctrl Pts',(18.7395400780403,1.12529086281877,127.960455609962));
#51466=CARTESIAN_POINT('Ctrl Pts',(18.5767277357217,1.14299969027711,127.970442080495));
#51467=CARTESIAN_POINT('Ctrl Pts',(18.491314532458,1.14371857755274,127.975498274504));
#51468=CARTESIAN_POINT('Ctrl Pts',(18.4886857815326,1.24006279342174,112.700349483895));
#51469=CARTESIAN_POINT('Ctrl Pts',(18.350700487512,1.23890142880501,112.7085177809));
#51470=CARTESIAN_POINT('Ctrl Pts',(18.1772861379161,1.21099225659712,112.719338882009));
#51471=CARTESIAN_POINT('Ctrl Pts',(17.9371470941586,1.11768692836503,112.735559070081));
#51472=CARTESIAN_POINT('Ctrl Pts',(17.7502869740318,1.0082123691728,112.749104651932));
#51473=CARTESIAN_POINT('Ctrl Pts',(17.5538963727147,0.830572680386769,112.765421885891));
#51474=CARTESIAN_POINT('Ctrl Pts',(17.3972550616849,0.615007769038441,112.781770658263));
#51475=CARTESIAN_POINT('Ctrl Pts',(17.253907652199,0.291146232712233,112.803582570228));
#51476=CARTESIAN_POINT('Ctrl Pts',(17.2113131548919,-0.157408290328995,
112.830961830784));
#51477=CARTESIAN_POINT('Ctrl Pts',(17.3824904082006,-0.673584584172649,
112.863958155807));
#51478=CARTESIAN_POINT('Ctrl Pts',(17.7519425650394,-1.07558463392321,112.897078373792));
#51479=CARTESIAN_POINT('Ctrl Pts',(18.255676840556,-1.29276968930806,112.930352237627));
#51480=CARTESIAN_POINT('Ctrl Pts',(18.8060692042725,-1.28530683832539,112.963758718116));
#51481=CARTESIAN_POINT('Ctrl Pts',(19.3078619919564,-1.05259089330479,112.997309949318));
#51482=CARTESIAN_POINT('Ctrl Pts',(19.672166717931,-0.633541265410673,113.031000596886));
#51483=CARTESIAN_POINT('Ctrl Pts',(19.8343041249495,-0.0999775951895171,
113.064833380886));
#51484=CARTESIAN_POINT('Ctrl Pts',(19.7640474039292,0.455577886151346,113.09880714741));
#51485=CARTESIAN_POINT('Ctrl Pts',(19.4717972044179,0.935971626992234,113.13292248262));
#51486=CARTESIAN_POINT('Ctrl Pts',(19.0069067899873,1.25642301617407,113.167178934682));
#51487=CARTESIAN_POINT('Ctrl Pts',(18.4493883394344,1.3594620991575,113.201576453895));
#51488=CARTESIAN_POINT('Ctrl Pts',(17.896156579089,1.22525216584098,113.236114632791));
#51489=CARTESIAN_POINT('Ctrl Pts',(17.44416598478,0.875366234347725,113.270793101865));
#51490=CARTESIAN_POINT('Ctrl Pts',(17.1734203958771,0.369351019247229,113.305611329641));
#51491=CARTESIAN_POINT('Ctrl Pts',(17.1328069524393,-0.205403746546834,
113.340568728524));
#51492=CARTESIAN_POINT('Ctrl Pts',(17.3312781873272,-0.748761750970205,
113.375664582924));
#51493=CARTESIAN_POINT('Ctrl Pts',(17.7359495942994,-1.16529115160682,113.410898124736));
#51494=CARTESIAN_POINT('Ctrl Pts',(18.2775596178026,-1.38103864357808,113.44626843028));
#51495=CARTESIAN_POINT('Ctrl Pts',(18.8622737221434,-1.35665630399749,113.48177458993));
#51496=CARTESIAN_POINT('Ctrl Pts',(19.3880357926552,-1.09457855934319,113.517415429957));
#51497=CARTESIAN_POINT('Ctrl Pts',(19.762282781053,-0.63891289156151,113.553189894316));
#51498=CARTESIAN_POINT('Ctrl Pts',(19.9183542097906,-0.0680386023566974,
113.589096658421));
#51499=CARTESIAN_POINT('Ctrl Pts',(19.8273068616531,0.518948612910108,113.62513440713));
#51500=CARTESIAN_POINT('Ctrl Pts',(19.5032854374879,1.01931705204083,113.661301729037));
#51501=CARTESIAN_POINT('Ctrl Pts',(19.0013754975563,1.34488795255941,113.69759704498));
#51502=CARTESIAN_POINT('Ctrl Pts',(18.5070667715635,1.42188430560478,113.727948563529));
#51503=CARTESIAN_POINT('Ctrl Pts',(18.1176199059488,1.35815507053335,113.752292070503));
#51504=CARTESIAN_POINT('Ctrl Pts',(17.7491627514288,1.21499957788935,113.776676870709));
#51505=CARTESIAN_POINT('Ctrl Pts',(17.3596817931078,0.895664735229003,113.807234801998));
#51506=CARTESIAN_POINT('Ctrl Pts',(17.088766042796,0.353119873219169,113.844025336828));
#51507=CARTESIAN_POINT('Ctrl Pts',(17.0629633807845,-0.254681689259876,
113.880935056018));
#51508=CARTESIAN_POINT('Ctrl Pts',(17.2883999286117,-0.821825992495695,
113.917961912365));
#51509=CARTESIAN_POINT('Ctrl Pts',(17.727173455224,-1.24873485756755,113.955103786105));
#51510=CARTESIAN_POINT('Ctrl Pts',(18.303800663237,-1.45983756465867,113.99235852218));
#51511=CARTESIAN_POINT('Ctrl Pts',(18.9181754346717,-1.41687241297771,114.029723858283));
#51512=CARTESIAN_POINT('Ctrl Pts',(19.4629905317816,-1.1258760124666,114.06719743653));
#51513=CARTESIAN_POINT('Ctrl Pts',(19.8424979033294,-0.636345183090518,
114.10477690674));
#51514=CARTESIAN_POINT('Ctrl Pts',(19.9893577348222,-0.0328548365392322,
114.142459719485));
#51515=CARTESIAN_POINT('Ctrl Pts',(19.8766107184348,0.579636771896997,114.180243394414));
#51516=CARTESIAN_POINT('Ctrl Pts',(19.5226143125954,1.09396896256936,114.218125277347));
#51517=CARTESIAN_POINT('Ctrl Pts',(18.9880576434996,1.4196814246808,114.256102695897));
#51518=CARTESIAN_POINT('Ctrl Pts',(18.3655758455969,1.49883229295896,114.294172904322));
#51519=CARTESIAN_POINT('Ctrl Pts',(17.7636357733795,1.31639721669226,114.332333090623));
#51520=CARTESIAN_POINT('Ctrl Pts',(17.2876293894219,0.903070126436221,114.370580382322));
#51521=CARTESIAN_POINT('Ctrl Pts',(17.021381596707,0.330105442854477,114.408911856729));
#51522=CARTESIAN_POINT('Ctrl Pts',(17.0123615413044,-0.302963995370305,
114.447324511126));
#51523=CARTESIAN_POINT('Ctrl Pts',(17.2632246426998,-0.885701130781865,
114.485815331495));
#51524=CARTESIAN_POINT('Ctrl Pts',(17.7311221924098,-1.31595137471215,114.524381167031));
#51525=CARTESIAN_POINT('Ctrl Pts',(18.3351011606019,-1.51799826919431,114.563018976257));
#51526=CARTESIAN_POINT('Ctrl Pts',(18.8641772955744,-1.46590872316032,114.595274296623));
#51527=CARTESIAN_POINT('Ctrl Pts',(19.2475290597062,-1.29717065284742,114.621111390481));
#51528=CARTESIAN_POINT('Ctrl Pts',(19.587930934106,-1.05255012654514,114.646969774733));
#51529=CARTESIAN_POINT('Ctrl Pts',(19.9027887485453,-0.622010716970455,
114.679331455281));
#51530=CARTESIAN_POINT('Ctrl Pts',(20.0367268988523,0.00492783437249169,
114.718224488104));
#51531=CARTESIAN_POINT('Ctrl Pts',(19.902771949599,0.632745745648799,114.757172921015));
#51532=CARTESIAN_POINT('Ctrl Pts',(19.5235337266645,1.1518069086034,114.796173482906));
#51533=CARTESIAN_POINT('Ctrl Pts',(18.9646746735623,1.47107637085436,114.835222648074));
#51534=CARTESIAN_POINT('Ctrl Pts',(18.3234147425032,1.53431878643646,114.874317010436));
#51535=CARTESIAN_POINT('Ctrl Pts',(17.7115872791309,1.32988381647799,114.913452982608));
#51536=CARTESIAN_POINT('Ctrl Pts',(17.236199074676,0.892983590472233,114.95262716011));
#51537=CARTESIAN_POINT('Ctrl Pts',(16.9804303870928,0.299434632784239,114.991835755524));
#51538=CARTESIAN_POINT('Ctrl Pts',(16.9885500629826,-0.275357498986949,
115.026715644867));
#51539=CARTESIAN_POINT('Ctrl Pts',(17.1661753238746,-0.739792594872671,
115.057252816654));
#51540=CARTESIAN_POINT('Ctrl Pts',(17.3582591195826,-0.995315857598361,
115.076892896405));
#51541=CARTESIAN_POINT('Ctrl Pts',(17.5129117285239,-1.1393035260029,115.089988598705));
#51542=CARTESIAN_POINT('Ctrl Pts',(17.5949882602575,-1.20577477857244,115.096537396983));
#51543=CARTESIAN_POINT('Ctrl Pts',(17.6816102396563,-1.2662793811424,115.103086599594));
#51544=CARTESIAN_POINT('Ctrl Pts',(17.8628170287837,-1.37497559618221,115.116186841398));
#51545=CARTESIAN_POINT('Ctrl Pts',(18.1617769542351,-1.48907715427518,115.135839934973));
#51546=CARTESIAN_POINT('Ctrl Pts',(18.5869931130475,-1.52497006090699,115.162053457002));
#51547=CARTESIAN_POINT('Ctrl Pts',(19.0057443231637,-1.44168146613633,115.188272628449));
#51548=CARTESIAN_POINT('Ctrl Pts',(19.3849508796851,-1.2457392947455,115.214498469562));
#51549=CARTESIAN_POINT('Ctrl Pts',(19.6955043477239,-0.952325970828538,
115.240728071787));
#51550=CARTESIAN_POINT('Ctrl Pts',(19.9120727588161,-0.58453124815665,115.266961861401));
#51551=CARTESIAN_POINT('Ctrl Pts',(20.0554335071329,-0.0328780904536275,
115.30194294116));
#51552=CARTESIAN_POINT('Ctrl Pts',(19.9573549390358,0.544872472127717,115.336926751788));
#51553=CARTESIAN_POINT('Ctrl Pts',(19.6792725553991,0.959018990798004,115.367536446853));
#51554=CARTESIAN_POINT('Ctrl Pts',(19.4770068532755,1.15607677108951,115.385026263675));
#51555=CARTESIAN_POINT('Ctrl Pts',(19.2485905147621,1.32287773637073,115.402515663463));
#51556=CARTESIAN_POINT('Ctrl Pts',(19.0214001924108,1.42466933279182,115.417817762452));
#51557=CARTESIAN_POINT('Ctrl Pts',(18.8160770510847,1.47600201291175,115.430931956767));
#51558=CARTESIAN_POINT('Ctrl Pts',(18.7119660101375,1.49445958327978,115.437488986517));
#51559=CARTESIAN_POINT('Ctrl Pts',(18.6243012018012,1.50374532227516,115.442952840385));
#51560=CARTESIAN_POINT('Ctrl Pts',(18.5539105066717,1.50738308247896,115.44732397057));
#51561=CARTESIAN_POINT('Ctrl Pts',(18.2682087517811,1.51284780011209,115.465050305463));
#51562=CARTESIAN_POINT('Ctrl Pts',(17.7497170731845,1.38044204374156,115.497218908285));
#51563=CARTESIAN_POINT('Ctrl Pts',(17.30801070384,0.970768685607363,115.53345638968));
#51564=CARTESIAN_POINT('Ctrl Pts',(17.1114916776926,0.601056660964444,115.559330092168));
#51565=CARTESIAN_POINT('Ctrl Pts',(17.0446027454294,0.402885159945071,115.572263924207));
#51566=CARTESIAN_POINT('Ctrl Pts',(17.0117248103742,0.239205340866807,115.582609001927));
#51567=CARTESIAN_POINT('Ctrl Pts',(16.9724616627671,-0.0923162242471636,
115.60329739301));
#51568=CARTESIAN_POINT('Ctrl Pts',(17.0696480425108,-0.642532402723225,
115.636900798108));
#51569=CARTESIAN_POINT('Ctrl Pts',(17.5517663934372,-1.24713786909881,115.683388146918));
#51570=CARTESIAN_POINT('Ctrl Pts',(18.2042007282122,-1.5217813743094,115.725958665169));
#51571=CARTESIAN_POINT('Ctrl Pts',(18.8381530262514,-1.49751551729433,115.764620805466));
#51572=CARTESIAN_POINT('Ctrl Pts',(19.3608147157338,-1.26964475423224,115.799384658136));
#51573=CARTESIAN_POINT('Ctrl Pts',(19.7637360954163,-0.866573811032385,
115.834113791312));
#51574=CARTESIAN_POINT('Ctrl Pts',(19.9532575329137,-0.431912285220216,
115.863024225621));
#51575=CARTESIAN_POINT('Ctrl Pts',(20.0019084566828,-0.0608512365984601,
115.886132317853));
#51576=CARTESIAN_POINT('Ctrl Pts',(19.9862463403857,0.219126166715986,115.903454009194));
#51577=CARTESIAN_POINT('Ctrl Pts',(19.9299939358539,0.44586883885173,115.917879168524));
#51578=CARTESIAN_POINT('Ctrl Pts',(19.8603226080054,0.618480030546314,115.929414262885));
#51579=CARTESIAN_POINT('Ctrl Pts',(19.732335428513,0.866591475554719,115.946711763469));
#51580=CARTESIAN_POINT('Ctrl Pts',(19.4548716729342,1.1889197996581,115.972636463467));
#51581=CARTESIAN_POINT('Ctrl Pts',(18.9541280189803,1.45349838246967,116.007156800886));
#51582=CARTESIAN_POINT('Ctrl Pts',(18.3921287206258,1.51673596305252,116.041627931309));
#51583=CARTESIAN_POINT('Ctrl Pts',(17.98308129254,1.40706783893502,116.06744280953));
#51584=CARTESIAN_POINT('Ctrl Pts',(17.7390445958302,1.2749731316633,116.084636072118));
#51585=CARTESIAN_POINT('Ctrl Pts',(17.5852912916948,1.1722752978984,116.096093986087));
#51586=CARTESIAN_POINT('Ctrl Pts',(17.3432828327208,0.956086398655082,116.116132394891));
#51587=CARTESIAN_POINT('Ctrl Pts',(17.1809589926931,0.698076633103147,116.134717679963));
#51588=CARTESIAN_POINT('Ctrl Pts',(17.1020431840008,0.481651667190302,116.149000182525));
#51589=CARTESIAN_POINT('Ctrl Pts',(17.0813292455805,0.415767578672489,116.153283932293));
#51590=CARTESIAN_POINT('Ctrl Pts',(17.0637859639785,0.348956125741941,116.157566823568));
#51591=CARTESIAN_POINT('Ctrl Pts',(17.0493670996022,0.281437463958633,116.16184876527));
#51592=CARTESIAN_POINT('Ctrl Pts',(17.038100686667,0.213320935068083,116.166129828349));
#51593=CARTESIAN_POINT('Ctrl Pts',(17.027418537701,0.121921946398209,116.171836683298));
#51594=CARTESIAN_POINT('Ctrl Pts',(17.0154022607627,-0.131006355748056,
116.187525750009));
#51595=CARTESIAN_POINT('Ctrl Pts',(17.0937079736478,-0.544356912453348,
116.213169665427));
#51596=CARTESIAN_POINT('Ctrl Pts',(17.3916931786148,-1.01842990090603,116.247299944086));
#51597=CARTESIAN_POINT('Ctrl Pts',(17.8414160362638,-1.35021757910078,116.281365294444));
#51598=CARTESIAN_POINT('Ctrl Pts',(18.38024698509,-1.49448019673828,116.315364296159));
#51599=CARTESIAN_POINT('Ctrl Pts',(18.9333558500912,-1.43205814835875,116.349294475226));
#51600=CARTESIAN_POINT('Ctrl Pts',(19.4244998765879,-1.17237925887462,116.383154182635));
#51601=CARTESIAN_POINT('Ctrl Pts',(19.7055325005771,-0.845552308419617,
116.409432645791));
#51602=CARTESIAN_POINT('Ctrl Pts',(19.8402281106805,-0.574341496855494,
116.428175851723));
#51603=CARTESIAN_POINT('Ctrl Pts',(19.9200054022093,-0.345954669915418,
116.443158705062));
#51604=CARTESIAN_POINT('Ctrl Pts',(19.9840539280259,0.0748890717238647,
116.469349942729));
#51605=CARTESIAN_POINT('Ctrl Pts',(19.8458498456958,0.679996931929124,116.506679814718));
#51606=CARTESIAN_POINT('Ctrl Pts',(19.3540620896253,1.23670047743049,116.55133441875));
#51607=CARTESIAN_POINT('Ctrl Pts',(18.6584618742995,1.48956129229607,116.595843150702));
#51608=CARTESIAN_POINT('Ctrl Pts',(17.9289213122935,1.37932213376007,116.640202113418));
#51609=CARTESIAN_POINT('Ctrl Pts',(17.4285805916008,0.999858721838042,116.677960635258));
#51610=CARTESIAN_POINT('Ctrl Pts',(17.1711328116473,0.561567611548129,116.709185478337));
#51611=CARTESIAN_POINT('Ctrl Pts',(17.0359126623898,0.0415724183980224,
116.74217956973));
#51612=CARTESIAN_POINT('Ctrl Pts',(17.1515940470276,-0.637998239122351,
116.783294411513));
#51613=CARTESIAN_POINT('Ctrl Pts',(17.7010550860578,-1.25205133614912,116.832422554598));
#51614=CARTESIAN_POINT('Ctrl Pts',(18.4894062498268,-1.47858967259486,116.881336428698));
#51615=CARTESIAN_POINT('Ctrl Pts',(19.2738940695048,-1.25207829303643,116.9300315906));
#51616=CARTESIAN_POINT('Ctrl Pts',(19.8153307145306,-0.645520014193124,
116.978503807804));
#51617=CARTESIAN_POINT('Ctrl Pts',(19.9274909343049,0.0191068948937147,
117.018708427583));
#51618=CARTESIAN_POINT('Ctrl Pts',(19.7960939552228,0.52415495559139,117.050756767602));
#51619=CARTESIAN_POINT('Ctrl Pts',(19.5981826748897,0.860577176378632,117.074735160752));
#51620=CARTESIAN_POINT('Ctrl Pts',(19.314819314541,1.1276909269993,117.09865491716));
#51621=CARTESIAN_POINT('Ctrl Pts',(18.8549396626615,1.36629811978027,117.130469699018));
#51622=CARTESIAN_POINT('Ctrl Pts',(18.1917040784683,1.40331982158644,117.170090005227));
#51623=CARTESIAN_POINT('Ctrl Pts',(17.4975691912014,1.01895490957414,117.217394838748));
#51624=CARTESIAN_POINT('Ctrl Pts',(17.1163543952753,0.327987168551171,117.264457516944));
#51625=CARTESIAN_POINT('Ctrl Pts',(17.160929761522,-0.455921789738659,117.311275902367));
#51626=CARTESIAN_POINT('Ctrl Pts',(17.6133690361685,-1.0925258757231,117.357848055034));
#51627=CARTESIAN_POINT('Ctrl Pts',(18.3313062938161,-1.38928284881341,117.404172384602));
#51628=CARTESIAN_POINT('Ctrl Pts',(19.0929708141868,-1.25926708655467,117.450247571127));
#51629=CARTESIAN_POINT('Ctrl Pts',(19.6655860734287,-0.746753373827336,
117.496072609338));
#51630=CARTESIAN_POINT('Ctrl Pts',(19.8765949471167,-0.0121828500468043,
117.54164678921));
#51631=CARTESIAN_POINT('Ctrl Pts',(19.6656116013329,0.718007452175992,117.586969706763));
#51632=CARTESIAN_POINT('Ctrl Pts',(19.1016254377219,1.22121959599358,117.632041258556));
#51633=CARTESIAN_POINT('Ctrl Pts',(18.3605130926681,1.34653801701873,117.676861646409));
#51634=CARTESIAN_POINT('Ctrl Pts',(17.6702033501949,1.05996166417369,117.721431373627));
#51635=CARTESIAN_POINT('Ctrl Pts',(17.2405952007114,0.453464700753241,117.765751245736));
#51636=CARTESIAN_POINT('Ctrl Pts',(17.1997363628675,-0.284476148782968,
117.809822372049));
#51637=CARTESIAN_POINT('Ctrl Pts',(17.5557499811275,-0.927408650891648,
117.853646158814));
#51638=CARTESIAN_POINT('Ctrl Pts',(18.1956275936224,-1.28041361919324,117.897224312267));
#51639=CARTESIAN_POINT('Ctrl Pts',(18.921197736518,-1.23907672512662,117.940558832347));
#51640=CARTESIAN_POINT('Ctrl Pts',(19.5101916907598,-0.820458777550031,
117.983652023246));
#51641=CARTESIAN_POINT('Ctrl Pts',(19.7848036770107,-0.156223199417709,
118.026506456872));
#51642=CARTESIAN_POINT('Ctrl Pts',(19.6843949739844,0.430767380595849,118.062021937999));
#51643=CARTESIAN_POINT('Ctrl Pts',(19.4275325513615,0.813160885753741,118.09031793704));
#51644=CARTESIAN_POINT('Ctrl Pts',(19.0770973083296,1.11031666639859,118.11853700952));
#51645=CARTESIAN_POINT('Ctrl Pts',(18.5109814174046,1.27316147481377,118.153667438987));
#51646=CARTESIAN_POINT('Ctrl Pts',(17.8353641889859,1.07788215725043,118.195598493365));
#51647=CARTESIAN_POINT('Ctrl Pts',(17.3697015237894,0.556044035321663,118.237307932148));
#51648=CARTESIAN_POINT('Ctrl Pts',(17.2536309754749,-0.13005972066861,118.278800089396));
#51649=CARTESIAN_POINT('Ctrl Pts',(17.519011887563,-0.76940485670393,118.320079435902));
#51650=CARTESIAN_POINT('Ctrl Pts',(18.0810167923109,-1.16759070881662,118.361150774145));
#51651=CARTESIAN_POINT('Ctrl Pts',(18.7653205420581,-1.20552740953108,118.402019112245));
#51652=CARTESIAN_POINT('Ctrl Pts',(19.3620426768933,-0.875236261419451,
118.44268974516));
#51653=CARTESIAN_POINT('Ctrl Pts',(19.6899929427312,-0.280852314250413,
118.483168136373));
#51654=CARTESIAN_POINT('Ctrl Pts',(19.6517027034045,0.393658905744708,118.523460105995));
#51655=CARTESIAN_POINT('Ctrl Pts',(19.262049671239,0.94218480231557,118.563571483349));
#51656=CARTESIAN_POINT('Ctrl Pts',(18.7464141286224,1.15520066927372,118.596852495218));
#51657=CARTESIAN_POINT('Ctrl Pts',(18.3143388197521,1.14217861007577,118.623393153417));
#51658=CARTESIAN_POINT('Ctrl Pts',(18.0062641848802,1.04426592123211,118.643257711825));
#51659=CARTESIAN_POINT('Ctrl Pts',(17.737911282933,0.864729841538294,118.663081671285));
#51660=CARTESIAN_POINT('Ctrl Pts',(17.5301393468996,0.618703669685291,118.682866420824));
#51661=CARTESIAN_POINT('Ctrl Pts',(17.39886715547,0.325178671794981,118.702612273734));
#51662=CARTESIAN_POINT('Ctrl Pts',(17.3540635143272,0.00751232992213948,
118.722320588503));
#51663=CARTESIAN_POINT('Ctrl Pts',(17.3988571968852,-0.309665669008213,
118.741991793837));
#51664=CARTESIAN_POINT('Ctrl Pts',(17.5077328986331,-0.552719890765469,
118.758354742027));
#51665=CARTESIAN_POINT('Ctrl Pts',(17.6323989098259,-0.723375778033712,
118.77142712254));
#51666=CARTESIAN_POINT('Ctrl Pts',(17.7796050666785,-0.874496856491821,
118.784488585854));
#51667=CARTESIAN_POINT('Ctrl Pts',(18.0883757023863,-1.0816829350278,118.807315342415));
#51668=CARTESIAN_POINT('Ctrl Pts',(18.6258850389041,-1.17297338013441,118.839842374316));
#51669=CARTESIAN_POINT('Ctrl Pts',(19.2288585553104,-0.922879583318754,
118.878749049984));
#51670=CARTESIAN_POINT('Ctrl Pts',(19.542020048084,-0.480800009490288,118.911072799632));
#51671=CARTESIAN_POINT('Ctrl Pts',(19.6130019723937,-0.11988951021874,118.933651657005));
#51672=CARTESIAN_POINT('Ctrl Pts',(19.6102239348255,0.0882078318904775,
118.946540021196));
#51673=CARTESIAN_POINT('Ctrl Pts',(19.5782633862719,0.294095923696726,118.959420392155));
#51674=CARTESIAN_POINT('Ctrl Pts',(19.4847100541208,0.538407016934738,118.975504309447));
#51675=CARTESIAN_POINT('Ctrl Pts',(19.2335825206301,0.873421396581657,119.001206235821));
#51676=CARTESIAN_POINT('Ctrl Pts',(18.7630625129791,1.133423759209,119.033274471397));
#51677=CARTESIAN_POINT('Ctrl Pts',(18.1200833960856,1.09710962449598,119.071670495069));
#51678=CARTESIAN_POINT('Ctrl Pts',(17.5960924873024,0.725093259873059,119.109988487022));
#51679=CARTESIAN_POINT('Ctrl Pts',(17.3918121525979,0.231296298510037,119.14186251893));
#51680=CARTESIAN_POINT('Ctrl Pts',(17.4043290798831,-0.183311036107097,
119.167330765526));
#51681=CARTESIAN_POINT('Ctrl Pts',(17.4825892496997,-0.4299892222351,119.183237212406));
#51682=CARTESIAN_POINT('Ctrl Pts',(17.572039140911,-0.586160414573573,119.194365338264));
#51683=CARTESIAN_POINT('Ctrl Pts',(17.6318745222132,-0.669372754950965,
119.200722868091));
#51684=CARTESIAN_POINT('Ctrl Pts',(17.6975224916197,-0.748188779439941,
119.207079373284));
#51685=CARTESIAN_POINT('Ctrl Pts',(17.7895488799981,-0.837670708203213,
119.215023530388));
#51686=CARTESIAN_POINT('Ctrl Pts',(17.9553267231429,-0.958868977804718,
119.227729237297));
#51687=CARTESIAN_POINT('Ctrl Pts',(18.1912383187694,-1.06444361121362,119.243605397494));
#51688=CARTESIAN_POINT('Ctrl Pts',(18.4982090921703,-1.10776721271402,119.262646233441));
#51689=CARTESIAN_POINT('Ctrl Pts',(18.80502032819,-1.06443802417128,119.281678727518));
#51690=CARTESIAN_POINT('Ctrl Pts',(19.0877383109047,-0.937929437452661,
119.300703044015));
#51691=CARTESIAN_POINT('Ctrl Pts',(19.3242981547535,-0.738152546180218,
119.319721102764));
#51692=CARTESIAN_POINT('Ctrl Pts',(19.4962591468119,-0.480795071701003,
119.338732993694));
#51693=CARTESIAN_POINT('Ctrl Pts',(19.5902349861746,-0.185930364314395,
119.357741177416));
#51694=CARTESIAN_POINT('Ctrl Pts',(19.5988995449809,0.12332837974993,119.376744922794));
#51695=CARTESIAN_POINT('Ctrl Pts',(19.5345226003805,0.372995262793573,119.392580513945));
#51696=CARTESIAN_POINT('Ctrl Pts',(19.4430256832353,0.556105224782065,119.405247530558));
#51697=CARTESIAN_POINT('Ctrl Pts',(19.2980649158877,0.766998982846697,119.421081592547));
#51698=CARTESIAN_POINT('Ctrl Pts',(19.0156700351553,0.998794457158363,119.44324895863));
#51699=CARTESIAN_POINT('Ctrl Pts',(18.5624053105446,1.12252034366067,119.47175321809));
#51700=CARTESIAN_POINT('Ctrl Pts',(18.0980570899233,1.05032299384497,119.500264531386));
#51701=CARTESIAN_POINT('Ctrl Pts',(17.7035292914276,0.79466914998275,119.528786584334));
#51702=CARTESIAN_POINT('Ctrl Pts',(17.447699261081,0.399967002624156,119.557322986304));
#51703=CARTESIAN_POINT('Ctrl Pts',(17.3753531548392,-0.0650758120843595,
119.585877532102));
#51704=CARTESIAN_POINT('Ctrl Pts',(17.4993233063343,-0.519496847790021,
119.614453598271));
#51705=CARTESIAN_POINT('Ctrl Pts',(17.7485568416745,-0.82315833221159,119.638288394535));
#51706=CARTESIAN_POINT('Ctrl Pts',(18.0094705396139,-0.989327736740765,
119.657370307388));
#51707=CARTESIAN_POINT('Ctrl Pts',(18.2992856072175,-1.09795570141558,119.676462853576));
#51708=CARTESIAN_POINT('Ctrl Pts',(18.6926161209824,-1.11462209520415,119.700348615935));
#51709=CARTESIAN_POINT('Ctrl Pts',(19.132174381934,-0.939774985844624,119.729047762112));
#51710=CARTESIAN_POINT('Ctrl Pts',(19.4624379375494,-0.600228903798103,
119.757786510277));
#51711=CARTESIAN_POINT('Ctrl Pts',(19.6254642184456,-0.154710493808823,
119.786568470845));
#51712=CARTESIAN_POINT('Ctrl Pts',(19.5922506981539,0.319294076080361,119.815397085605));
#51713=CARTESIAN_POINT('Ctrl Pts',(19.3679519164038,0.739126592198824,119.844275847045));
#51714=CARTESIAN_POINT('Ctrl Pts',(18.9910313338467,1.03127863586338,119.873208155992));
#51715=CARTESIAN_POINT('Ctrl Pts',(18.526768166279,1.1442132821202,119.902197433971));
#51716=CARTESIAN_POINT('Ctrl Pts',(18.0558482748031,1.05752607607186,119.931246981343));
#51717=CARTESIAN_POINT('Ctrl Pts',(17.726496041802,0.830759475988353,119.955507997517));
#51718=CARTESIAN_POINT('Ctrl Pts',(17.5354344117903,0.580091248025318,119.974950233318));
#51719=CARTESIAN_POINT('Ctrl Pts',(17.4002338592083,0.29498975660088,119.994415199709));
#51720=CARTESIAN_POINT('Ctrl Pts',(17.3495085645331,-0.103555383199835,
120.018790389193));
#51721=CARTESIAN_POINT('Ctrl Pts',(17.4897005229253,-0.566111876871723,
120.048113816961));
#51722=CARTESIAN_POINT('Ctrl Pts',(17.8073958110046,-0.932013831621567,
120.077513669291));
#51723=CARTESIAN_POINT('Ctrl Pts',(18.2480282367772,-1.13680697021833,120.106992966317));
#51724=CARTESIAN_POINT('Ctrl Pts',(18.7352313285216,-1.14378430035558,120.136554771527));
#51725=CARTESIAN_POINT('Ctrl Pts',(19.1840902814294,-0.950608003668691,
120.1662020226));
#51726=CARTESIAN_POINT('Ctrl Pts',(19.5158873892962,-0.589875672534864,
120.195937638644));
#51727=CARTESIAN_POINT('Ctrl Pts',(19.671889057115,-0.123661189251937,120.22576445635));
#51728=CARTESIAN_POINT('Ctrl Pts',(19.623714661444,0.367152098317012,120.255685262371));
#51729=CARTESIAN_POINT('Ctrl Pts',(19.3784858113755,0.796867932693748,120.285702774258));
#51730=CARTESIAN_POINT('Ctrl Pts',(18.9778103881022,1.08991323854088,120.315819647296));
#51731=CARTESIAN_POINT('Ctrl Pts',(18.490745518226,1.19410168075579,120.346038467292));
#51732=CARTESIAN_POINT('Ctrl Pts',(18.0019208947732,1.0899089270007,120.376361751047));
#51733=CARTESIAN_POINT('Ctrl Pts',(17.5968617879682,0.794109542044404,120.406791944027));
#51734=CARTESIAN_POINT('Ctrl Pts',(17.347051270975,0.357102672662465,120.437331420421));
#51735=CARTESIAN_POINT('Ctrl Pts',(17.2973371287444,-0.145653526217233,
120.467982479992));
#51736=CARTESIAN_POINT('Ctrl Pts',(17.4578978561675,-0.626646770663367,
120.498747346768));
#51737=CARTESIAN_POINT('Ctrl Pts',(17.8022046733259,-1.00151876106162,120.529628166802));
#51738=CARTESIAN_POINT('Ctrl Pts',(18.2713816533395,-1.2038382914039,120.56062700755));
#51739=CARTESIAN_POINT('Ctrl Pts',(18.7842526924098,-1.19685517031873,120.591745857205));
#51740=CARTESIAN_POINT('Ctrl Pts',(19.2513645194326,-0.980158514937333,
120.622986622443));
#51741=CARTESIAN_POINT('Ctrl Pts',(19.5905678372684,-0.590034427104998,
120.654351127325));
#51742=CARTESIAN_POINT('Ctrl Pts',(19.7414461342557,-0.0934120172357776,
120.685841110659));
#51743=CARTESIAN_POINT('Ctrl Pts',(19.6760617503497,0.423601688996781,120.71745822783));
#51744=CARTESIAN_POINT('Ctrl Pts',(19.404107616491,0.870629407224791,120.749204045237));
#51745=CARTESIAN_POINT('Ctrl Pts',(18.9715208516985,1.16881187603194,120.781080048323));
#51746=CARTESIAN_POINT('Ctrl Pts',(18.4527393308266,1.26469201462238,120.813087622212));
#51747=CARTESIAN_POINT('Ctrl Pts',(17.9379142663286,1.13980835377827,120.845228084342));
#51748=CARTESIAN_POINT('Ctrl Pts',(17.5172493454425,0.814174010463595,120.877502620948));
#51749=CARTESIAN_POINT('Ctrl Pts',(17.2652262451152,0.343182535559932,120.909912404771));
#51750=CARTESIAN_POINT('Ctrl Pts',(17.2273959740802,-0.191955731854894,
120.942458370174));
#51751=CARTESIAN_POINT('Ctrl Pts',(17.3660099011979,-0.571412507180306,
120.966970834626));
#51752=CARTESIAN_POINT('Ctrl Pts',(17.5184864903043,-0.787587395398978,
120.983355475166));
#51753=CARTESIAN_POINT('Ctrl Pts',(17.6347010321129,-0.920420644721155,
120.994290222211));
#51754=CARTESIAN_POINT('Ctrl Pts',(17.8733381436317,-1.11944341903204,121.013456130434));
#51755=CARTESIAN_POINT('Ctrl Pts',(18.2938200015906,-1.28705511872534,121.040922810645));
#51756=CARTESIAN_POINT('Ctrl Pts',(18.838962756471,-1.26431650933352,121.074022238662));
#51757=CARTESIAN_POINT('Ctrl Pts',(19.3292777630611,-1.01994040665058,121.107261676011));
#51758=CARTESIAN_POINT('Ctrl Pts',(19.6785157529131,-0.594786234672817,
121.140641575335));
#51759=CARTESIAN_POINT('Ctrl Pts',(19.8242377305752,-0.061848242086873,
121.174162316278));
#51760=CARTESIAN_POINT('Ctrl Pts',(19.7392267053303,0.486436575583768,121.20782417147));
#51761=CARTESIAN_POINT('Ctrl Pts',(19.4364151393894,0.954128542250682,121.241627324197));
#51762=CARTESIAN_POINT('Ctrl Pts',(18.9670347240106,1.25861868234264,121.275571858454));
#51763=CARTESIAN_POINT('Ctrl Pts',(18.4119209874691,1.3451928655867,121.309657764006));
#51764=CARTESIAN_POINT('Ctrl Pts',(17.8676162900118,1.19687069039815,121.34388493345));
#51765=CARTESIAN_POINT('Ctrl Pts',(17.4295680364872,0.837690818648143,121.378253164648));
#51766=CARTESIAN_POINT('Ctrl Pts',(17.1753947118292,0.328842988621187,121.412762158879));
#51767=CARTESIAN_POINT('Ctrl Pts',(17.1511288723051,-0.241752018640547,
121.447411523291));
#51768=CARTESIAN_POINT('Ctrl Pts',(17.3628888947757,-0.77463506048684,121.482200766943));
#51769=CARTESIAN_POINT('Ctrl Pts',(17.7754799049959,-1.17614877543075,121.517129308824));
#51770=CARTESIAN_POINT('Ctrl Pts',(18.3182280438042,-1.37490813354109,121.552196464719));
#51771=CARTESIAN_POINT('Ctrl Pts',(18.897088341648,-1.33448709779315,121.587401473303));
#51772=CARTESIAN_POINT('Ctrl Pts',(19.410942275329,-1.06009788899736,121.622743447905));
#51773=CARTESIAN_POINT('Ctrl Pts',(19.7692799982594,-0.597977854521384,
121.658221467788));
#51774=CARTESIAN_POINT('Ctrl Pts',(19.9081358825043,-0.0276549104963941,
121.693834408962));
#51775=CARTESIAN_POINT('Ctrl Pts',(19.8015290711147,0.551829178738792,121.729581235412));
#51776=CARTESIAN_POINT('Ctrl Pts',(19.4663014352217,1.03901557989597,121.765460617446));
#51777=CARTESIAN_POINT('Ctrl Pts',(18.9594683704855,1.34791861935948,121.801471275704));
#51778=CARTESIAN_POINT('Ctrl Pts',(18.3685489456073,1.4231309693145,121.837611797694));
#51779=CARTESIAN_POINT('Ctrl Pts',(17.7964224040695,1.2498108864466,121.873880663349));
#51780=CARTESIAN_POINT('Ctrl Pts',(17.343411761646,0.856551976471352,121.910276301795));
#51781=CARTESIAN_POINT('Ctrl Pts',(17.0896693094759,0.310691435299757,121.946797039564));
#51782=CARTESIAN_POINT('Ctrl Pts',(17.0809859345148,-0.293233463282239,
121.983441096799));
#51783=CARTESIAN_POINT('Ctrl Pts',(17.3205246799805,-0.849870499306589,
122.020206666278));
#51784=CARTESIAN_POINT('Ctrl Pts',(17.7679800867644,-1.26145256297933,122.057091786186));
#51785=CARTESIAN_POINT('Ctrl Pts',(18.3463570362798,-1.45498776189057,122.09409447297));
#51786=CARTESIAN_POINT('Ctrl Pts',(18.9552323067948,-1.39521898177386,122.131212644739));
#51787=CARTESIAN_POINT('Ctrl Pts',(19.4882105420212,-1.09104109063806,122.16844410693));
#51788=CARTESIAN_POINT('Ctrl Pts',(19.8515424108103,-0.594221675970028,
122.205786668318));
#51789=CARTESIAN_POINT('Ctrl Pts',(19.9806313833143,0.00942427040184544,
122.24323795134));
#51790=CARTESIAN_POINT('Ctrl Pts',(19.8515388043119,0.614855844550354,122.280795635654));
#51791=CARTESIAN_POINT('Ctrl Pts',(19.4853987313484,1.11614759069681,122.318457157599));
#51792=CARTESIAN_POINT('Ctrl Pts',(18.945004615623,1.42498917337475,122.356220138897));
#51793=CARTESIAN_POINT('Ctrl Pts',(18.3239615977549,1.48632115394554,122.394081816335));
#51794=CARTESIAN_POINT('Ctrl Pts',(17.730540856481,1.28815607788699,122.43203962541));
#51795=CARTESIAN_POINT('Ctrl Pts',(17.2686808444291,0.863809782588366,122.470090788431));
#51796=CARTESIAN_POINT('Ctrl Pts',(17.0198424256365,0.286534217812077,122.508232510253));
#51797=CARTESIAN_POINT('Ctrl Pts',(17.0275509599641,-0.273612269369176,
122.542214254841));
#51798=CARTESIAN_POINT('Ctrl Pts',(17.200985856733,-0.726414318936751,122.572003192732));
#51799=CARTESIAN_POINT('Ctrl Pts',(17.533930302551,-1.17071941096088,122.60609683765));
#51800=CARTESIAN_POINT('Ctrl Pts',(18.1603244553639,-1.51749147705401,122.648803589497));
#51801=CARTESIAN_POINT('Ctrl Pts',(19.0208668383675,-1.4694521284666,122.700188190209));
#51802=CARTESIAN_POINT('Ctrl Pts',(19.7255038627886,-0.969775365785065,
122.751701753606));
#51803=CARTESIAN_POINT('Ctrl Pts',(20.057165664497,-0.169954192248215,122.803336782717));
#51804=CARTESIAN_POINT('Ctrl Pts',(19.9120558026029,0.685817564794368,122.855085508656));
#51805=CARTESIAN_POINT('Ctrl Pts',(19.4292974339625,1.22598318348634,122.898297694433));
#51806=CARTESIAN_POINT('Ctrl Pts',(18.9142363313226,1.45527724361131,122.932916381728));
#51807=CARTESIAN_POINT('Ctrl Pts',(18.5110045428195,1.51276370728313,122.957941335571));
#51808=CARTESIAN_POINT('Ctrl Pts',(18.1227813242447,1.46364271968411,122.982023454891));
#51809=CARTESIAN_POINT('Ctrl Pts',(17.6559380408361,1.28127618901461,123.01287122073));
#51810=CARTESIAN_POINT('Ctrl Pts',(17.1851908013954,0.844766685164182,123.05147176177));
#51811=CARTESIAN_POINT('Ctrl Pts',(16.9804906029009,0.235476790658082,123.090121547379));
#51812=CARTESIAN_POINT('Ctrl Pts',(17.0063897534652,-0.266692007359343,
123.121068363773));
#51813=CARTESIAN_POINT('Ctrl Pts',(17.1538193871115,-0.747580694334549,
123.152031740723));
#51814=CARTESIAN_POINT('Ctrl Pts',(17.5553447104498,-1.25148896205411,123.190765979047));
#51815=CARTESIAN_POINT('Ctrl Pts',(18.2089111413414,-1.52674514579364,123.233411566373));
#51816=CARTESIAN_POINT('Ctrl Pts',(18.845013323169,-1.50249908902663,123.272206310198));
#51817=CARTESIAN_POINT('Ctrl Pts',(19.3702773407149,-1.27357787369309,123.307138988368));
#51818=CARTESIAN_POINT('Ctrl Pts',(19.7757310421874,-0.868041960323205,
123.342086539292));
#51819=CARTESIAN_POINT('Ctrl Pts',(20.0050916775235,-0.342429526733087,
123.377046507916));
#51820=CARTESIAN_POINT('Ctrl Pts',(20.0265714206272,0.230936564025209,123.412016066948));
#51821=CARTESIAN_POINT('Ctrl Pts',(19.8370330508419,0.772511505541999,123.446993063256));
#51822=CARTESIAN_POINT('Ctrl Pts',(19.5251158650213,1.13509549584705,123.476144022344));
#51823=CARTESIAN_POINT('Ctrl Pts',(19.2089427812759,1.34157439541724,123.499466157668));
#51824=CARTESIAN_POINT('Ctrl Pts',(18.8022297310169,1.51083005679838,123.526675351318));
#51825=CARTESIAN_POINT('Ctrl Pts',(18.1887610066183,1.54150746802044,123.563601539563));
#51826=CARTESIAN_POINT('Ctrl Pts',(17.6066469876977,1.26096106460104,123.602465316226));
#51827=CARTESIAN_POINT('Ctrl Pts',(17.2634272748862,0.890203007238264,123.633549572047));
#51828=CARTESIAN_POINT('Ctrl Pts',(17.082525889251,0.557815732951941,123.656858912516));
#51829=CARTESIAN_POINT('Ctrl Pts',(16.9571642283976,0.0684428947444481,
123.687931234929));
#51830=CARTESIAN_POINT('Ctrl Pts',(17.0295068117547,-0.507832033319457,
123.722875203782));
#51831=CARTESIAN_POINT('Ctrl Pts',(17.3688526160543,-1.04683816221682,123.76168087717));
#51832=CARTESIAN_POINT('Ctrl Pts',(17.8485226943806,-1.40115675162508,123.798041904308));
#51833=CARTESIAN_POINT('Ctrl Pts',(18.4538939392114,-1.54830506570096,123.835832958897));
#51834=CARTESIAN_POINT('Ctrl Pts',(19.0894977356217,-1.43102650733447,123.875047216809));
#51835=CARTESIAN_POINT('Ctrl Pts',(19.5769795248757,-1.09521158649819,123.910962428104));
#51836=CARTESIAN_POINT('Ctrl Pts',(19.8171106927969,-0.743274952053088,
123.937060754552));
#51837=CARTESIAN_POINT('Ctrl Pts',(19.9502929533394,-0.41864633746552,123.958798228661));
#51838=CARTESIAN_POINT('Ctrl Pts',(20.0158658834292,-0.0890469932101259,
123.979438649622));
#51839=CARTESIAN_POINT('Ctrl Pts',(19.9801779106362,0.333611522888986,124.00549195359));
#51840=CARTESIAN_POINT('Ctrl Pts',(19.8290153175581,0.729564899250391,124.031524512427));
#51841=CARTESIAN_POINT('Ctrl Pts',(19.5743395932742,1.06792890083028,124.057536023747));
#51842=CARTESIAN_POINT('Ctrl Pts',(19.2362602337412,1.32231677379998,124.083524975047));
#51843=CARTESIAN_POINT('Ctrl Pts',(18.8741909391828,1.46053309200947,124.107326736802));
#51844=CARTESIAN_POINT('Ctrl Pts',(18.5262231917483,1.50202994660038,124.128946988843));
#51845=CARTESIAN_POINT('Ctrl Pts',(18.1076238579464,1.4640685601785,124.154872476773));
#51846=CARTESIAN_POINT('Ctrl Pts',(17.6176451983895,1.2530494858779,124.187242696241));
#51847=CARTESIAN_POINT('Ctrl Pts',(17.1851241144578,0.782275600676782,124.226025525988));
#51848=CARTESIAN_POINT('Ctrl Pts',(16.9829299045482,0.1770230330116,124.264743351255));
#51849=CARTESIAN_POINT('Ctrl Pts',(17.0454911865098,-0.456965239846467,
124.30339306494));
#51850=CARTESIAN_POINT('Ctrl Pts',(17.3609592723271,-1.00905161410177,124.341971388204));
#51851=CARTESIAN_POINT('Ctrl Pts',(17.8734251128938,-1.38342287409913,124.380475205641));
#51852=CARTESIAN_POINT('Ctrl Pts',(18.4928529976412,-1.51554782034155,124.418901391255));
#51853=CARTESIAN_POINT('Ctrl Pts',(19.1109216504511,-1.38342471232708,124.457246905499));
#51854=CARTESIAN_POINT('Ctrl Pts',(19.6200023544194,-1.01118544846169,124.49550874605));
#51855=CARTESIAN_POINT('Ctrl Pts',(19.9319316125004,-0.464719077268282,
124.533683975605));
#51856=CARTESIAN_POINT('Ctrl Pts',(19.9933046864079,0.160025206387855,124.571769710634));
#51857=CARTESIAN_POINT('Ctrl Pts',(19.7946296329937,0.753903791122387,124.609763131141));
#51858=CARTESIAN_POINT('Ctrl Pts',(19.3717730079164,1.21368184599254,124.64766147922));
#51859=CARTESIAN_POINT('Ctrl Pts',(18.7994810228966,1.46000434721644,124.685462062322));
#51860=CARTESIAN_POINT('Ctrl Pts',(18.1781480997808,1.45111278538542,124.723162252709));
#51861=CARTESIAN_POINT('Ctrl Pts',(17.6161784166517,1.1899275989982,124.760759491016));
#51862=CARTESIAN_POINT('Ctrl Pts',(17.2110444840083,0.723298061997832,124.798251287713));
#51863=CARTESIAN_POINT('Ctrl Pts',(17.0323572001242,0.13359183205746,124.835635225636));
#51864=CARTESIAN_POINT('Ctrl Pts',(17.1098918761081,-0.475863436901096,
124.872908960883));
#51865=CARTESIAN_POINT('Ctrl Pts',(17.4286318467171,-0.998910009243678,
124.910070223437));
#51866=CARTESIAN_POINT('Ctrl Pts',(17.9316532413484,-1.34507560956785,124.94711681947));
#51867=CARTESIAN_POINT('Ctrl Pts',(18.5302997942462,-1.4552410218869,124.984046633175));
#51868=CARTESIAN_POINT('Ctrl Pts',(19.1198269249153,-1.31174356609111,125.020857628516));
#51869=CARTESIAN_POINT('Ctrl Pts',(19.5977510346322,-0.941189098052047,
125.057547850278));
#51870=CARTESIAN_POINT('Ctrl Pts',(19.8816855461754,-0.409529192802567,
125.094115424384));
#51871=CARTESIAN_POINT('Ctrl Pts',(19.9235560493417,0.18968666604768,125.130558559894));
#51872=CARTESIAN_POINT('Ctrl Pts',(19.7177399243904,0.751788965015347,125.166875550473));
#51873=CARTESIAN_POINT('Ctrl Pts',(19.3017530441372,1.17929037033942,125.203064775802));
#51874=CARTESIAN_POINT('Ctrl Pts',(18.7494159379068,1.39880874462414,125.239124702444));
#51875=CARTESIAN_POINT('Ctrl Pts',(18.1577440922458,1.37367073694802,125.275053884033));
#51876=CARTESIAN_POINT('Ctrl Pts',(17.6298927509336,1.11003035193486,125.310850962849));
#51877=CARTESIAN_POINT('Ctrl Pts',(17.2571574920252,0.655483923670628,125.346514670974));
#51878=CARTESIAN_POINT('Ctrl Pts',(17.1031737632591,0.090478868078499,125.382043831286));
#51879=CARTESIAN_POINT('Ctrl Pts',(17.1930513384486,-0.485932720696993,
125.417437358099));
#51880=CARTESIAN_POINT('Ctrl Pts',(17.5092987036455,-0.97347085777756,125.452694257279));
#51881=CARTESIAN_POINT('Ctrl Pts',(17.9951946615233,-1.28808402644339,125.487813627298));
#51882=CARTESIAN_POINT('Ctrl Pts',(18.5649614447451,-1.37644458054661,125.522794660169));
#51883=CARTESIAN_POINT('Ctrl Pts',(19.1189140641177,-1.22498304396499,125.557636641932));
#51884=CARTESIAN_POINT('Ctrl Pts',(19.5609089134785,-0.861932403090798,
125.592338953059));
#51885=CARTESIAN_POINT('Ctrl Pts',(19.8150359936985,-0.3520829415954,125.626901068439));
#51886=CARTESIAN_POINT('Ctrl Pts',(19.8386557221893,0.214780046773663,125.661322558033));
#51887=CARTESIAN_POINT('Ctrl Pts',(19.6295419625641,0.739691486449853,125.695603087442));
#51888=CARTESIAN_POINT('Ctrl Pts',(19.2259376869629,1.13178788840374,125.729742418013));
#51889=CARTESIAN_POINT('Ctrl Pts',(18.699572821645,1.32403667491472,125.763740406868));
#51890=CARTESIAN_POINT('Ctrl Pts',(18.1429176388844,1.28469073562223,125.79759700673));
#51891=CARTESIAN_POINT('Ctrl Pts',(17.6529372209239,1.02251218425985,125.83131226639));
#51892=CARTESIAN_POINT('Ctrl Pts',(17.314201690391,0.584910210351183,125.864886330625));
#51893=CARTESIAN_POINT('Ctrl Pts',(17.1842938014887,0.0493775379142845,
125.8983194402));
#51894=CARTESIAN_POINT('Ctrl Pts',(17.2840304301682,-0.490228611078988,
125.931611931248));
#51895=CARTESIAN_POINT('Ctrl Pts',(17.5941561350494,-0.940132612138631,
125.964764235148));
#51896=CARTESIAN_POINT('Ctrl Pts',(18.0590277207118,-1.2229319970556,125.997776878586));
#51897=CARTESIAN_POINT('Ctrl Pts',(18.5965888870425,-1.29090509505102,126.030650483148));
#51898=CARTESIAN_POINT('Ctrl Pts',(19.1128476053057,-1.13404910216438,126.063385764873));
#51899=CARTESIAN_POINT('Ctrl Pts',(19.5183028611001,-0.781498242508856,
126.095983533252));
#51900=CARTESIAN_POINT('Ctrl Pts',(19.7434513004666,-0.296132794314435,
126.128444690937));
#51901=CARTESIAN_POINT('Ctrl Pts',(19.7506887966976,0.236626129343923,126.160770233622));
#51902=CARTESIAN_POINT('Ctrl Pts',(19.5405717683373,0.723840014487345,126.192961249111));
#51903=CARTESIAN_POINT('Ctrl Pts',(19.1514003155747,1.08125376520771,126.225018916639));
#51904=CARTESIAN_POINT('Ctrl Pts',(18.6522529654985,1.24785219893955,126.256944505325));
#51905=CARTESIAN_POINT('Ctrl Pts',(18.1307374876082,1.19626020002051,126.288739373834));
#51906=CARTESIAN_POINT('Ctrl Pts',(17.6776283044279,0.937216920035472,126.320404969913));
#51907=CARTESIAN_POINT('Ctrl Pts',(17.3710826183557,0.517398188580757,126.351942829254));
#51908=CARTESIAN_POINT('Ctrl Pts',(17.2631766509069,0.0110212755183283,
126.383354574252));
#51909=CARTESIAN_POINT('Ctrl Pts',(17.3710775008581,-0.493259952344315,
126.414641912253));
#51910=CARTESIAN_POINT('Ctrl Pts',(17.674343269895,-0.907858065298181,126.445806634917));
#51911=CARTESIAN_POINT('Ctrl Pts',(18.1187695860277,-1.16144504596442,126.476850617591));
#51912=CARTESIAN_POINT('Ctrl Pts',(18.6260618945864,-1.21120322734561,126.507775817858));
#51913=CARTESIAN_POINT('Ctrl Pts',(19.1076094508818,-1.05003444205409,126.538584273908));
#51914=CARTESIAN_POINT('Ctrl Pts',(19.479941054855,-0.707518256395985,126.569278102458));
#51915=CARTESIAN_POINT('Ctrl Pts',(19.6791707230463,-0.24450208536029,126.599859497819));
#51916=CARTESIAN_POINT('Ctrl Pts',(19.6719374762803,0.257689964881801,126.630330731029));
#51917=CARTESIAN_POINT('Ctrl Pts',(19.4609699048984,0.711518134755177,126.660694148595));
#51918=CARTESIAN_POINT('Ctrl Pts',(19.0843530164292,1.03846031023916,126.690952169495));
#51919=CARTESIAN_POINT('Ctrl Pts',(18.6086699841862,1.18257251108356,126.721107284798));
#51920=CARTESIAN_POINT('Ctrl Pts',(18.1172532654699,1.12003822633395,126.751162052644));
#51921=CARTESIAN_POINT('Ctrl Pts',(17.6956108030026,0.863083641583314,126.781119104258));
#51922=CARTESIAN_POINT('Ctrl Pts',(17.416579633507,0.457614474125132,126.810981129717));
#51923=CARTESIAN_POINT('Ctrl Pts',(17.3277652379225,-0.0249623152391279,
126.840750898208));
#51924=CARTESIAN_POINT('Ctrl Pts',(17.4434533079629,-0.500296570460753,
126.870431213523));
#51925=CARTESIAN_POINT('Ctrl Pts',(17.7423144868672,-0.88579332001242,126.90002499059));
#51926=CARTESIAN_POINT('Ctrl Pts',(18.1713583899084,-1.11496153501696,126.929535108301));
#51927=CARTESIAN_POINT('Ctrl Pts',(18.6552355318737,-1.14880190241397,126.958964681934));
#51928=CARTESIAN_POINT('Ctrl Pts',(19.1095782364948,-0.982521504293672,
126.988316543786));
#51929=CARTESIAN_POINT('Ctrl Pts',(19.3977730939009,-0.702071800600608,
127.012714617116));
#51930=CARTESIAN_POINT('Ctrl Pts',(19.544407755015,-0.422356879638505,127.032197081111));
#51931=CARTESIAN_POINT('Ctrl Pts',(19.6298827620869,-0.118693626635683,
127.051656751625));
#51932=CARTESIAN_POINT('Ctrl Pts',(19.6130086123708,0.281159288420498,127.075938299492));
#51933=CARTESIAN_POINT('Ctrl Pts',(19.398925270687,0.709905348928385,127.105011643396));
#51934=CARTESIAN_POINT('Ctrl Pts',(19.0292329604127,1.01317916174629,127.13402325986));
#51935=CARTESIAN_POINT('Ctrl Pts',(18.5688144179712,1.13875566987803,127.162976744829));
#51936=CARTESIAN_POINT('Ctrl Pts',(18.0981675564226,1.06546968077371,127.191875335313));
#51937=CARTESIAN_POINT('Ctrl Pts',(17.6992029213682,0.806808307174844,127.220722517499));
#51938=CARTESIAN_POINT('Ctrl Pts',(17.4411124901692,0.408418905232783,127.2495217004));
#51939=CARTESIAN_POINT('Ctrl Pts',(17.3683562548528,-0.059914175730859,
127.278276385889));
#51940=CARTESIAN_POINT('Ctrl Pts',(17.4930509072919,-0.516467398722105,
127.306990073295));
#51941=CARTESIAN_POINT('Ctrl Pts',(17.7929496172605,-0.881797347761693,
127.335666305827));
#51942=CARTESIAN_POINT('Ctrl Pts',(18.2154066647599,-1.09252862496411,127.364308643604));
#51943=CARTESIAN_POINT('Ctrl Pts',(18.6865908567962,-1.11231576412509,127.392920676274));
#51944=CARTESIAN_POINT('Ctrl Pts',(19.1243553998719,-0.938093194560736,
127.421506009437));
#51945=CARTESIAN_POINT('Ctrl Pts',(19.45251882398,-0.600540327235931,127.45006827227));
#51946=CARTESIAN_POINT('Ctrl Pts',(19.6140849830491,-0.158694271514664,
127.478611095749));
#51947=CARTESIAN_POINT('Ctrl Pts',(19.5811155297149,0.310347270840708,127.507138158241));
#51948=CARTESIAN_POINT('Ctrl Pts',(19.3595430994241,0.724840908398939,127.535653065854));
#51949=CARTESIAN_POINT('Ctrl Pts',(18.9881132079945,1.01260452927925,127.564159617603));
#51950=CARTESIAN_POINT('Ctrl Pts',(18.531618625509,1.1235480699415,127.592661253259));
#51951=CARTESIAN_POINT('Ctrl Pts',(18.0696423587533,1.03837509085643,127.621162112442));
#51952=CARTESIAN_POINT('Ctrl Pts',(17.6827054043867,0.771915824816395,127.649664924942));
#51953=CARTESIAN_POINT('Ctrl Pts',(17.4382943211488,0.370573227075538,127.678175448639));
#51954=CARTESIAN_POINT('Ctrl Pts',(17.3790816129046,-0.0957583806675449,
127.706693056054));
#51955=CARTESIAN_POINT('Ctrl Pts',(17.5156217028773,-0.54581326651222,127.735229383328));
#51956=CARTESIAN_POINT('Ctrl Pts',(17.8241150899294,-0.901101660216496,
127.763774970624));
#51957=CARTESIAN_POINT('Ctrl Pts',(18.2514042557898,-1.09944789271686,127.792354060315));
#51958=CARTESIAN_POINT('Ctrl Pts',(18.7223811907647,-1.10621903008227,127.820935645081));
#51959=CARTESIAN_POINT('Ctrl Pts',(19.1561166875056,-0.919327144483553,
127.849587422587));
#51960=CARTESIAN_POINT('Ctrl Pts',(19.4756002029098,-0.572270806023172,
127.878200076059));
#51961=CARTESIAN_POINT('Ctrl Pts',(19.6249067912141,-0.122932666865693,
127.906929915726));
#51962=CARTESIAN_POINT('Ctrl Pts',(19.5878100755787,0.269735776585891,127.930897472309));
#51963=CARTESIAN_POINT('Ctrl Pts',(19.4623935348208,0.552856736689258,127.94996601605));
#51964=CARTESIAN_POINT('Ctrl Pts',(19.3242851294489,0.74328918256335,127.964401021732));
#51965=CARTESIAN_POINT('Ctrl Pts',(19.1499004928383,0.900980613118008,127.978886757729));
#51966=CARTESIAN_POINT('Ctrl Pts',(18.951180564553,1.01733117928007,127.99328776375));
#51967=CARTESIAN_POINT('Ctrl Pts',(18.7347414903714,1.08846509195581,128.007592012474));
#51968=CARTESIAN_POINT('Ctrl Pts',(18.5768458460658,1.10568133857386,128.01727789117));
#51969=CARTESIAN_POINT('Ctrl Pts',(18.4937646355866,1.10638059843974,128.022196038513));
#51970=CARTESIAN_POINT('Ctrl Pts',(18.4930824954759,1.12090089948759,112.757679850141));
#51971=CARTESIAN_POINT('Ctrl Pts',(18.3665883682682,1.11983625122485,112.765167906081));
#51972=CARTESIAN_POINT('Ctrl Pts',(18.2101165898736,1.09441509929884,112.774937242857));
#51973=CARTESIAN_POINT('Ctrl Pts',(17.9940242321427,1.01053960936053,112.789530556343));
#51974=CARTESIAN_POINT('Ctrl Pts',(17.8253522939624,0.911714328966616,112.801759037985));
#51975=CARTESIAN_POINT('Ctrl Pts',(17.6473020816238,0.750791187869453,112.816545585475));
#51976=CARTESIAN_POINT('Ctrl Pts',(17.5057913426302,0.555764932259308,112.831330741684));
#51977=CARTESIAN_POINT('Ctrl Pts',(17.3767761116466,0.264559939346119,112.850945111638));
#51978=CARTESIAN_POINT('Ctrl Pts',(17.3383331924762,-0.140265095337886,
112.875655684827));
#51979=CARTESIAN_POINT('Ctrl Pts',(17.4927882555132,-0.605925596627459,
112.905423832316));
#51980=CARTESIAN_POINT('Ctrl Pts',(17.8254561829886,-0.967734043234468,
112.935237085143));
#51981=CARTESIAN_POINT('Ctrl Pts',(18.2793089423996,-1.16352235132462,112.965222037507));
#51982=CARTESIAN_POINT('Ctrl Pts',(18.7747576544017,-1.15669178044294,112.995289912586));
#51983=CARTESIAN_POINT('Ctrl Pts',(19.2264713360212,-0.947257459845427,
113.02549484845));
#51984=CARTESIAN_POINT('Ctrl Pts',(19.5543003375184,-0.570103883609804,
113.055812262305));
#51985=CARTESIAN_POINT('Ctrl Pts',(19.7002188514683,-0.0899595846873296,
113.086259988855));
#51986=CARTESIAN_POINT('Ctrl Pts',(19.6369907959431,0.409971727794146,113.1168309809));
#51987=CARTESIAN_POINT('Ctrl Pts',(19.3739931350828,0.842295715905271,113.147533111348));
#51988=CARTESIAN_POINT('Ctrl Pts',(18.955569154602,1.13072856629342,113.178365554388));
#51989=CARTESIAN_POINT('Ctrl Pts',(18.4536699456387,1.22350120172658,113.209331880026));
#51990=CARTESIAN_POINT('Ctrl Pts',(17.955480573998,1.10266249250285,113.240433415561));
#51991=CARTESIAN_POINT('Ctrl Pts',(17.5483074543974,0.787495789961384,113.271672405762));
#51992=CARTESIAN_POINT('Ctrl Pts',(17.3042899501749,0.331487994701509,113.303050509289));
#51993=CARTESIAN_POINT('Ctrl Pts',(17.2676425549497,-0.186732323798034,
113.334569540469));
#51994=CARTESIAN_POINT('Ctrl Pts',(17.4466617531715,-0.676931075321784,
113.366231100277));
#51995=CARTESIAN_POINT('Ctrl Pts',(17.8119359198239,-1.05296122692266,113.39803672783));
#51996=CARTESIAN_POINT('Ctrl Pts',(18.3011750647179,-1.24788995601349,113.429987890354));
#51997=CARTESIAN_POINT('Ctrl Pts',(18.8297649694566,-1.22589192727795,113.462085865074));
#51998=CARTESIAN_POINT('Ctrl Pts',(19.3054703951861,-0.988819290874638,
113.494331996892));
#51999=CARTESIAN_POINT('Ctrl Pts',(19.6444065316308,-0.576226626359959,
113.526727323068));
#52000=CARTESIAN_POINT('Ctrl Pts',(19.7859212202161,-0.0588050517471134,
113.559272952392));
#52001=CARTESIAN_POINT('Ctrl Pts',(19.7033719576413,0.47377367502414,113.591969792592));
#52002=CARTESIAN_POINT('Ctrl Pts',(19.4091319363877,0.928265721457266,113.624818684065));
#52003=CARTESIAN_POINT('Ctrl Pts',(18.9528039781542,1.22434665049485,113.657820367104));
#52004=CARTESIAN_POINT('Ctrl Pts',(18.5028388600387,1.29449412400773,113.68544960784));
#52005=CARTESIAN_POINT('Ctrl Pts',(18.1479930389594,1.23643849564634,113.707629976648));
#52006=CARTESIAN_POINT('Ctrl Pts',(17.8120670406829,1.10593529978113,113.729861743692));
#52007=CARTESIAN_POINT('Ctrl Pts',(17.4566011291118,0.814568801733298,113.75774788851));
#52008=CARTESIAN_POINT('Ctrl Pts',(17.2089757557268,0.318843304737269,113.791365973));
#52009=CARTESIAN_POINT('Ctrl Pts',(17.1852851292711,-0.237300982291561,
113.82513892758));
#52010=CARTESIAN_POINT('Ctrl Pts',(17.3917751493225,-0.757010035973108,
113.859066883272));
#52011=CARTESIAN_POINT('Ctrl Pts',(17.7943511543741,-1.14882229284447,113.893149827088));
#52012=CARTESIAN_POINT('Ctrl Pts',(18.3242514269155,-1.34291473661002,113.927387660746));
#52013=CARTESIAN_POINT('Ctrl Pts',(18.8897524203654,-1.30346129922779,113.96178017383));
#52014=CARTESIAN_POINT('Ctrl Pts',(19.3920622637203,-1.0352770156871,113.996327045818));
#52015=CARTESIAN_POINT('Ctrl Pts',(19.7425772839418,-0.583305907411899,
114.031027870034));
#52016=CARTESIAN_POINT('Ctrl Pts',(19.8785122908702,-0.0251396062433737,
114.065882103309));
#52017=CARTESIAN_POINT('Ctrl Pts',(19.7741540483073,0.542360198983367,114.100889139007));
#52018=CARTESIAN_POINT('Ctrl Pts',(19.4456896959022,1.01978490940607,114.136048227714));
#52019=CARTESIAN_POINT('Ctrl Pts',(18.9487316956458,1.32271689126222,114.171358545353));
#52020=CARTESIAN_POINT('Ctrl Pts',(18.3689335050377,1.3965536931616,114.206819149106));
#52021=CARTESIAN_POINT('Ctrl Pts',(17.8071893150124,1.22642114794512,114.242429002406));
#52022=CARTESIAN_POINT('Ctrl Pts',(17.3620871476616,0.840084178305824,114.278186961052));
#52023=CARTESIAN_POINT('Ctrl Pts',(17.1125862773131,0.303442518713258,114.314091790017));
#52024=CARTESIAN_POINT('Ctrl Pts',(17.1039992313928,-0.29069230440087,114.350142137921));
#52025=CARTESIAN_POINT('Ctrl Pts',(17.339781679565,-0.838712338207705,114.386336584108));
#52026=CARTESIAN_POINT('Ctrl Pts',(17.7805525009889,-1.24418911264205,114.422673554901));
#52027=CARTESIAN_POINT('Ctrl Pts',(18.3507274190001,-1.43506356953502,114.459151484535));
#52028=CARTESIAN_POINT('Ctrl Pts',(18.8512555693308,-1.38589286433566,114.489665673091));
#52029=CARTESIAN_POINT('Ctrl Pts',(19.2144873415626,-1.22603513103535,114.514145775214));
#52030=CARTESIAN_POINT('Ctrl Pts',(19.5373516406566,-0.994043405793173,
114.538671340607));
#52031=CARTESIAN_POINT('Ctrl Pts',(19.8365357359841,-0.585125520559961,
114.569412866718));
#52032=CARTESIAN_POINT('Ctrl Pts',(19.9641680455432,0.0116468285138929,
114.606436218208));
#52033=CARTESIAN_POINT('Ctrl Pts',(19.8365166045373,0.610578458805209,114.643590857788));
#52034=CARTESIAN_POINT('Ctrl Pts',(19.4740841771901,1.10687327644485,114.680874670396));
#52035=CARTESIAN_POINT('Ctrl Pts',(18.9387445540885,1.41286803486826,114.718285330484));
#52036=CARTESIAN_POINT('Ctrl Pts',(18.3230736607037,1.47372940305447,114.755820519772));
#52037=CARTESIAN_POINT('Ctrl Pts',(17.7343186963893,1.27715511909712,114.793477731825));
#52038=CARTESIAN_POINT('Ctrl Pts',(17.2757904414825,0.855945729927207,114.831254534063));
#52039=CARTESIAN_POINT('Ctrl Pts',(17.0284653198638,0.282361907137467,114.869148139596));
#52040=CARTESIAN_POINT('Ctrl Pts',(17.0362003735306,-0.274389704184093,
114.902933084858));
#52041=CARTESIAN_POINT('Ctrl Pts',(17.2085237252143,-0.725107334144531,
114.932566782391));
#52042=CARTESIAN_POINT('Ctrl Pts',(17.3951754462632,-0.973455623444401,
114.951654102959));
#52043=CARTESIAN_POINT('Ctrl Pts',(17.5456173829533,-1.11352655242482,114.964393287536));
#52044=CARTESIAN_POINT('Ctrl Pts',(17.6254879200035,-1.17821151495492,114.970766127917));
#52045=CARTESIAN_POINT('Ctrl Pts',(17.7098144577346,-1.23711376226772,114.977141778623));
#52046=CARTESIAN_POINT('Ctrl Pts',(17.8862821458639,-1.34296898272677,114.989899536136));
#52047=CARTESIAN_POINT('Ctrl Pts',(18.1776912562802,-1.45422368744665,115.00905699236));
#52048=CARTESIAN_POINT('Ctrl Pts',(18.5927994037828,-1.48930722877114,115.034647641612));
#52049=CARTESIAN_POINT('Ctrl Pts',(19.0022284342603,-1.40791898797909,115.060282536743));
#52050=CARTESIAN_POINT('Ctrl Pts',(19.3735618999477,-1.21609226917294,115.085962555239));
#52051=CARTESIAN_POINT('Ctrl Pts',(19.678145682308,-0.928385692937971,115.111685215156));
#52052=CARTESIAN_POINT('Ctrl Pts',(19.8908852298623,-0.567169870467851,
115.137450886196));
#52053=CARTESIAN_POINT('Ctrl Pts',(20.0319650959912,-0.0245695829546816,
115.171859957911));
#52054=CARTESIAN_POINT('Ctrl Pts',(19.9355006689882,0.545066308576247,115.206350112054));
#52055=CARTESIAN_POINT('Ctrl Pts',(19.6607594620582,0.954350677105631,115.236596811922));
#52056=CARTESIAN_POINT('Ctrl Pts',(19.4606676325734,1.14929313186806,115.253898981719));
#52057=CARTESIAN_POINT('Ctrl Pts',(19.2345360594306,1.31443977360675,115.271213897795));
#52058=CARTESIAN_POINT('Ctrl Pts',(19.0093660410988,1.4153511981227,115.286380615372));
#52059=CARTESIAN_POINT('Ctrl Pts',(18.8056648791855,1.46628172584519,115.299391205841));
#52060=CARTESIAN_POINT('Ctrl Pts',(18.70233708238,1.48460038389795,115.305898900516));
#52061=CARTESIAN_POINT('Ctrl Pts',(18.6152995235572,1.49382058101683,115.31132371314));
#52062=CARTESIAN_POINT('Ctrl Pts',(18.5453906128826,1.49743368689553,115.315664843346));
#52063=CARTESIAN_POINT('Ctrl Pts',(18.2616037566892,1.50286105643157,115.333272874718));
#52064=CARTESIAN_POINT('Ctrl Pts',(17.7457736243556,1.37132382404071,115.365273134799));
#52065=CARTESIAN_POINT('Ctrl Pts',(17.3050555028768,0.962837299905914,115.401418669274));
#52066=CARTESIAN_POINT('Ctrl Pts',(17.1086587613839,0.593395661306247,115.427273326137));
#52067=CARTESIAN_POINT('Ctrl Pts',(17.041754656606,0.395197980803883,115.440209277673));
#52068=CARTESIAN_POINT('Ctrl Pts',(17.0088461550716,0.231377891853717,115.45056305284));
#52069=CARTESIAN_POINT('Ctrl Pts',(16.9695299982344,-0.100563471670666,
115.471278156146));
#52070=CARTESIAN_POINT('Ctrl Pts',(17.0668112497359,-0.652391726720423,
115.504977987031));
#52071=CARTESIAN_POINT('Ctrl Pts',(17.5514104118804,-1.26053326074223,115.551724578996));
#52072=CARTESIAN_POINT('Ctrl Pts',(18.2091610061576,-1.53767209463446,115.594647763884));
#52073=CARTESIAN_POINT('Ctrl Pts',(18.8498791049214,-1.51327085728669,115.633721735647));
#52074=CARTESIAN_POINT('Ctrl Pts',(19.3792076114729,-1.28260786692149,115.668926420135));
#52075=CARTESIAN_POINT('Ctrl Pts',(19.7881337259166,-0.873687487640924,
115.704166304091));
#52076=CARTESIAN_POINT('Ctrl Pts',(19.9809069947669,-0.431787129828086,
115.733560457919));
#52077=CARTESIAN_POINT('Ctrl Pts',(20.0304646093459,-0.0539560084034985,
115.757090137144));
#52078=CARTESIAN_POINT('Ctrl Pts',(20.014513183359,0.231413092827471,115.774745421663));
#52079=CARTESIAN_POINT('Ctrl Pts',(19.9571325086356,0.462752236719258,115.789462821084));
#52080=CARTESIAN_POINT('Ctrl Pts',(19.8859980822438,0.638993028576267,115.801240368326));
#52081=CARTESIAN_POINT('Ctrl Pts',(19.7552607146953,0.892444019511638,115.818910181336));
#52082=CARTESIAN_POINT('Ctrl Pts',(19.4715368254779,1.22216613224498,115.84542538746));
#52083=CARTESIAN_POINT('Ctrl Pts',(18.9584318064315,1.49339724075382,115.880801368486));
#52084=CARTESIAN_POINT('Ctrl Pts',(18.3813899373706,1.55843356026758,115.916195855039));
#52085=CARTESIAN_POINT('Ctrl Pts',(17.9605504546436,1.44568553379809,115.942753651494));
#52086=CARTESIAN_POINT('Ctrl Pts',(17.7091835003908,1.30962683993775,115.96046307762));
#52087=CARTESIAN_POINT('Ctrl Pts',(17.5507370910921,1.20379635308115,115.972270697712));
#52088=CARTESIAN_POINT('Ctrl Pts',(17.3011550655096,0.98086341180248,115.992935385917));
#52089=CARTESIAN_POINT('Ctrl Pts',(17.1334706598133,0.714436140504968,116.012129312691));
#52090=CARTESIAN_POINT('Ctrl Pts',(17.0518809246904,0.490682531218659,116.026895286345));
#52091=CARTESIAN_POINT('Ctrl Pts',(17.0304611374528,0.422553018506051,116.031325075242));
#52092=CARTESIAN_POINT('Ctrl Pts',(17.0123149108823,0.353447043175113,116.035755043463));
#52093=CARTESIAN_POINT('Ctrl Pts',(16.9973973546347,0.283593260328368,116.04018507481));
#52094=CARTESIAN_POINT('Ctrl Pts',(16.9857382118008,0.213104433320238,116.044615258831));
#52095=CARTESIAN_POINT('Ctrl Pts',(16.9746811349069,0.118498464452188,116.050522304053));
#52096=CARTESIAN_POINT('Ctrl Pts',(16.9622358386438,-0.143393353812591,
116.066767577372));
#52097=CARTESIAN_POINT('Ctrl Pts',(17.0433378618505,-0.57191585117926,116.093351814281));
#52098=CARTESIAN_POINT('Ctrl Pts',(17.3527452079877,-1.06435322127642,116.128800325967));
#52099=CARTESIAN_POINT('Ctrl Pts',(17.8206484218217,-1.40967908128267,116.164247300363));
#52100=CARTESIAN_POINT('Ctrl Pts',(18.3823463748326,-1.56016792906666,116.199690802844));
#52101=CARTESIAN_POINT('Ctrl Pts',(18.960023412883,-1.49507323389592,116.235127425045));
#52102=CARTESIAN_POINT('Ctrl Pts',(19.473954356025,-1.22345837930286,116.270554878086));
#52103=CARTESIAN_POINT('Ctrl Pts',(19.7685848901886,-0.880932463929016,
116.298099485735));
#52104=CARTESIAN_POINT('Ctrl Pts',(19.9099467736206,-0.596314691693052,
116.317769354208));
#52105=CARTESIAN_POINT('Ctrl Pts',(19.9937199319316,-0.356497524231079,
116.333502033051));
#52106=CARTESIAN_POINT('Ctrl Pts',(20.0610683033509,0.0857899363499977,
116.361028744888));
#52107=CARTESIAN_POINT('Ctrl Pts',(19.915745394596,0.722908696208606,116.400330942654));
#52108=CARTESIAN_POINT('Ctrl Pts',(19.3969443143545,1.31053562959535,116.447453844904));
#52109=CARTESIAN_POINT('Ctrl Pts',(18.6612967313308,1.57818772307471,116.494529797347));
#52110=CARTESIAN_POINT('Ctrl Pts',(17.8879145752841,1.46154465113853,116.541552584403));
#52111=CARTESIAN_POINT('Ctrl Pts',(17.3562475109639,1.05855180793689,116.581666715373));
#52112=CARTESIAN_POINT('Ctrl Pts',(17.0822320017472,0.592142557113021,116.614895645628));
#52113=CARTESIAN_POINT('Ctrl Pts',(16.9381151379149,0.0381362663569181,
116.650049508666));
#52114=CARTESIAN_POINT('Ctrl Pts',(17.06135129899,-0.687251812711299,116.693934033461));
#52115=CARTESIAN_POINT('Ctrl Pts',(17.6489755475387,-1.34438516219944,116.746493535922));
#52116=CARTESIAN_POINT('Ctrl Pts',(18.4942268949859,-1.58756196052271,116.798942419545));
#52117=CARTESIAN_POINT('Ctrl Pts',(19.337338674134,-1.34440174201639,116.851272002281));
#52118=CARTESIAN_POINT('Ctrl Pts',(19.92063012609,-0.691351138595169,116.90347356047));
#52119=CARTESIAN_POINT('Ctrl Pts',(20.0418737752447,0.025869309660071,116.946861524311));
#52120=CARTESIAN_POINT('Ctrl Pts',(19.8998969931766,0.571745128810662,116.981499280576));
#52121=CARTESIAN_POINT('Ctrl Pts',(19.6858090505737,0.935720760934458,117.007440856283));
#52122=CARTESIAN_POINT('Ctrl Pts',(19.3789673554751,1.22500437846248,117.033343801827));
#52123=CARTESIAN_POINT('Ctrl Pts',(18.8805090860516,1.48367338497174,117.067829408806));
#52124=CARTESIAN_POINT('Ctrl Pts',(18.1606038475644,1.52404123757986,117.110835756358));
#52125=CARTESIAN_POINT('Ctrl Pts',(17.4056904905111,1.10626788119792,117.162275443176));
#52126=CARTESIAN_POINT('Ctrl Pts',(16.9902676509324,0.353713203820808,117.213539395222));
#52127=CARTESIAN_POINT('Ctrl Pts',(17.0387094918925,-0.501579978728816,
117.264620504126));
#52128=CARTESIAN_POINT('Ctrl Pts',(17.5329599372551,-1.19732719183391,117.31551163559));
#52129=CARTESIAN_POINT('Ctrl Pts',(18.3185603384476,-1.5222362057658,117.366206019748));
#52130=CARTESIAN_POINT('Ctrl Pts',(19.1532504124722,-1.37991603886097,117.416697051433));
#52131=CARTESIAN_POINT('Ctrl Pts',(19.7816490558389,-0.817671078757634,
117.466978403285));
#52132=CARTESIAN_POINT('Ctrl Pts',(20.0135833048256,-0.0107439011157763,
117.51704398714));
#52133=CARTESIAN_POINT('Ctrl Pts',(19.7816717126225,0.792319952976642,117.56688798825));
#52134=CARTESIAN_POINT('Ctrl Pts',(19.1608825384109,1.34636250207202,117.616504844247));
#52135=CARTESIAN_POINT('Ctrl Pts',(18.3443183643152,1.48453909285033,117.665889273317));
#52136=CARTESIAN_POINT('Ctrl Pts',(17.583080543547,1.16861015724102,117.715036278499));
#52137=CARTESIAN_POINT('Ctrl Pts',(17.1089685240541,0.499410868515231,117.763941144654));
#52138=CARTESIAN_POINT('Ctrl Pts',(17.063797208761,-0.315336896122432,117.812599443987));
#52139=CARTESIAN_POINT('Ctrl Pts',(17.4570085476632,-1.02554149240549,117.861007055314));
#52140=CARTESIAN_POINT('Ctrl Pts',(18.1640470768909,-1.41563553676877,117.909160155275));
#52141=CARTESIAN_POINT('Ctrl Pts',(18.9659789153658,-1.36996787540684,117.957055229807));
#52142=CARTESIAN_POINT('Ctrl Pts',(19.6170386441137,-0.907245642934142,
118.004689063668));
#52143=CARTESIAN_POINT('Ctrl Pts',(19.9205783683424,-0.173019719646544,
118.052058788429));
#52144=CARTESIAN_POINT('Ctrl Pts',(19.8095868167875,0.475732877498027,118.091311294739));
#52145=CARTESIAN_POINT('Ctrl Pts',(19.5257452599602,0.898279490209589,118.122578859281));
#52146=CARTESIAN_POINT('Ctrl Pts',(19.1385654967184,1.22658636111508,118.153756402072));
#52147=CARTESIAN_POINT('Ctrl Pts',(18.5132602545178,1.40641663127513,118.192559112172));
#52148=CARTESIAN_POINT('Ctrl Pts',(17.7674133597538,1.19077223754927,118.23884983952));
#52149=CARTESIAN_POINT('Ctrl Pts',(17.2537148357509,0.614990335990114,118.284866859679));
#52150=CARTESIAN_POINT('Ctrl Pts',(17.1258431048699,-0.141409915617434,
118.330609188837));
#52151=CARTESIAN_POINT('Ctrl Pts',(17.418242037862,-0.845576547539981,118.376076242404));
#52152=CARTESIAN_POINT('Ctrl Pts',(18.0366942746291,-1.28361257902887,118.421267732646));
#52153=CARTESIAN_POINT('Ctrl Pts',(18.7887803634788,-1.32517662651085,118.466183719367));
#52154=CARTESIAN_POINT('Ctrl Pts',(19.4436861157114,-0.962516049661502,
118.510824594297));
#52155=CARTESIAN_POINT('Ctrl Pts',(19.8029993786324,-0.310963483597782,
118.555191066519));
#52156=CARTESIAN_POINT('Ctrl Pts',(19.7609285432409,0.427174297464442,118.599284210161));
#52157=CARTESIAN_POINT('Ctrl Pts',(19.3350856476775,1.02632487648794,118.643105363827));
#52158=CARTESIAN_POINT('Ctrl Pts',(18.7727329827513,1.25846786869882,118.679397823757));
#52159=CARTESIAN_POINT('Ctrl Pts',(18.3022615240602,1.24425151779425,118.708297621323));
#52160=CARTESIAN_POINT('Ctrl Pts',(17.9671502464406,1.13772165563029,118.729905777668));
#52161=CARTESIAN_POINT('Ctrl Pts',(17.6755615111956,0.942607394299044,118.751447393656));
#52162=CARTESIAN_POINT('Ctrl Pts',(17.4500539954179,0.675538200698231,118.772922954479));
#52163=CARTESIAN_POINT('Ctrl Pts',(17.3077447937584,0.357268879764495,118.79433265138));
#52164=CARTESIAN_POINT('Ctrl Pts',(17.2592510930774,0.0132284868385163,
118.815676981559));
#52165=CARTESIAN_POINT('Ctrl Pts',(17.3077344272548,-0.329873474156492,
118.83695621263));
#52166=CARTESIAN_POINT('Ctrl Pts',(17.4253889548699,-0.592464205208098,
118.854635131944));
#52167=CARTESIAN_POINT('Ctrl Pts',(17.5599631022999,-0.77667438666265,118.868745986558));
#52168=CARTESIAN_POINT('Ctrl Pts',(17.7187598102564,-0.939688687757648,
118.882835792676));
#52169=CARTESIAN_POINT('Ctrl Pts',(18.0515602644821,-1.16295343598271,118.907436743883));
#52170=CARTESIAN_POINT('Ctrl Pts',(18.6297474877978,-1.26093160039624,118.942422930714));
#52171=CARTESIAN_POINT('Ctrl Pts',(19.2764330124332,-0.992404814600162,
118.984156975342));
#52172=CARTESIAN_POINT('Ctrl Pts',(19.61120284939,-0.519416332488902,119.018730962761));
#52173=CARTESIAN_POINT('Ctrl Pts',(19.686909231104,-0.134245860237119,119.042827779968));
#52174=CARTESIAN_POINT('Ctrl Pts',(19.6839452453031,0.0875961253331513,
119.056567264143));
#52175=CARTESIAN_POINT('Ctrl Pts',(19.6498909294618,0.306908054978469,119.070287444309));
#52176=CARTESIAN_POINT('Ctrl Pts',(19.5503299373673,0.566837211628185,119.087400456966));
#52177=CARTESIAN_POINT('Ctrl Pts',(19.283502207417,0.922706019580419,119.114703819853));
#52178=CARTESIAN_POINT('Ctrl Pts',(18.7847361296941,1.19802461749581,119.148688660687));
#52179=CARTESIAN_POINT('Ctrl Pts',(18.105589661502,1.15934359728563,119.189245337803));
#52180=CARTESIAN_POINT('Ctrl Pts',(17.554184317493,0.767457727973741,119.229582217277));
#52181=CARTESIAN_POINT('Ctrl Pts',(17.3401465479837,0.249355250526175,119.263018378624));
#52182=CARTESIAN_POINT('Ctrl Pts',(17.3533022473312,-0.184386285466681,
119.289663181768));
#52183=CARTESIAN_POINT('Ctrl Pts',(17.435058145981,-0.441987019344221,119.306274088754));
#52184=CARTESIAN_POINT('Ctrl Pts',(17.5283491445481,-0.604844175741195,
119.317879227065));
#52185=CARTESIAN_POINT('Ctrl Pts',(17.5907056725042,-0.691564410421368,
119.324504643888));
#52186=CARTESIAN_POINT('Ctrl Pts',(17.6590894370632,-0.773661699956384,
119.331125917677));
#52187=CARTESIAN_POINT('Ctrl Pts',(17.7548833948339,-0.866802523811535,
119.339395111115));
#52188=CARTESIAN_POINT('Ctrl Pts',(17.9272916167502,-0.992838247175765,
119.35260859244));
#52189=CARTESIAN_POINT('Ctrl Pts',(18.1722977532925,-1.10244509398686,119.369095798182));
#52190=CARTESIAN_POINT('Ctrl Pts',(18.4904870561884,-1.14730747422361,119.388832136372));
#52191=CARTESIAN_POINT('Ctrl Pts',(18.8078898486568,-1.1024397351981,119.408522019047));
#52192=CARTESIAN_POINT('Ctrl Pts',(19.0997912866972,-0.971773191355699,
119.428165514072));
#52193=CARTESIAN_POINT('Ctrl Pts',(19.3435464737509,-0.765863353259586,
119.447764277111));
#52194=CARTESIAN_POINT('Ctrl Pts',(19.520374037332,-0.50114213177421,119.467318315598));
#52195=CARTESIAN_POINT('Ctrl Pts',(19.6167962999359,-0.198456868038709,
119.486829786065));
#52196=CARTESIAN_POINT('Ctrl Pts',(19.625628021481,0.118361475213261,119.506297999103));
#52197=CARTESIAN_POINT('Ctrl Pts',(19.5597739900227,0.373606936035918,119.522487978212));
#52198=CARTESIAN_POINT('Ctrl Pts',(19.4663649515948,0.560527496785607,119.535418986606));
#52199=CARTESIAN_POINT('Ctrl Pts',(19.3185225194951,0.775596785762759,119.551566637584));
#52200=CARTESIAN_POINT('Ctrl Pts',(19.0310431260634,1.0114115820414,119.574127159248));
#52201=CARTESIAN_POINT('Ctrl Pts',(18.5711112904984,1.13679629805337,119.603048118056));
#52202=CARTESIAN_POINT('Ctrl Pts',(18.1014514961469,1.06361619886642,119.631887037596));
#52203=CARTESIAN_POINT('Ctrl Pts',(17.7037118047289,0.805695586947934,119.660647396262));
#52204=CARTESIAN_POINT('Ctrl Pts',(17.4466785036886,0.408850110880016,119.689332630667));
#52205=CARTESIAN_POINT('Ctrl Pts',(17.3743358538123,-0.0571818016204902,
119.717946446007));
#52206=CARTESIAN_POINT('Ctrl Pts',(17.4983253082146,-0.511079568737379,
119.746492162257));
#52207=CARTESIAN_POINT('Ctrl Pts',(17.7466129424125,-0.813384860531917,
119.770227025735));
#52208=CARTESIAN_POINT('Ctrl Pts',(18.0058293990763,-0.978443247176416,
119.789184216853));
#52209=CARTESIAN_POINT('Ctrl Pts',(18.2933141133492,-1.08617062167036,119.808122253429));
#52210=CARTESIAN_POINT('Ctrl Pts',(18.6825508024836,-1.10253496953756,119.831759004564));
#52211=CARTESIAN_POINT('Ctrl Pts',(19.1161093341978,-0.929908145532468,
119.860070187335));
#52212=CARTESIAN_POINT('Ctrl Pts',(19.4407832828235,-0.59588973771539,119.888332066323));
#52213=CARTESIAN_POINT('Ctrl Pts',(19.6004637023044,-0.159071451104862,
119.916548585756));
#52214=CARTESIAN_POINT('Ctrl Pts',(19.5678525962247,0.304175161164362,119.94472356439));
#52215=CARTESIAN_POINT('Ctrl Pts',(19.3491799377188,0.713159074225391,119.972860943747));
#52216=CARTESIAN_POINT('Ctrl Pts',(18.9829635246229,0.996826194546356,120.000964621022));
#52217=CARTESIAN_POINT('Ctrl Pts',(18.5333246059365,1.10605246133314,120.029038590895));
#52218=CARTESIAN_POINT('Ctrl Pts',(18.0786639414332,1.02221007217602,120.057086755249));
#52219=CARTESIAN_POINT('Ctrl Pts',(17.7616747610674,0.803810507414772,120.08044215356));
#52220=CARTESIAN_POINT('Ctrl Pts',(17.5781706881473,0.563020021594781,120.099117557111));
#52221=CARTESIAN_POINT('Ctrl Pts',(17.4485102894162,0.289546062171738,120.117787596985));
#52222=CARTESIAN_POINT('Ctrl Pts',(17.4000766883178,-0.0919110956988218,
120.141116750007));
#52223=CARTESIAN_POINT('Ctrl Pts',(17.5340026995979,-0.533317467951709,
120.169101926724));
#52224=CARTESIAN_POINT('Ctrl Pts',(17.8364514864612,-0.881453389642329,
120.197081436934));
#52225=CARTESIAN_POINT('Ctrl Pts',(18.2546972918622,-1.07569505981494,120.225059261169));
#52226=CARTESIAN_POINT('Ctrl Pts',(18.7158361983992,-1.08216853743163,120.253039487099));
#52227=CARTESIAN_POINT('Ctrl Pts',(19.1395027643609,-0.899695026965587,
120.281026122395));
#52228=CARTESIAN_POINT('Ctrl Pts',(19.4518086127432,-0.559968571162895,
120.309023214945));
#52229=CARTESIAN_POINT('Ctrl Pts',(19.5981997788132,-0.122089063377897,
120.33703477985));
#52230=CARTESIAN_POINT('Ctrl Pts',(19.552950474692,0.337696943191307,120.36506483566));
#52231=CARTESIAN_POINT('Ctrl Pts',(19.3236731730684,0.739225257076302,120.393117382629));
#52232=CARTESIAN_POINT('Ctrl Pts',(18.9500423513974,1.01234988098468,120.421196409681));
#52233=CARTESIAN_POINT('Ctrl Pts',(18.4969528285068,1.10915757122897,120.449305885466));
#52234=CARTESIAN_POINT('Ctrl Pts',(18.0432838645376,1.0123484532541,120.477449757804));
#52235=CARTESIAN_POINT('Ctrl Pts',(17.6682096728875,0.738317035565853,120.505631950467));
#52236=CARTESIAN_POINT('Ctrl Pts',(17.437423751279,0.334387982344825,120.533856363023));
#52237=CARTESIAN_POINT('Ctrl Pts',(17.3916675325301,-0.129330292288387,
120.562126866275));
#52238=CARTESIAN_POINT('Ctrl Pts',(17.5395597076022,-0.572076137360996,
120.590447299692));
#52239=CARTESIAN_POINT('Ctrl Pts',(17.855984803406,-0.916457888564851,120.618821467709));
#52240=CARTESIAN_POINT('Ctrl Pts',(18.2863409307668,-1.10194268406267,120.647253137918));
#52241=CARTESIAN_POINT('Ctrl Pts',(18.7559322318109,-1.09546592268358,120.67574604072));
#52242=CARTESIAN_POINT('Ctrl Pts',(19.1828951657191,-0.897307355511358,
120.704303864294));
#52243=CARTESIAN_POINT('Ctrl Pts',(19.4924290395271,-0.541191746237481,
120.732930254292));
#52244=CARTESIAN_POINT('Ctrl Pts',(19.629864127016,-0.0885718616664442,
120.761628805457));
#52245=CARTESIAN_POINT('Ctrl Pts',(19.5702915902,0.38194575566233,120.790403069716));
#52246=CARTESIAN_POINT('Ctrl Pts',(19.3230606442279,0.788211584401149,120.81925653667));
#52247=CARTESIAN_POINT('Ctrl Pts',(18.9303370039179,1.05884354017487,120.848192665372));
#52248=CARTESIAN_POINT('Ctrl Pts',(18.4599333444905,1.14572580145235,120.877214815781));
#52249=CARTESIAN_POINT('Ctrl Pts',(17.9936381567603,1.03256046278807,120.906326368603));
#52250=CARTESIAN_POINT('Ctrl Pts',(17.6130217950625,0.737867413805891,120.935530493837));
#52251=CARTESIAN_POINT('Ctrl Pts',(17.3852199880608,0.312046699813544,120.964830580706));
#52252=CARTESIAN_POINT('Ctrl Pts',(17.3510866111027,-0.171347529488756,
120.994229417955));
#52253=CARTESIAN_POINT('Ctrl Pts',(17.4762315523886,-0.513852621030988,
121.016355467724));
#52254=CARTESIAN_POINT('Ctrl Pts',(17.6138033107167,-0.708894863435242,
121.031138486187));
#52255=CARTESIAN_POINT('Ctrl Pts',(17.7186460182362,-0.828728920899541,
121.041003185243));
#52256=CARTESIAN_POINT('Ctrl Pts',(17.9338771397665,-1.00822503331039,121.058288970429));
#52257=CARTESIAN_POINT('Ctrl Pts',(18.3129598588467,-1.15930959599405,121.083050806596));
#52258=CARTESIAN_POINT('Ctrl Pts',(18.8041703554433,-1.13879633990496,121.112875718073));
#52259=CARTESIAN_POINT('Ctrl Pts',(19.2457859888915,-0.918670752954191,
121.142814329296));
#52260=CARTESIAN_POINT('Ctrl Pts',(19.5602240335785,-0.535856279758148,
121.172869253422));
#52261=CARTESIAN_POINT('Ctrl Pts',(19.6913854815473,-0.0561259788657527,
121.203043167138));
#52262=CARTESIAN_POINT('Ctrl Pts',(19.6148686833085,0.437325039991343,121.233338591474));
#52263=CARTESIAN_POINT('Ctrl Pts',(19.3423661747877,0.858198271022791,121.263758005378));
#52264=CARTESIAN_POINT('Ctrl Pts',(18.9199837839974,1.13220110886314,121.294303783052));
#52265=CARTESIAN_POINT('Ctrl Pts',(18.42042918257,1.21011500633407,121.32497822383));
#52266=CARTESIAN_POINT('Ctrl Pts',(17.9305393050093,1.07662958513204,121.355783533596));
#52267=CARTESIAN_POINT('Ctrl Pts',(17.5362003747735,0.753305442664608,121.386721831682));
#52268=CARTESIAN_POINT('Ctrl Pts',(17.3073177623713,0.295125520361277,121.417795146862));
#52269=CARTESIAN_POINT('Ctrl Pts',(17.2854401515084,-0.218834434459951,
121.449005416441));
#52270=CARTESIAN_POINT('Ctrl Pts',(17.4762374736664,-0.699031393505859,
121.480354486252));
#52271=CARTESIAN_POINT('Ctrl Pts',(17.8481867637241,-1.06103365410968,121.511844103753));
#52272=CARTESIAN_POINT('Ctrl Pts',(18.3377536992966,-1.24035134890439,121.543475928373));
#52273=CARTESIAN_POINT('Ctrl Pts',(18.8602278069233,-1.20390349087577,121.575251508684));
#52274=CARTESIAN_POINT('Ctrl Pts',(19.3243579160287,-0.956110272282689,
121.607172324249));
#52275=CARTESIAN_POINT('Ctrl Pts',(19.6482814584831,-0.538442349648599,
121.63923970298));
#52276=CARTESIAN_POINT('Ctrl Pts',(19.7739347309703,-0.0225425683993542,
121.671454972332));
#52277=CARTESIAN_POINT('Ctrl Pts',(19.6774652298788,0.502115753058099,121.703819199622));
#52278=CARTESIAN_POINT('Ctrl Pts',(19.3737224989186,0.943640496909592,121.736333532426));
#52279=CARTESIAN_POINT('Ctrl Pts',(18.9140030444815,1.22389593147418,121.768998887406));
#52280=CARTESIAN_POINT('Ctrl Pts',(18.377429165599,1.29225269519424,121.801816130025));
#52281=CARTESIAN_POINT('Ctrl Pts',(17.8573241502507,1.13475923997334,121.834786019857));
#52282=CARTESIAN_POINT('Ctrl Pts',(17.4450010757071,0.776910878603483,121.867909199878));
#52283=CARTESIAN_POINT('Ctrl Pts',(17.2137312599202,0.279562992177936,121.901186219253));
#52284=CARTESIAN_POINT('Ctrl Pts',(17.2057348606295,-0.2714116808315,121.934617523114));
#52285=CARTESIAN_POINT('Ctrl Pts',(17.4244858838036,-0.779938810205246,
121.968203442992));
#52286=CARTESIAN_POINT('Ctrl Pts',(17.8337421937975,-1.15649409223492,122.001944217451));
#52287=CARTESIAN_POINT('Ctrl Pts',(18.3635288783225,-1.33385851932845,122.035839968655));
#52288=CARTESIAN_POINT('Ctrl Pts',(18.9220955048508,-1.27911558981949,122.069890723435));
#52289=CARTESIAN_POINT('Ctrl Pts',(19.4118031026727,-0.999736384496644,
122.104096394088));
#52290=CARTESIAN_POINT('Ctrl Pts',(19.7461944871727,-0.542647687182364,
122.138456799284));
#52291=CARTESIAN_POINT('Ctrl Pts',(19.8652556008789,0.013647933341159,122.172971637033));
#52292=CARTESIAN_POINT('Ctrl Pts',(19.7461888829058,0.572532365852113,122.207640521162));
#52293=CARTESIAN_POINT('Ctrl Pts',(19.4077323355963,1.03609396929577,122.242462929572));
#52294=CARTESIAN_POINT('Ctrl Pts',(18.9072812151109,1.322227313061,122.277438289026));
#52295=CARTESIAN_POINT('Ctrl Pts',(18.3310963479423,1.37923683565688,122.312565853708));
#52296=CARTESIAN_POINT('Ctrl Pts',(17.7795212835281,1.19516070447226,122.34784483257));
#52297=CARTESIAN_POINT('Ctrl Pts',(17.3494069677128,0.800134075483034,122.38327430115));
#52298=CARTESIAN_POINT('Ctrl Pts',(17.1171842054199,0.261691707489099,122.418853238197));
#52299=CARTESIAN_POINT('Ctrl Pts',(17.1242829390838,-0.261793907771907,
122.450610839665));
#52300=CARTESIAN_POINT('Ctrl Pts',(17.2865889445715,-0.685649920943017,
122.478494089534));
#52301=CARTESIAN_POINT('Ctrl Pts',(17.5985838897628,-1.10207969945623,122.510447354666));
#52302=CARTESIAN_POINT('Ctrl Pts',(18.18666838241,-1.42792122315664,122.550550404142));
#52303=CARTESIAN_POINT('Ctrl Pts',(18.9968853221201,-1.38299738205048,122.598929027424));
#52304=CARTESIAN_POINT('Ctrl Pts',(19.6622552549554,-0.911544492503412,
122.647558773599));
#52305=CARTESIAN_POINT('Ctrl Pts',(19.9764902272409,-0.154570377655717,
122.696435587038));
#52306=CARTESIAN_POINT('Ctrl Pts',(19.8390738237385,0.657775266502406,122.74555504686));
#52307=CARTESIAN_POINT('Ctrl Pts',(19.3797620617075,1.17210955074175,122.786686268123));
#52308=CARTESIAN_POINT('Ctrl Pts',(18.8884735110166,1.39088302497454,122.819707738936));
#52309=CARTESIAN_POINT('Ctrl Pts',(18.5033111211165,1.44583087334473,122.843612041481));
#52310=CARTESIAN_POINT('Ctrl Pts',(18.1319627148124,1.39887538222455,122.866646747491));
#52311=CARTESIAN_POINT('Ctrl Pts',(17.6848506292388,1.22425836285374,122.896190503993));
#52312=CARTESIAN_POINT('Ctrl Pts',(17.2330030000641,0.805544093152841,122.933230312885));
#52313=CARTESIAN_POINT('Ctrl Pts',(17.0358813147302,0.219439642783941,122.970413341592));
#52314=CARTESIAN_POINT('Ctrl Pts',(17.0608067523446,-0.264630775831841,
123.000243864343));
#52315=CARTESIAN_POINT('Ctrl Pts',(17.2030640210597,-0.72877788689057,123.030129409407));
#52316=CARTESIAN_POINT('Ctrl Pts',(17.5912103662842,-1.21622770551833,123.067588736755));
#52317=CARTESIAN_POINT('Ctrl Pts',(18.2248499897429,-1.48333671290741,123.108939586315));
#52318=CARTESIAN_POINT('Ctrl Pts',(18.8430841455309,-1.45988936207864,123.146643846141));
#52319=CARTESIAN_POINT('Ctrl Pts',(19.35464113493,-1.23705318214091,123.180662420129));
#52320=CARTESIAN_POINT('Ctrl Pts',(19.7503526751607,-0.841413044968066,
123.214763669378));
#52321=CARTESIAN_POINT('Ctrl Pts',(19.9747043163627,-0.327540003001533,
123.248945585414));
#52322=CARTESIAN_POINT('Ctrl Pts',(19.9958554010032,0.234190739582267,123.283205786453));
#52323=CARTESIAN_POINT('Ctrl Pts',(19.809886470046,0.765886840091164,123.31754245384));
#52324=CARTESIAN_POINT('Ctrl Pts',(19.503128994245,1.12261086723232,123.346217672991));
#52325=CARTESIAN_POINT('Ctrl Pts',(19.1916465195094,1.32604725655206,123.369194036914));
#52326=CARTESIAN_POINT('Ctrl Pts',(18.7905766269883,1.49297621000668,123.396027008284));
#52327=CARTESIAN_POINT('Ctrl Pts',(18.1844752698309,1.52349251558905,123.432510323781));
#52328=CARTESIAN_POINT('Ctrl Pts',(17.6076908763952,1.24575162694292,123.471012023267));
#52329=CARTESIAN_POINT('Ctrl Pts',(17.2669358073587,0.877725128070975,123.501869301326));
#52330=CARTESIAN_POINT('Ctrl Pts',(17.0870893744063,0.547329694514233,123.525039768527));
#52331=CARTESIAN_POINT('Ctrl Pts',(16.9622603091664,0.0602367962628432,
123.555968827903));
#52332=CARTESIAN_POINT('Ctrl Pts',(17.0342291378425,-0.514571727658781,
123.590822340935));
#52333=CARTESIAN_POINT('Ctrl Pts',(17.3733949645324,-1.05353060709449,123.629619294211));
#52334=CARTESIAN_POINT('Ctrl Pts',(17.8538625057619,-1.40857439093685,123.666045889573));
#52335=CARTESIAN_POINT('Ctrl Pts',(18.461592831455,-1.5564523426571,123.703986589641));
#52336=CARTESIAN_POINT('Ctrl Pts',(19.101195146309,-1.43859456950387,123.743445712838));
#52337=CARTESIAN_POINT('Ctrl Pts',(19.5929149609134,-1.10003231948515,123.77966722315));
#52338=CARTESIAN_POINT('Ctrl Pts',(19.8356254005539,-0.74441967000705,123.806040285316));
#52339=CARTESIAN_POINT('Ctrl Pts',(19.9703654530638,-0.416005980207952,
123.828031369899));
#52340=CARTESIAN_POINT('Ctrl Pts',(20.0368072594968,-0.0822239677629709,
123.848934198666));
#52341=CARTESIAN_POINT('Ctrl Pts',(20.0006566043124,0.346454692026937,123.875358332762));
#52342=CARTESIAN_POINT('Ctrl Pts',(19.8471547497178,0.748660819823204,123.901800955164));
#52343=CARTESIAN_POINT('Ctrl Pts',(19.5881175815438,1.09289552386003,123.928261650183));
#52344=CARTESIAN_POINT('Ctrl Pts',(19.2437140701204,1.35209703835508,123.954738785435));
#52345=CARTESIAN_POINT('Ctrl Pts',(18.8743120378708,1.49315805935625,123.97902361159));
#52346=CARTESIAN_POINT('Ctrl Pts',(18.5188213115279,1.53557171478921,124.001111261365));
#52347=CARTESIAN_POINT('Ctrl Pts',(18.0907023088825,1.49677336723877,124.027626520082));
#52348=CARTESIAN_POINT('Ctrl Pts',(17.5886989835531,1.28071224384361,124.060787965071));
#52349=CARTESIAN_POINT('Ctrl Pts',(17.1445191175465,0.797474344906156,124.10060608365));
#52350=CARTESIAN_POINT('Ctrl Pts',(16.9363317375956,0.174754912879289,124.140444286067));
#52351=CARTESIAN_POINT('Ctrl Pts',(17.000693693818,-0.479009409878407,124.180298719382));
#52352=CARTESIAN_POINT('Ctrl Pts',(17.3265672215966,-1.04960547491672,124.220165279827));
#52353=CARTESIAN_POINT('Ctrl Pts',(17.8571916910488,-1.43742494106541,124.260039981735));
#52354=CARTESIAN_POINT('Ctrl Pts',(18.5000049546241,-1.57468781447863,124.299918766618));
#52355=CARTESIAN_POINT('Ctrl Pts',(19.142818830386,-1.43742342812486,124.339797610578));
#52356=CARTESIAN_POINT('Ctrl Pts',(19.6734460569893,-1.04960765164736,124.379672470623));
#52357=CARTESIAN_POINT('Ctrl Pts',(19.9993212502782,-0.478996882985747,
124.419539315287));
#52358=CARTESIAN_POINT('Ctrl Pts',(20.063685387175,0.17475275129412,124.459394112919));
#52359=CARTESIAN_POINT('Ctrl Pts',(19.855493029657,0.79751985498053,124.499232843074));
#52360=CARTESIAN_POINT('Ctrl Pts',(19.4113116700434,1.28068814713101,124.539051495894));
#52361=CARTESIAN_POINT('Ctrl Pts',(18.8088847361186,1.54012930695157,124.57884607634));
#52362=CARTESIAN_POINT('Ctrl Pts',(18.1534946893475,1.53088466548527,124.618612603657));
#52363=CARTESIAN_POINT('Ctrl Pts',(17.5595230439077,1.25497200645252,124.658347116273));
#52364=CARTESIAN_POINT('Ctrl Pts',(17.1304444180403,0.760962163490976,124.698045674236));
#52365=CARTESIAN_POINT('Ctrl Pts',(16.940761355013,0.135410421294839,124.73770436324));
#52366=CARTESIAN_POINT('Ctrl Pts',(17.0230407297764,-0.51234136906881,124.77731929645));
#52367=CARTESIAN_POINT('Ctrl Pts',(17.3623119928872,-1.0693180342063,124.81688661527));
#52368=CARTESIAN_POINT('Ctrl Pts',(17.8987924872961,-1.43865725028846,124.856402493113));
#52369=CARTESIAN_POINT('Ctrl Pts',(18.5384432864047,-1.55649001223549,124.89586313845));
#52370=CARTESIAN_POINT('Ctrl Pts',(19.1694876783657,-1.40300740644741,124.935264798184));
#52371=CARTESIAN_POINT('Ctrl Pts',(19.6819844911938,-1.00579246197517,124.974603759877));
#52372=CARTESIAN_POINT('Ctrl Pts',(19.9870215554236,-0.434856710408076,
125.013876352219));
#52373=CARTESIAN_POINT('Ctrl Pts',(20.0321717618401,0.209724078121503,125.053078948617));
#52374=CARTESIAN_POINT('Ctrl Pts',(19.8105195361387,0.815386929581868,125.092207970087));
#52375=CARTESIAN_POINT('Ctrl Pts',(19.361701163962,1.27677787532468,125.131259888399));
#52376=CARTESIAN_POINT('Ctrl Pts',(18.7648066215825,1.5141139501787,125.170231228365));
#52377=CARTESIAN_POINT('Ctrl Pts',(18.1244162904329,1.48700453469375,125.209118568196));
#52378=CARTESIAN_POINT('Ctrl Pts',(17.5522425067462,1.20133350244083,125.247918542709));
#52379=CARTESIAN_POINT('Ctrl Pts',(17.1476050430654,0.708028317127927,125.286627846152));
#52380=CARTESIAN_POINT('Ctrl Pts',(16.9801594170711,0.0939676037639261,
125.325243234936));
#52381=CARTESIAN_POINT('Ctrl Pts',(17.0778869149266,-0.533346746909132,
125.363761529995));
#52382=CARTESIAN_POINT('Ctrl Pts',(17.4224200985157,-1.0646435628828,125.402179617076));
#52383=CARTESIAN_POINT('Ctrl Pts',(17.9524839925264,-1.40794981777256,125.440494449376));
#52384=CARTESIAN_POINT('Ctrl Pts',(18.5748095291292,-1.50453836038642,125.47870305043));
#52385=CARTESIAN_POINT('Ctrl Pts',(19.1805722495993,-1.33898635608767,125.516802516252));
#52386=CARTESIAN_POINT('Ctrl Pts',(19.6644539096247,-0.941619949238724,
125.554790017782));
#52387=CARTESIAN_POINT('Ctrl Pts',(19.9429825043806,-0.382961689893696,
125.592662801021));
#52388=CARTESIAN_POINT('Ctrl Pts',(19.9689520201468,0.2388025468179,125.630418189203));
#52389=CARTESIAN_POINT('Ctrl Pts',(19.7394275641386,0.815106336169562,125.668053585541));
#52390=CARTESIAN_POINT('Ctrl Pts',(19.2959782023475,1.24598811837169,125.705566474907));
#52391=CARTESIAN_POINT('Ctrl Pts',(18.7171464460761,1.45745420294917,125.742954426178));
#52392=CARTESIAN_POINT('Ctrl Pts',(18.1045195341734,1.41419939899926,125.780215092177));
#52393=CARTESIAN_POINT('Ctrl Pts',(17.5648760765932,1.12549636275945,125.817346211604));
#52394=CARTESIAN_POINT('Ctrl Pts',(17.1915502824867,0.643272766242982,125.854345611245));
#52395=CARTESIAN_POINT('Ctrl Pts',(17.0482705064466,0.0527665519465494,
125.891211207534));
#52396=CARTESIAN_POINT('Ctrl Pts',(17.1582735037444,-0.54255765424983,125.927941008396));
#52397=CARTESIAN_POINT('Ctrl Pts',(17.5005545415035,-1.03915845752618,125.964533113257));
#52398=CARTESIAN_POINT('Ctrl Pts',(18.0138543548987,-1.35144610286629,126.000985714488));
#52399=CARTESIAN_POINT('Ctrl Pts',(18.6076292011844,-1.42654679770189,126.037297099343));
#52400=CARTESIAN_POINT('Ctrl Pts',(19.1780377234228,-1.25325431972676,126.073465651058));
#52401=CARTESIAN_POINT('Ctrl Pts',(19.6261188945682,-0.863654225443849,
126.109489850372));
#52402=CARTESIAN_POINT('Ctrl Pts',(19.8749757363862,-0.327195816840043,
126.145368275421));
#52403=CARTESIAN_POINT('Ctrl Pts',(19.8829785376702,0.261694286094789,126.181099602915));
#52404=CARTESIAN_POINT('Ctrl Pts',(19.650719858024,0.800245939977902,126.216682609493));
#52405=CARTESIAN_POINT('Ctrl Pts',(19.220561895408,1.19529383673981,126.252116172656));
#52406=CARTESIAN_POINT('Ctrl Pts',(18.6689174524219,1.37940357614657,126.287399271635));
#52407=CARTESIAN_POINT('Ctrl Pts',(18.0926704275284,1.32238292183252,126.322530987377));
#52408=CARTESIAN_POINT('Ctrl Pts',(17.5921506137728,1.03621366175272,126.357510503253));
#52409=CARTESIAN_POINT('Ctrl Pts',(17.2536567723353,0.572602926071189,126.392337106094));
#52410=CARTESIAN_POINT('Ctrl Pts',(17.1345737699536,0.0136453744042972,
126.427010186614));
#52411=CARTESIAN_POINT('Ctrl Pts',(17.2536504364034,-0.542717522157398,
126.461529239891));
#52412=CARTESIAN_POINT('Ctrl Pts',(17.5880834324056,-0.999864641603807,
126.495893865198));
#52413=CARTESIAN_POINT('Ctrl Pts',(18.0778530411477,-1.27927849056268,126.530103766427));
#52414=CARTESIAN_POINT('Ctrl Pts',(18.6364904459868,-1.33402870614301,126.564158752655));
#52415=CARTESIAN_POINT('Ctrl Pts',(19.1663446909442,-1.15664138180575,126.598058738222));
#52416=CARTESIAN_POINT('Ctrl Pts',(19.5756533377215,-0.78003806942924,126.631803742641));
#52417=CARTESIAN_POINT('Ctrl Pts',(19.794432443157,-0.271445460467721,126.665393890358));
#52418=CARTESIAN_POINT('Ctrl Pts',(19.7864349006516,0.27959998319499,126.69882941077));
#52419=CARTESIAN_POINT('Ctrl Pts',(19.5551353092926,0.777012272782376,126.732110638587));
#52420=CARTESIAN_POINT('Ctrl Pts',(19.1427587398274,1.13490641725472,126.765238013014));
#52421=CARTESIAN_POINT('Ctrl Pts',(18.6225867432735,1.29242086659805,126.798212078173));
#52422=CARTESIAN_POINT('Ctrl Pts',(18.0859430362728,1.22405396241437,126.831033480681));
#52423=CARTESIAN_POINT('Ctrl Pts',(17.6261649865072,0.943764553716469,126.863702973114));
#52424=CARTESIAN_POINT('Ctrl Pts',(17.3223818224607,0.502178353438225,126.896221407178));
#52425=CARTESIAN_POINT('Ctrl Pts',(17.2259017352908,-0.0225383357424905,
126.92858974499));
#52426=CARTESIAN_POINT('Ctrl Pts',(17.3515757437269,-0.538512892512059,
126.960809035826));
#52427=CARTESIAN_POINT('Ctrl Pts',(17.6755338947518,-0.956225990676644,
126.992880456677));
#52428=CARTESIAN_POINT('Ctrl Pts',(18.1397311835696,-1.20405787590894,127.024805234591));
#52429=CARTESIAN_POINT('Ctrl Pts',(18.6622539843598,-1.24049861448516,127.056584791087));
#52430=CARTESIAN_POINT('Ctrl Pts',(19.1519117947061,-1.06117933724715,127.088220467932));
#52431=CARTESIAN_POINT('Ctrl Pts',(19.4618550662539,-0.759439290617938,
127.114465119351));
#52432=CARTESIAN_POINT('Ctrl Pts',(19.6193300865727,-0.459005379949352,
127.135390361088));
#52433=CARTESIAN_POINT('Ctrl Pts',(19.7110223729966,-0.133185783680743,
127.156269267074));
#52434=CARTESIAN_POINT('Ctrl Pts',(19.6928503715007,0.295153408660477,127.182280859505));
#52435=CARTESIAN_POINT('Ctrl Pts',(19.4639046032388,0.753395195664358,127.213357950153));
#52436=CARTESIAN_POINT('Ctrl Pts',(19.0695377246349,1.07675375085461,127.244299876378));
#52437=CARTESIAN_POINT('Ctrl Pts',(18.5795803461416,1.21025686910366,127.275108807355));
#52438=CARTESIAN_POINT('Ctrl Pts',(18.0799738634865,1.13233247683963,127.305786783584));
#52439=CARTESIAN_POINT('Ctrl Pts',(17.6575395077607,0.858299579569359,127.336336050748));
#52440=CARTESIAN_POINT('Ctrl Pts',(17.3850098668066,0.437377398955207,127.366758880445));
#52441=CARTESIAN_POINT('Ctrl Pts',(17.3084803074032,-0.0561256639258518,
127.39705766334));
#52442=CARTESIAN_POINT('Ctrl Pts',(17.439663243693,-0.535912780145553,127.427234856148));
#52443=CARTESIAN_POINT('Ctrl Pts',(17.7541222443087,-0.918759596678555,
127.45729300688));
#52444=CARTESIAN_POINT('Ctrl Pts',(18.1958079698188,-1.13892417265509,127.487234739106));
#52445=CARTESIAN_POINT('Ctrl Pts',(18.6870232674475,-1.15940871276915,127.517062760317));
#52446=CARTESIAN_POINT('Ctrl Pts',(19.1420662103094,-0.978153105648501,
127.546779850572));
#52447=CARTESIAN_POINT('Ctrl Pts',(19.4821508736072,-0.628126893328401,
127.576388872373));
#52448=CARTESIAN_POINT('Ctrl Pts',(19.6490175278053,-0.171352587712298,
127.605892744728));
#52449=CARTESIAN_POINT('Ctrl Pts',(19.6148875667895,0.312060165323532,127.635294496316));
#52450=CARTESIAN_POINT('Ctrl Pts',(19.387060763882,0.737933090385993,127.664597137408));
#52451=CARTESIAN_POINT('Ctrl Pts',(19.0064135995696,1.03264512775516,127.69380393404));
#52452=CARTESIAN_POINT('Ctrl Pts',(18.5400762875866,1.14582302109237,127.722917848391));
#52453=CARTESIAN_POINT('Ctrl Pts',(18.069635799574,1.05893307361866,127.751942612257));
#52454=CARTESIAN_POINT('Ctrl Pts',(17.6768791166838,0.788277917073556,127.780880584301));
#52455=CARTESIAN_POINT('Ctrl Pts',(17.4296332142809,0.381982697626676,127.809737248291));
#52456=CARTESIAN_POINT('Ctrl Pts',(17.3700415360265,-0.0885703605568786,
127.838511718406));
#52457=CARTESIAN_POINT('Ctrl Pts',(17.507531797481,-0.541218118675741,127.867215509699));
#52458=CARTESIAN_POINT('Ctrl Pts',(17.816984019384,-0.897377443387583,127.895838832972));
#52459=CARTESIAN_POINT('Ctrl Pts',(18.244166417509,-1.09549488656034,127.924406623306));
#52460=CARTESIAN_POINT('Ctrl Pts',(18.7134661788609,-1.10209796420226,127.952885817208));
#52461=CARTESIAN_POINT('Ctrl Pts',(19.1442712717119,-0.916283636031154,
127.981348904678));
#52462=CARTESIAN_POINT('Ctrl Pts',(19.460485405136,-0.572567145982761,128.009677920323));
#52463=CARTESIAN_POINT('Ctrl Pts',(19.6077409437319,-0.12891228120585,128.038041366258));
#52464=CARTESIAN_POINT('Ctrl Pts',(19.571105117469,0.257508093441198,128.061628433663));
#52465=CARTESIAN_POINT('Ctrl Pts',(19.4479991183959,0.535304279391785,128.080339688794));
#52466=CARTESIAN_POINT('Ctrl Pts',(19.3125791070956,0.722042855063143,128.094494421635));
#52467=CARTESIAN_POINT('Ctrl Pts',(19.141797922151,0.876422884225493,128.108678534636));
#52468=CARTESIAN_POINT('Ctrl Pts',(18.9477421547559,0.990014057708069,128.122740918746));
#52469=CARTESIAN_POINT('Ctrl Pts',(18.7367548382266,1.05934633488113,128.136684558088));
#52470=CARTESIAN_POINT('Ctrl Pts',(18.582539945268,1.07619894693391,128.146145491089));
#52471=CARTESIAN_POINT('Ctrl Pts',(18.5011390454481,1.07688406432642,128.150964169306));
#52472=CARTESIAN_POINT('Ctrl Pts',(18.5048905446611,1.0769826448063,112.950906422413));
#52473=CARTESIAN_POINT('Ctrl Pts',(18.3830098066567,1.07595682551458,112.958121380168));
#52474=CARTESIAN_POINT('Ctrl Pts',(18.2332489107013,1.05152251268125,112.967474141999));
#52475=CARTESIAN_POINT('Ctrl Pts',(18.0268596028074,0.971442179610211,112.981411102263));
#52476=CARTESIAN_POINT('Ctrl Pts',(17.8656334975826,0.876962742492602,112.993100991851));
#52477=CARTESIAN_POINT('Ctrl Pts',(17.6954686455205,0.723186909327924,113.007230605468));
#52478=CARTESIAN_POINT('Ctrl Pts',(17.5608075681054,0.537408101995845,113.021310819524));
#52479=CARTESIAN_POINT('Ctrl Pts',(17.4385635814574,0.261558152501724,113.039890602226));
#52480=CARTESIAN_POINT('Ctrl Pts',(17.4023331932359,-0.121639614718659,
113.063280373129));
#52481=CARTESIAN_POINT('Ctrl Pts',(17.5481112006283,-0.560471337755449,
113.091337893366));
#52482=CARTESIAN_POINT('Ctrl Pts',(17.8601965720909,-0.899510546216632,
113.119288341739));
#52483=CARTESIAN_POINT('Ctrl Pts',(18.2843287346396,-1.08233432237433,113.147308243339));
#52484=CARTESIAN_POINT('Ctrl Pts',(18.7451740809681,-1.0757227904068,113.175274045851));
#52485=CARTESIAN_POINT('Ctrl Pts',(19.1636363346921,-0.881531337437797,
113.203262131254));
#52486=CARTESIAN_POINT('Ctrl Pts',(19.4659983852052,-0.53335175821849,113.231237553952));
#52487=CARTESIAN_POINT('Ctrl Pts',(19.5999624515289,-0.0919352051397887,
113.259227393613));
#52488=CARTESIAN_POINT('Ctrl Pts',(19.5418755258235,0.36583827782248,113.28722106912));
#52489=CARTESIAN_POINT('Ctrl Pts',(19.3017885872034,0.760159580845085,113.315231457202));
#52490=CARTESIAN_POINT('Ctrl Pts',(18.9213424421171,1.02219956875272,113.343257793308));
#52491=CARTESIAN_POINT('Ctrl Pts',(18.4667053085281,1.10606223937008,113.371306390066));
#52492=CARTESIAN_POINT('Ctrl Pts',(18.0170529864695,0.996825804229037,113.399380178387));
#52493=CARTESIAN_POINT('Ctrl Pts',(17.6508486223648,0.71316562605935,113.427483635222));
#52494=CARTESIAN_POINT('Ctrl Pts',(17.432175698002,0.304188605160904,113.455620456518));
#52495=CARTESIAN_POINT('Ctrl Pts',(17.3995688929116,-0.159048710866342,
113.483794694377));
#52496=CARTESIAN_POINT('Ctrl Pts',(17.5592416108375,-0.595843498412212,
113.512010220208));
#52497=CARTESIAN_POINT('Ctrl Pts',(17.8839047765297,-0.929863593703113,
113.5402708761));
#52498=CARTESIAN_POINT('Ctrl Pts',(18.3174363420886,-1.10244895914806,113.568580611988));
#52499=CARTESIAN_POINT('Ctrl Pts',(18.7845032234939,-1.08288015874688,113.596943024728));
#52500=CARTESIAN_POINT('Ctrl Pts',(19.2036958810281,-0.873830234443041,
113.625362225695));
#52501=CARTESIAN_POINT('Ctrl Pts',(19.5015677804977,-0.511035220651307,
113.653841612173));
#52502=CARTESIAN_POINT('Ctrl Pts',(19.625569402385,-0.057210726531146,113.682385109334));
#52503=CARTESIAN_POINT('Ctrl Pts',(19.5532262978395,0.408801574029359,113.710996276871));
#52504=CARTESIAN_POINT('Ctrl Pts',(19.2962196078634,0.805590455062962,113.739678701328));
#52505=CARTESIAN_POINT('Ctrl Pts',(18.8985263284912,1.06350860478144,113.768436045941));
#52506=CARTESIAN_POINT('Ctrl Pts',(18.5071722498531,1.12444142266846,113.792465688214));
#52507=CARTESIAN_POINT('Ctrl Pts',(18.1989776345572,1.07400338365928,113.811730434757));
#52508=CARTESIAN_POINT('Ctrl Pts',(17.9074645018029,0.960739376980088,113.831023029996));
#52509=CARTESIAN_POINT('Ctrl Pts',(17.5994270430112,0.70815915760555,113.855191843742));
#52510=CARTESIAN_POINT('Ctrl Pts',(17.3852129809237,0.279151779569495,113.884283163333));
#52511=CARTESIAN_POINT('Ctrl Pts',(17.3648125841006,-0.201413575017571,
113.913466255147));
#52512=CARTESIAN_POINT('Ctrl Pts',(17.543062918984,-0.649872702566433,113.942744420078));
#52513=CARTESIAN_POINT('Ctrl Pts',(17.8900876353479,-0.987536991035994,
113.972120816461));
#52514=CARTESIAN_POINT('Ctrl Pts',(18.3463327148162,-1.15459443856777,114.001598506433));
#52515=CARTESIAN_POINT('Ctrl Pts',(18.8327332303177,-1.1206124571982,114.031180517165));
#52516=CARTESIAN_POINT('Ctrl Pts',(19.2643943014772,-0.890100751175115,
114.06086982685));
#52517=CARTESIAN_POINT('Ctrl Pts',(19.5653719416265,-0.501947847935971,
114.09066925157));
#52518=CARTESIAN_POINT('Ctrl Pts',(19.6820042768537,-0.0229147496842619,
114.120581667901));
#52519=CARTESIAN_POINT('Ctrl Pts',(19.5924653448508,0.463866328892549,114.150609737823));
#52520=CARTESIAN_POINT('Ctrl Pts',(19.3108158047468,0.873213114754433,114.180756134765));
#52521=CARTESIAN_POINT('Ctrl Pts',(18.884827463517,1.13286962417431,114.211023428844));
#52522=CARTESIAN_POINT('Ctrl Pts',(18.3879247470357,1.19614313007461,114.241414092977));
#52523=CARTESIAN_POINT('Ctrl Pts',(17.9065295194458,1.05034460153068,114.271930535497));
#52524=CARTESIAN_POINT('Ctrl Pts',(17.525074544366,0.719258169043549,114.302575067548));
#52525=CARTESIAN_POINT('Ctrl Pts',(17.311212189731,0.259295019260713,114.333349916817));
#52526=CARTESIAN_POINT('Ctrl Pts',(17.3038340324676,-0.250078136447899,
114.364257227859));
#52527=CARTESIAN_POINT('Ctrl Pts',(17.5060302198135,-0.720090902958034,
114.395299041011));
#52528=CARTESIAN_POINT('Ctrl Pts',(17.8842069801639,-1.0680223900666,114.42647733462));
#52529=CARTESIAN_POINT('Ctrl Pts',(18.3736961688967,-1.23192189085238,114.457793936704));
#52530=CARTESIAN_POINT('Ctrl Pts',(18.8036898078691,-1.1897113502064,114.484007900284));
#52531=CARTESIAN_POINT('Ctrl Pts',(19.1159133168913,-1.05231178322972,114.50504993148));
#52532=CARTESIAN_POINT('Ctrl Pts',(19.3935460299567,-0.852827854344241,
114.526139457072));
#52533=CARTESIAN_POINT('Ctrl Pts',(19.6510131217686,-0.500999526556579,
114.55259106752));
#52534=CARTESIAN_POINT('Ctrl Pts',(19.7609905689121,0.0129651070626104,
114.584477754316));
#52535=CARTESIAN_POINT('Ctrl Pts',(19.650994915611,0.529347254895316,114.616510721381));
#52536=CARTESIAN_POINT('Ctrl Pts',(19.3382243340085,0.957748579656661,114.648691181518));
#52537=CARTESIAN_POINT('Ctrl Pts',(18.8756353988208,1.22224115354423,114.681020361715));
#52538=CARTESIAN_POINT('Ctrl Pts',(18.3429067772104,1.27497971988073,114.713499322237));
#52539=CARTESIAN_POINT('Ctrl Pts',(17.8327292020459,1.10472610803286,114.746129066567));
#52540=CARTESIAN_POINT('Ctrl Pts',(17.4347759656649,0.739278786151279,114.778910452807));
#52541=CARTESIAN_POINT('Ctrl Pts',(17.2197395303671,0.240806168981795,114.811844294554));
#52542=CARTESIAN_POINT('Ctrl Pts',(17.2263876359587,-0.243861224283583,
114.84125487901));
#52543=CARTESIAN_POINT('Ctrl Pts',(17.3765832012891,-0.636801446696335,
114.86708881416));
#52544=CARTESIAN_POINT('Ctrl Pts',(17.5394691336362,-0.853562773319375,
114.883747582543));
#52545=CARTESIAN_POINT('Ctrl Pts',(17.6708754828836,-0.975913973213227,
114.894874948331));
#52546=CARTESIAN_POINT('Ctrl Pts',(17.7406579614793,-1.03242891223486,114.90044288571));
#52547=CARTESIAN_POINT('Ctrl Pts',(17.8143583148267,-1.08390903483199,114.906015127139));
#52548=CARTESIAN_POINT('Ctrl Pts',(17.9686273982593,-1.17645090895374,114.917168135458));
#52549=CARTESIAN_POINT('Ctrl Pts',(18.2235871886093,-1.27381361087282,114.933929931012));
#52550=CARTESIAN_POINT('Ctrl Pts',(18.5872244681008,-1.30458106909559,114.956347672507));
#52551=CARTESIAN_POINT('Ctrl Pts',(18.9463768488907,-1.23322152774062,114.978834252193));
#52552=CARTESIAN_POINT('Ctrl Pts',(19.2725435869032,-1.06476481773121,115.001389672404));
#52553=CARTESIAN_POINT('Ctrl Pts',(19.5404655740093,-0.811742344080699,
115.024013960787));
#52554=CARTESIAN_POINT('Ctrl Pts',(19.7278646675296,-0.49361337321824,115.046707123689));
#52555=CARTESIAN_POINT('Ctrl Pts',(19.8523533513939,-0.0150590219413064,
115.077056466642));
#52556=CARTESIAN_POINT('Ctrl Pts',(19.7672800481721,0.488492784476201,115.107543396053));
#52557=CARTESIAN_POINT('Ctrl Pts',(19.5239217355454,0.851131103462418,115.134339669597));
#52558=CARTESIAN_POINT('Ctrl Pts',(19.3464502043358,1.02403675952917,115.149686032856));
#52559=CARTESIAN_POINT('Ctrl Pts',(19.1457347753392,1.17063466428336,115.165055294933));
#52560=CARTESIAN_POINT('Ctrl Pts',(18.9456442449245,1.26032940329247,115.178533337362));
#52561=CARTESIAN_POINT('Ctrl Pts',(18.7644374565501,1.30563923878879,115.190107211783));
#52562=CARTESIAN_POINT('Ctrl Pts',(18.6724851125622,1.32194107295301,115.195898442959));
#52563=CARTESIAN_POINT('Ctrl Pts',(18.5949991174864,1.33015007590669,115.20072800507));
#52564=CARTESIAN_POINT('Ctrl Pts',(18.5327430757371,1.33336828052772,115.204593820968));
#52565=CARTESIAN_POINT('Ctrl Pts',(18.2799794944861,1.33819961620997,115.220277475459));
#52566=CARTESIAN_POINT('Ctrl Pts',(17.8197716587963,1.22103049658674,115.2488239801));
#52567=CARTESIAN_POINT('Ctrl Pts',(17.4253298552619,0.855698560316531,115.281163584306));
#52568=CARTESIAN_POINT('Ctrl Pts',(17.2492366094994,0.524494113764414,115.304342264289));
#52569=CARTESIAN_POINT('Ctrl Pts',(17.1891919203476,0.346634023056757,115.315951203043));
#52570=CARTESIAN_POINT('Ctrl Pts',(17.1596329463037,0.199501998041167,115.325250098553));
#52571=CARTESIAN_POINT('Ctrl Pts',(17.1243035124897,-0.0987566443949158,
115.343863735336));
#52572=CARTESIAN_POINT('Ctrl Pts',(17.2116820602607,-0.595538227281773,
115.374199781352));
#52573=CARTESIAN_POINT('Ctrl Pts',(17.6490664555784,-1.14488189393693,115.416413259229));
#52574=CARTESIAN_POINT('Ctrl Pts',(18.2448545926823,-1.39619727372569,115.455299363107));
#52575=CARTESIAN_POINT('Ctrl Pts',(18.8269985365369,-1.37416556805341,115.490800315133));
#52576=CARTESIAN_POINT('Ctrl Pts',(19.3091730618201,-1.16418222178215,115.522865895736));
#52577=CARTESIAN_POINT('Ctrl Pts',(19.6826743730051,-0.790869258048996,
115.555045084909));
#52578=CARTESIAN_POINT('Ctrl Pts',(19.8592522083324,-0.386354923335411,
115.581955060021));
#52579=CARTESIAN_POINT('Ctrl Pts',(19.9047342090055,-0.039775606573619,
115.603538521507));
#52580=CARTESIAN_POINT('Ctrl Pts',(19.8900978097642,0.222324863243005,115.619754213295));
#52581=CARTESIAN_POINT('Ctrl Pts',(19.8373395713028,0.435090922581195,115.633289817848));
#52582=CARTESIAN_POINT('Ctrl Pts',(19.7718546188064,0.597339740059701,115.644132193337));
#52583=CARTESIAN_POINT('Ctrl Pts',(19.651425322384,0.830816794202225,115.660409573376));
#52584=CARTESIAN_POINT('Ctrl Pts',(19.3896969715251,1.13513142859796,115.684876307424));
#52585=CARTESIAN_POINT('Ctrl Pts',(18.9150284789188,1.38619680296976,115.717606636203));
#52586=CARTESIAN_POINT('Ctrl Pts',(18.3797054104768,1.4466716138587,115.750443142464));
#52587=CARTESIAN_POINT('Ctrl Pts',(17.988183958309,1.34188408743399,115.775149099498));
#52588=CARTESIAN_POINT('Ctrl Pts',(17.7539350453868,1.21509730703865,115.791652121032));
#52589=CARTESIAN_POINT('Ctrl Pts',(17.6061813470909,1.11641122904621,115.802662864195));
#52590=CARTESIAN_POINT('Ctrl Pts',(17.3731821120973,0.908319548202519,115.821953447962));
#52591=CARTESIAN_POINT('Ctrl Pts',(17.2162644616103,0.659137577823519,115.839908099308));
#52592=CARTESIAN_POINT('Ctrl Pts',(17.1398169389646,0.449494569945197,115.85374265585));
#52593=CARTESIAN_POINT('Ctrl Pts',(17.1197416648792,0.385640496558971,115.85789451934));
#52594=CARTESIAN_POINT('Ctrl Pts',(17.1027272724371,0.320847543293446,115.862047984451));
#52595=CARTESIAN_POINT('Ctrl Pts',(17.0887358351757,0.255330496363598,115.866202984813));
#52596=CARTESIAN_POINT('Ctrl Pts',(17.0777963741667,0.189195464046852,115.870359570435));
#52597=CARTESIAN_POINT('Ctrl Pts',(17.067418125527,0.100399771748922,115.87590376183));
#52598=CARTESIAN_POINT('Ctrl Pts',(17.0557272856128,-0.145527942481447,
115.891159038571));
#52599=CARTESIAN_POINT('Ctrl Pts',(17.1319155326297,-0.548674192364992,
115.916167747218));
#52600=CARTESIAN_POINT('Ctrl Pts',(17.4236891361341,-1.01332159343547,115.949610144654));
#52601=CARTESIAN_POINT('Ctrl Pts',(17.8662933378701,-1.34016087503944,115.983147288212));
#52602=CARTESIAN_POINT('Ctrl Pts',(18.399223693082,-1.48309771040529,116.016777928577));
#52603=CARTESIAN_POINT('Ctrl Pts',(18.9489636278778,-1.42130150179873,116.050499822527));
#52604=CARTESIAN_POINT('Ctrl Pts',(19.439526569492,-1.16221164480534,116.084311444931));
#52605=CARTESIAN_POINT('Ctrl Pts',(19.7216356020653,-0.834420794277268,
116.110677095138));
#52606=CARTESIAN_POINT('Ctrl Pts',(19.8572233100093,-0.561455048962172,
116.129541929259));
#52607=CARTESIAN_POINT('Ctrl Pts',(19.9376530730783,-0.331222395435849,
116.144645751291));
#52608=CARTESIAN_POINT('Ctrl Pts',(20.0024589418389,0.0939862014720346,
116.171111021937));
#52609=CARTESIAN_POINT('Ctrl Pts',(19.8626252653565,0.708422611339051,116.20900999971));
#52610=CARTESIAN_POINT('Ctrl Pts',(19.3606426600479,1.27757833594637,116.254631289769));
#52611=CARTESIAN_POINT('Ctrl Pts',(18.6457170687546,1.53809320293154,116.300389436894));
#52612=CARTESIAN_POINT('Ctrl Pts',(17.890910575448,1.4246417143608,116.346279427979));
#52613=CARTESIAN_POINT('Ctrl Pts',(17.3697592183846,1.03003291245044,116.385584939065));
#52614=CARTESIAN_POINT('Ctrl Pts',(17.100337406561,0.571607302391164,116.418246772046));
#52615=CARTESIAN_POINT('Ctrl Pts',(16.9582745330856,0.0258686179393441,
116.452879275666));
#52616=CARTESIAN_POINT('Ctrl Pts',(17.079642569554,-0.691275011863127,116.4962606349));
#52617=CARTESIAN_POINT('Ctrl Pts',(17.6627581645516,-1.34421776223012,116.54845478634));
#52618=CARTESIAN_POINT('Ctrl Pts',(18.5058185302644,-1.58735022301968,116.600777176171));
#52619=CARTESIAN_POINT('Ctrl Pts',(19.3508960628413,-1.34420890496649,116.65321930077));
#52620=CARTESIAN_POINT('Ctrl Pts',(19.9385417998377,-0.687144258006306,
116.705772267722));
#52621=CARTESIAN_POINT('Ctrl Pts',(20.0616184527334,0.0381325630880677,
116.74965182232));
#52622=CARTESIAN_POINT('Ctrl Pts',(19.9176287834958,0.592128040193145,116.784801682567));
#52623=CARTESIAN_POINT('Ctrl Pts',(19.6999442414976,0.962347691535422,116.81118670354));
#52624=CARTESIAN_POINT('Ctrl Pts',(19.387187078997,1.25730153941532,116.83759221283));
#52625=CARTESIAN_POINT('Ctrl Pts',(18.8779720660596,1.52166037321083,116.872826686248));
#52626=CARTESIAN_POINT('Ctrl Pts',(18.1399667081786,1.56350792410162,116.9169162291));
#52627=CARTESIAN_POINT('Ctrl Pts',(17.3622686789024,1.13377519632968,116.969889685186));
#52628=CARTESIAN_POINT('Ctrl Pts',(16.9320466679883,0.355566704353337,117.022919441898));
#52629=CARTESIAN_POINT('Ctrl Pts',(16.9818233579469,-0.533172765301191,
117.075996285446));
#52630=CARTESIAN_POINT('Ctrl Pts',(17.4972137629198,-1.25963702599659,117.129110660468));
#52631=CARTESIAN_POINT('Ctrl Pts',(18.3205410600314,-1.60074493849521,117.18225312368));
#52632=CARTESIAN_POINT('Ctrl Pts',(19.199461586771,-1.45143815071003,117.23541411388));
#52633=CARTESIAN_POINT('Ctrl Pts',(19.8643227073833,-0.857296174050731,
117.288584083064));
#52634=CARTESIAN_POINT('Ctrl Pts',(20.1111513110505,-0.000491905914397789,
117.341753458203));
#52635=CARTESIAN_POINT('Ctrl Pts',(19.8643244718875,0.856132975128993,117.394912684707));
#52636=CARTESIAN_POINT('Ctrl Pts',(19.1998096494292,1.44990225773341,117.448052198099));
#52637=CARTESIAN_POINT('Ctrl Pts',(18.3217251143232,1.599013628145,117.501162465982));
#52638=CARTESIAN_POINT('Ctrl Pts',(17.499504374338,1.25832728231969,117.554234001358));
#52639=CARTESIAN_POINT('Ctrl Pts',(16.985055982408,0.533061319756643,117.60725735614));
#52640=CARTESIAN_POINT('Ctrl Pts',(16.9353935453568,-0.353785275682392,
117.660223128507));
#52641=CARTESIAN_POINT('Ctrl Pts',(17.3646646422282,-1.13011770093016,117.713122006794));
#52642=CARTESIAN_POINT('Ctrl Pts',(18.1400392517145,-1.55845623704423,117.76594474964));
#52643=CARTESIAN_POINT('Ctrl Pts',(19.0230777257463,-1.50863468531329,117.818682215354));
#52644=CARTESIAN_POINT('Ctrl Pts',(19.7428658914057,-0.997619269505286,
117.871325327931));
#52645=CARTESIAN_POINT('Ctrl Pts',(20.0799462528815,-0.183426406491474,
117.923865215528));
#52646=CARTESIAN_POINT('Ctrl Pts',(19.9567569394742,0.538729417132324,117.967555008894));
#52647=CARTESIAN_POINT('Ctrl Pts',(19.6400599565462,1.01030681822159,118.002446570801));
#52648=CARTESIAN_POINT('Ctrl Pts',(19.2073385738753,1.37731958827904,118.03729626475));
#52649=CARTESIAN_POINT('Ctrl Pts',(18.5067297996373,1.57915592164188,118.080777892618));
#52650=CARTESIAN_POINT('Ctrl Pts',(17.6681360568722,1.33710476368857,118.132817962888));
#52651=CARTESIAN_POINT('Ctrl Pts',(17.0885466977777,0.6880330974798,118.184712313374));
#52652=CARTESIAN_POINT('Ctrl Pts',(16.9435495706207,-0.167492528644316,
118.236452721141));
#52653=CARTESIAN_POINT('Ctrl Pts',(17.2749324092385,-0.966447647923809,
118.288031455808));
#52654=CARTESIAN_POINT('Ctrl Pts',(17.9782861905575,-1.46502430150085,118.33944080786));
#52655=CARTESIAN_POINT('Ctrl Pts',(18.8361224498172,-1.51274888582587,118.390673366568));
#52656=CARTESIAN_POINT('Ctrl Pts',(19.5851780705485,-1.09829472567512,118.441721870754));
#52657=CARTESIAN_POINT('Ctrl Pts',(19.9973084426146,-0.351551880340416,
118.492579360892));
#52658=CARTESIAN_POINT('Ctrl Pts',(19.9492369017591,0.496527279998027,118.543238980189));
#52659=CARTESIAN_POINT('Ctrl Pts',(19.4591265716024,1.1865303680748,118.59369432018));
#52660=CARTESIAN_POINT('Ctrl Pts',(18.8104123489689,1.45452734640773,118.635564768299));
#52661=CARTESIAN_POINT('Ctrl Pts',(18.2668600482904,1.43813882096128,118.66895295447));
#52662=CARTESIAN_POINT('Ctrl Pts',(17.8793606825511,1.3149779455841,118.69393898397));
#52663=CARTESIAN_POINT('Ctrl Pts',(17.5418800138726,1.08918872056738,118.718869663376));
#52664=CARTESIAN_POINT('Ctrl Pts',(17.2806722359481,0.779868090767067,118.743743756155));
#52665=CARTESIAN_POINT('Ctrl Pts',(17.115688834786,0.41095174070353,118.768561126351));
#52666=CARTESIAN_POINT('Ctrl Pts',(17.059420080157,0.0118658393363464,118.793320604163));
#52667=CARTESIAN_POINT('Ctrl Pts',(17.1156776902122,-0.386417116216434,
118.818022013955));
#52668=CARTESIAN_POINT('Ctrl Pts',(17.2523308733496,-0.691438028513019,
118.838557160723));
#52669=CARTESIAN_POINT('Ctrl Pts',(17.4087191006526,-0.905517574177908,
118.854955848303));
#52670=CARTESIAN_POINT('Ctrl Pts',(17.5933085235369,-1.09500930757365,118.871334137985));
#52671=CARTESIAN_POINT('Ctrl Pts',(17.9803266474948,-1.35467533102602,118.899944149037));
#52672=CARTESIAN_POINT('Ctrl Pts',(18.6532437648212,-1.46879524415219,118.940663432495));
#52673=CARTESIAN_POINT('Ctrl Pts',(19.4066095777413,-1.15607767482664,118.989279524881));
#52674=CARTESIAN_POINT('Ctrl Pts',(19.7969063670871,-0.604727996663488,
119.029583574239));
#52675=CARTESIAN_POINT('Ctrl Pts',(19.8852025512401,-0.15555160666413,119.05768465636));
#52676=CARTESIAN_POINT('Ctrl Pts',(19.88174482432,0.103206678710061,119.073710544167));
#52677=CARTESIAN_POINT('Ctrl Pts',(19.8420242547932,0.359028078531283,119.089714694668));
#52678=CARTESIAN_POINT('Ctrl Pts',(19.7258720066209,0.662275611606032,119.109679686885));
#52679=CARTESIAN_POINT('Ctrl Pts',(19.4145468469588,1.07750284183372,119.141536856276));
#52680=CARTESIAN_POINT('Ctrl Pts',(18.8325235269669,1.39878522268015,119.181194851707));
#52681=CARTESIAN_POINT('Ctrl Pts',(18.0400340075687,1.35363547075075,119.228519889168));
#52682=CARTESIAN_POINT('Ctrl Pts',(17.3967718435735,0.89641934013867,119.275577945121));
#52683=CARTESIAN_POINT('Ctrl Pts',(17.1472193984553,0.292229951924935,119.314568595929));
#52684=CARTESIAN_POINT('Ctrl Pts',(17.1625698892113,-0.213333516171699,
119.345625653156));
#52685=CARTESIAN_POINT('Ctrl Pts',(17.2578325055986,-0.513471977461749,
119.364979574332));
#52686=CARTESIAN_POINT('Ctrl Pts',(17.3665030300232,-0.703170857591556,
119.378497592737));
#52687=CARTESIAN_POINT('Ctrl Pts',(17.4391238043473,-0.804166878514464,
119.386213631278));
#52688=CARTESIAN_POINT('Ctrl Pts',(17.5187561772849,-0.899766250215976,
119.393923967814));
#52689=CARTESIAN_POINT('Ctrl Pts',(17.630281948166,-1.00820403810343,119.403551172218));
#52690=CARTESIAN_POINT('Ctrl Pts',(17.8309717833451,-1.15490872115532,119.418932014259));
#52691=CARTESIAN_POINT('Ctrl Pts',(18.1160464864079,-1.28243128828034,119.438115227001));
#52692=CARTESIAN_POINT('Ctrl Pts',(18.4860686310391,-1.33458226019453,119.461066507994));
#52693=CARTESIAN_POINT('Ctrl Pts',(18.8549377775812,-1.28242608286313,119.483949129966));
#52694=CARTESIAN_POINT('Ctrl Pts',(19.1939409847697,-1.13065085353412,119.506762964988));
#52695=CARTESIAN_POINT('Ctrl Pts',(19.4768178449134,-0.891673212986614,
119.52950802525));
#52696=CARTESIAN_POINT('Ctrl Pts',(19.6818581712436,-0.584671279112933,
119.552184188786));
#52697=CARTESIAN_POINT('Ctrl Pts',(19.7935622110083,-0.233953471223591,
119.574791531524));
#52698=CARTESIAN_POINT('Ctrl Pts',(19.8037606611236,0.132828699787753,119.597329945963));
#52699=CARTESIAN_POINT('Ctrl Pts',(19.7275779091676,0.428031572432683,119.616054659699));
#52700=CARTESIAN_POINT('Ctrl Pts',(19.619614446759,0.644065603823603,119.630999964254));
#52701=CARTESIAN_POINT('Ctrl Pts',(19.4488281681557,0.89250425474605,119.64965300798));
#52702=CARTESIAN_POINT('Ctrl Pts',(19.1170401588768,1.16456978521157,119.675687037975));
#52703=CARTESIAN_POINT('Ctrl Pts',(18.5871553030014,1.30892105032127,119.709005045111));
#52704=CARTESIAN_POINT('Ctrl Pts',(18.0470739154042,1.22466017262848,119.742169110698));
#52705=CARTESIAN_POINT('Ctrl Pts',(17.5906153353427,0.92852820021813,119.775179782028));
#52706=CARTESIAN_POINT('Ctrl Pts',(17.2962939028983,0.473891549786357,119.80803764787));
#52707=CARTESIAN_POINT('Ctrl Pts',(17.2137278862079,-0.0588069964784256,
119.840743488334));
#52708=CARTESIAN_POINT('Ctrl Pts',(17.3552583261151,-0.576413195052804,
119.873298037803));
#52709=CARTESIAN_POINT('Ctrl Pts',(17.6378267009486,-0.920280590517876,
119.900301683486));
#52710=CARTESIAN_POINT('Ctrl Pts',(17.9322059358076,-1.10769984563428,119.921829832672));
#52711=CARTESIAN_POINT('Ctrl Pts',(18.2582726230055,-1.22986089927834,119.943308554429));
#52712=CARTESIAN_POINT('Ctrl Pts',(18.6988777360301,-1.24826140338436,119.970064276947));
#52713=CARTESIAN_POINT('Ctrl Pts',(19.1882573017696,-1.05324218253824,120.002024304111));
#52714=CARTESIAN_POINT('Ctrl Pts',(19.5536298555227,-0.677126307322699,
120.033838749918));
#52715=CARTESIAN_POINT('Ctrl Pts',(19.7327011533039,-0.186782542043285,
120.065509088722));
#52716=CARTESIAN_POINT('Ctrl Pts',(19.6960404522687,0.331577532740455,120.0970368287));
#52717=CARTESIAN_POINT('Ctrl Pts',(19.4519605062165,0.787710743631352,120.128423616381));
#52718=CARTESIAN_POINT('Ctrl Pts',(19.0446667619321,1.10296875506974,120.159671158499));
#52719=CARTESIAN_POINT('Ctrl Pts',(18.5463561410001,1.22382983664122,120.19078130098));
#52720=CARTESIAN_POINT('Ctrl Pts',(18.0442916571447,1.13105334473252,120.221755909485));
#52721=CARTESIAN_POINT('Ctrl Pts',(17.6955585720856,0.890589398969558,120.247456881368));
#52722=CARTESIAN_POINT('Ctrl Pts',(17.494206304073,0.626324017549734,120.267951925713));
#52723=CARTESIAN_POINT('Ctrl Pts',(17.3521978134265,0.326733896928664,120.288403487671));
#52724=CARTESIAN_POINT('Ctrl Pts',(17.2994574052005,-0.089976635869453,
120.313887268105));
#52725=CARTESIAN_POINT('Ctrl Pts',(17.4453910079367,-0.570256699169521,
120.344340822402));
#52726=CARTESIAN_POINT('Ctrl Pts',(17.7733937212861,-0.947489949761874,
120.374669791192));
#52727=CARTESIAN_POINT('Ctrl Pts',(18.2250498759407,-1.15701559211397,120.404876598007));
#52728=CARTESIAN_POINT('Ctrl Pts',(18.7209167059739,-1.16376250471033,120.43496378867));
#52729=CARTESIAN_POINT('Ctrl Pts',(19.1745246697594,-0.968157083714777,
120.46493395781));
#52730=CARTESIAN_POINT('Ctrl Pts',(19.5074032171353,-0.605727211221481,
120.494789798378));
#52731=CARTESIAN_POINT('Ctrl Pts',(19.6626391866769,-0.140691381829317,
120.524534069588));
#52732=CARTESIAN_POINT('Ctrl Pts',(19.6145749646053,0.345408120183416,120.554169611841));
#52733=CARTESIAN_POINT('Ctrl Pts',(19.3730279409814,0.767967837218571,120.583699337212));
#52734=CARTESIAN_POINT('Ctrl Pts',(18.981327184557,1.05401910504784,120.613126231449));
#52735=CARTESIAN_POINT('Ctrl Pts',(18.5085627461879,1.15479574234016,120.64245334912));
#52736=CARTESIAN_POINT('Ctrl Pts',(18.037426479005,1.05402306854266,120.671683811955));
#52737=CARTESIAN_POINT('Ctrl Pts',(17.6497818027982,0.770520108026078,120.700820806668));
#52738=CARTESIAN_POINT('Ctrl Pts',(17.4124738708295,0.354706256959195,120.729867584727));
#52739=CARTESIAN_POINT('Ctrl Pts',(17.3658345014046,-0.120342674613531,
120.758827458907));
#52740=CARTESIAN_POINT('Ctrl Pts',(17.5168518221837,-0.571705086255479,
120.787703800973));
#52741=CARTESIAN_POINT('Ctrl Pts',(17.8381564074402,-0.921050935566984,
120.816500038417));
#52742=CARTESIAN_POINT('Ctrl Pts',(18.2729637820143,-1.10819891035518,120.845219652361));
#52743=CARTESIAN_POINT('Ctrl Pts',(18.7450836643294,-1.10145297227955,120.873866177775));
#52744=CARTESIAN_POINT('Ctrl Pts',(19.1722351044748,-0.902949084941853,
120.902443198341));
#52745=CARTESIAN_POINT('Ctrl Pts',(19.4803468036944,-0.54811414646913,120.930954347204));
#52746=CARTESIAN_POINT('Ctrl Pts',(19.6163641816792,-0.0993634013560132,
120.959403296642));
#52747=CARTESIAN_POINT('Ctrl Pts',(19.5573567106693,0.36484925508517,120.987793769242));
#52748=CARTESIAN_POINT('Ctrl Pts',(19.3143653934618,0.763705712028081,121.016129512177));
#52749=CARTESIAN_POINT('Ctrl Pts',(18.9303516375633,1.0280578161787,121.044414340805));
#52750=CARTESIAN_POINT('Ctrl Pts',(18.4726214819807,1.1123686635717,121.072652047794));
#52751=CARTESIAN_POINT('Ctrl Pts',(18.0210682203609,1.00254924865375,121.100846563677));
#52752=CARTESIAN_POINT('Ctrl Pts',(17.6542606193921,0.718265809992657,121.129001647677));
#52753=CARTESIAN_POINT('Ctrl Pts',(17.4358298475876,0.309493931538336,121.157121462298));
#52754=CARTESIAN_POINT('Ctrl Pts',(17.4034366817011,-0.152362004672267,
121.185209478558));
#52755=CARTESIAN_POINT('Ctrl Pts',(17.5226227411507,-0.478090876422412,
121.206255356037));
#52756=CARTESIAN_POINT('Ctrl Pts',(17.6531201906185,-0.663090893144466,
121.22027789221));
#52757=CARTESIAN_POINT('Ctrl Pts',(17.7524655785764,-0.776636580209785,
121.229625106739));
#52758=CARTESIAN_POINT('Ctrl Pts',(17.9560938470234,-0.94641425946181,121.245976987179));
#52759=CARTESIAN_POINT('Ctrl Pts',(18.3135998936201,-1.08871343434314,121.269325120801));
#52760=CARTESIAN_POINT('Ctrl Pts',(18.7747781066023,-1.06924543466266,121.297327130536));
#52761=CARTESIAN_POINT('Ctrl Pts',(19.1875682929109,-0.863261922321633,
121.325317720602));
#52762=CARTESIAN_POINT('Ctrl Pts',(19.480175414768,-0.506709737445342,121.353300778039));
#52763=CARTESIAN_POINT('Ctrl Pts',(19.6016091931846,-0.0618147900173241,
121.38128041041));
#52764=CARTESIAN_POINT('Ctrl Pts',(19.5307495553282,0.393896407522541,121.409260613888));
#52765=CARTESIAN_POINT('Ctrl Pts',(19.2798982106118,0.78098259809769,121.437245445173));
#52766=CARTESIAN_POINT('Ctrl Pts',(18.8927083288752,1.03193571113476,121.465238926932));
#52767=CARTESIAN_POINT('Ctrl Pts',(18.4365809280527,1.10289372174427,121.493245092408));
#52768=CARTESIAN_POINT('Ctrl Pts',(17.9909862406699,0.981295289662669,121.521267957359));
#52769=CARTESIAN_POINT('Ctrl Pts',(17.6336525893153,0.688090158880322,121.54931152847));
#52770=CARTESIAN_POINT('Ctrl Pts',(17.4270545585554,0.274145584653852,121.577379799094));
#52771=CARTESIAN_POINT('Ctrl Pts',(17.407521715122,-0.188551808914773,121.605476744048));
#52772=CARTESIAN_POINT('Ctrl Pts',(17.578871006045,-0.619374849770778,121.633606325448));
#52773=CARTESIAN_POINT('Ctrl Pts',(17.9116705005978,-0.943060979454274,
121.661772468717));
#52774=CARTESIAN_POINT('Ctrl Pts',(18.3482760990906,-1.10282238037483,121.689979100292));
#52775=CARTESIAN_POINT('Ctrl Pts',(18.8127861354656,-1.07027500003871,121.718230068639));
#52776=CARTESIAN_POINT('Ctrl Pts',(19.2241926323308,-0.850473759884222,
121.746529289687));
#52777=CARTESIAN_POINT('Ctrl Pts',(19.5104728423211,-0.481127471064448,
121.774880465549));
#52778=CARTESIAN_POINT('Ctrl Pts',(19.6211489336822,-0.0261818239526985,
121.803287602493));
#52779=CARTESIAN_POINT('Ctrl Pts',(19.5361773084952,0.435267939246471,121.831754120211));
#52780=CARTESIAN_POINT('Ctrl Pts',(19.2695609307072,0.822620385440146,121.860284019395));
#52781=CARTESIAN_POINT('Ctrl Pts',(18.8670431140771,1.06787405410294,121.888880821572));
#52782=CARTESIAN_POINT('Ctrl Pts',(18.3983088047807,1.12748222485771,121.917548158767));
#52783=CARTESIAN_POINT('Ctrl Pts',(17.9449368652974,0.990091865801272,121.946289639226));
#52784=CARTESIAN_POINT('Ctrl Pts',(17.5862538567715,0.678671854848107,121.975108743805));
#52785=CARTESIAN_POINT('Ctrl Pts',(17.3854827140722,0.24670147648264,122.004008943349));
#52786=CARTESIAN_POINT('Ctrl Pts',(17.3786328692577,-0.230991019697471,
122.032993686558));
#52787=CARTESIAN_POINT('Ctrl Pts',(17.5680585071982,-0.67115046067875,122.062066264703));
#52788=CARTESIAN_POINT('Ctrl Pts',(17.9218464717271,-0.996572482097319,
122.091230038573));
#52789=CARTESIAN_POINT('Ctrl Pts',(18.3791686838937,-1.14960748605158,122.120488198196));
#52790=CARTESIAN_POINT('Ctrl Pts',(18.8607119999246,-1.10235313954737,122.14984391457));
#52791=CARTESIAN_POINT('Ctrl Pts',(19.2823992466147,-0.861717252928226,
122.179300327631));
#52792=CARTESIAN_POINT('Ctrl Pts',(19.5700353909992,-0.468457924978318,
122.208860408707));
#52793=CARTESIAN_POINT('Ctrl Pts',(19.67233106885,0.0097073705472888,122.238527197898));
#52794=CARTESIAN_POINT('Ctrl Pts',(19.5700316977566,0.489712410185742,122.268303502345));
#52795=CARTESIAN_POINT('Ctrl Pts',(19.2795029754614,0.887577837959271,122.298192256778));
#52796=CARTESIAN_POINT('Ctrl Pts',(18.8501763787566,1.13301634843011,122.328196028424));
#52797=CARTESIAN_POINT('Ctrl Pts',(18.3561006293489,1.18188281079065,122.35831766051));
#52798=CARTESIAN_POINT('Ctrl Pts',(17.8832822795417,1.02407533627195,122.388559619116));
#52799=CARTESIAN_POINT('Ctrl Pts',(17.5146580665992,0.685512525443912,122.418924457051));
#52800=CARTESIAN_POINT('Ctrl Pts',(17.3156519974485,0.224081959662186,122.44941458419));
#52801=CARTESIAN_POINT('Ctrl Pts',(17.3217321515332,-0.224535868550723,
122.476630331878));
#52802=CARTESIAN_POINT('Ctrl Pts',(17.4608369291701,-0.587814069483905,
122.500528323594));
#52803=CARTESIAN_POINT('Ctrl Pts',(17.7282696593147,-0.944769846820399,
122.527918057151));
#52804=CARTESIAN_POINT('Ctrl Pts',(18.232480082639,-1.22418021862519,122.562302776727));
#52805=CARTESIAN_POINT('Ctrl Pts',(18.9275391443125,-1.18570268762942,122.603805135729));
#52806=CARTESIAN_POINT('Ctrl Pts',(19.4987907286606,-0.781035799526716,
122.645552786729));
#52807=CARTESIAN_POINT('Ctrl Pts',(19.7688835459748,-0.130648543500597,
122.687549892942));
#52808=CARTESIAN_POINT('Ctrl Pts',(19.6507983536421,0.568114068619408,122.72980038736));
#52809=CARTESIAN_POINT('Ctrl Pts',(19.2553118912251,1.01114100863068,122.76522328566));
#52810=CARTESIAN_POINT('Ctrl Pts',(18.8317674110158,1.19977536711199,122.79369172896));
#52811=CARTESIAN_POINT('Ctrl Pts',(18.4994714464154,1.24719930072615,122.814315320483));
#52812=CARTESIAN_POINT('Ctrl Pts',(18.1788486649134,1.20667156059022,122.83420320996));
#52813=CARTESIAN_POINT('Ctrl Pts',(17.7925371098079,1.05582037916025,122.859729393806));
#52814=CARTESIAN_POINT('Ctrl Pts',(17.4016249448576,0.693715854025999,122.89176826119));
#52815=CARTESIAN_POINT('Ctrl Pts',(17.2307330623022,0.185953345830622,122.92398349555));
#52816=CARTESIAN_POINT('Ctrl Pts',(17.2523323040732,-0.23399781816306,122.949862141601));
#52817=CARTESIAN_POINT('Ctrl Pts',(17.3758319956166,-0.63702041854291,122.975812083321));
#52818=CARTESIAN_POINT('Ctrl Pts',(17.7132270565981,-1.06094316132434,123.008383394391));
#52819=CARTESIAN_POINT('Ctrl Pts',(18.2652129563259,-1.29379566909652,123.044409330373));
#52820=CARTESIAN_POINT('Ctrl Pts',(18.8048202871323,-1.27341194899918,123.077317844062));
#52821=CARTESIAN_POINT('Ctrl Pts',(19.2520591589225,-1.0786731726488,123.107057458581));
#52822=CARTESIAN_POINT('Ctrl Pts',(19.5986320076058,-0.732275146337212,
123.136919222601));
#52823=CARTESIAN_POINT('Ctrl Pts',(19.7955049190142,-0.281541487902919,
123.166903310585));
#52824=CARTESIAN_POINT('Ctrl Pts',(19.814175494069,0.212080051862212,123.197009803247));
#52825=CARTESIAN_POINT('Ctrl Pts',(19.6505357555705,0.680199603450974,123.22723875367));
#52826=CARTESIAN_POINT('Ctrl Pts',(19.3800198693595,0.994891712538085,123.252531518524));
#52827=CARTESIAN_POINT('Ctrl Pts',(19.1048855509728,1.17460736001555,123.272826913899));
#52828=CARTESIAN_POINT('Ctrl Pts',(18.7502795847464,1.32221520931078,123.296552374618));
#52829=CARTESIAN_POINT('Ctrl Pts',(18.2134028163266,1.34942925716205,123.328869397769));
#52830=CARTESIAN_POINT('Ctrl Pts',(17.7009999455689,1.10290673401308,123.363067775711));
#52831=CARTESIAN_POINT('Ctrl Pts',(17.3976492612122,0.775343454126338,123.390534343115));
#52832=CARTESIAN_POINT('Ctrl Pts',(17.2373156796508,0.480844927046111,123.411188117109));
#52833=CARTESIAN_POINT('Ctrl Pts',(17.1258389632255,0.0460476148377275,
123.438798023514));
#52834=CARTESIAN_POINT('Ctrl Pts',(17.190043079014,-0.468229286583892,123.469979677869));
#52835=CARTESIAN_POINT('Ctrl Pts',(17.4941741697257,-0.951758531768305,
123.504781176556));
#52836=CARTESIAN_POINT('Ctrl Pts',(17.9260851237358,-1.27106107307662,123.537531680416));
#52837=CARTESIAN_POINT('Ctrl Pts',(18.4738055254567,-1.40450128521582,123.571728513849));
#52838=CARTESIAN_POINT('Ctrl Pts',(19.0518747398078,-1.29815338903981,123.607389463288));
#52839=CARTESIAN_POINT('Ctrl Pts',(19.4975667911712,-0.991471108595277,
123.64021397565));
#52840=CARTESIAN_POINT('Ctrl Pts',(19.718108765147,-0.668458656443225,123.664171779265));
#52841=CARTESIAN_POINT('Ctrl Pts',(19.840684276858,-0.369704589488725,123.684176966688));
#52842=CARTESIAN_POINT('Ctrl Pts',(19.9012468618966,-0.0656783463889097,
123.703216913146));
#52843=CARTESIAN_POINT('Ctrl Pts',(19.8683061355372,0.325537213186654,123.727331521864));
#52844=CARTESIAN_POINT('Ctrl Pts',(19.7280021633901,0.693317586446537,123.751509567709));
#52845=CARTESIAN_POINT('Ctrl Pts',(19.4907339764757,1.00870957723937,123.775750778072));
#52846=CARTESIAN_POINT('Ctrl Pts',(19.1746344843562,1.24667974067477,123.800054570196));
#52847=CARTESIAN_POINT('Ctrl Pts',(18.8349045453036,1.37646300010242,123.822389896322));
#52848=CARTESIAN_POINT('Ctrl Pts',(18.5073833848405,1.41556608351708,123.842739728062));
#52849=CARTESIAN_POINT('Ctrl Pts',(18.1123610183889,1.37979837018668,123.867205371628));
#52850=CARTESIAN_POINT('Ctrl Pts',(17.6480520706786,1.18013603372677,123.89787276461));
#52851=CARTESIAN_POINT('Ctrl Pts',(17.2358803945236,0.732012860791261,123.934808434271));
#52852=CARTESIAN_POINT('Ctrl Pts',(17.0419794776495,0.152653694038211,123.971876745333));
#52853=CARTESIAN_POINT('Ctrl Pts',(17.10185151608,-0.45756914112672,124.009075627682));
#52854=CARTESIAN_POINT('Ctrl Pts',(17.4067903543957,-0.991921667797129,
124.046402830605));
#52855=CARTESIAN_POINT('Ctrl Pts',(17.9050692573643,-1.35635713407927,124.08385606453));
#52856=CARTESIAN_POINT('Ctrl Pts',(18.5107335847068,-1.48590165559992,124.121432928518));
#52857=CARTESIAN_POINT('Ctrl Pts',(19.1184385180564,-1.3563507502972,124.159130952342));
#52858=CARTESIAN_POINT('Ctrl Pts',(19.6218022289785,-0.98872576919303,124.196947576568));
#52859=CARTESIAN_POINT('Ctrl Pts',(19.9320540444447,-0.445907038184834,
124.234880164305));
#52860=CARTESIAN_POINT('Ctrl Pts',(19.9937135700085,0.178148153659393,124.272925997681));
#52861=CARTESIAN_POINT('Ctrl Pts',(19.7945218608488,0.774684491212139,124.311082283028));
#52862=CARTESIAN_POINT('Ctrl Pts',(19.3678473665426,1.23913646259581,124.349346152036));
#52863=CARTESIAN_POINT('Ctrl Pts',(18.7870971810712,1.48948517765483,124.387714664201));
#52864=CARTESIAN_POINT('Ctrl Pts',(18.1530697283671,1.48076648367652,124.426184806719));
#52865=CARTESIAN_POINT('Ctrl Pts',(17.5764302450274,1.21315420572873,124.464753497712));
#52866=CARTESIAN_POINT('Ctrl Pts',(17.1583610032014,0.73216643659731,124.503417588286));
#52867=CARTESIAN_POINT('Ctrl Pts',(16.9727754031592,0.120915171124057,124.542173865763));
#52868=CARTESIAN_POINT('Ctrl Pts',(17.053228230474,-0.514279241981028,124.581019055523));
#52869=CARTESIAN_POINT('Ctrl Pts',(17.3868443511107,-1.06241526162645,124.619949821452));
#52870=CARTESIAN_POINT('Ctrl Pts',(17.9163655702989,-1.42724443394371,124.658962768982));
#52871=CARTESIAN_POINT('Ctrl Pts',(18.5499933474172,-1.54420384030286,124.698054447786));
#52872=CARTESIAN_POINT('Ctrl Pts',(19.177333010067,-1.39186200173388,124.737221354945));
#52873=CARTESIAN_POINT('Ctrl Pts',(19.6886650872882,-0.995845166220365,
124.776459937328));
#52874=CARTESIAN_POINT('Ctrl Pts',(19.9941729942927,-0.424524481016298,
124.815766591911));
#52875=CARTESIAN_POINT('Ctrl Pts',(20.0397508728227,0.222810121504123,124.855137669041));
#52876=CARTESIAN_POINT('Ctrl Pts',(19.816603606709,0.833240192938617,124.894569475321));
#52877=CARTESIAN_POINT('Ctrl Pts',(19.3629322894934,1.29995631129024,124.934058276943));
#52878=CARTESIAN_POINT('Ctrl Pts',(18.7573836344576,1.5409857282793,124.973600302423));
#52879=CARTESIAN_POINT('Ctrl Pts',(18.1053883878064,1.51361956558236,125.013191742918));
#52880=CARTESIAN_POINT('Ctrl Pts',(17.5207664641707,1.22199509521115,125.05282875548));
#52881=CARTESIAN_POINT('Ctrl Pts',(17.1058149097213,0.716484110643661,125.092507466257));
#52882=CARTESIAN_POINT('Ctrl Pts',(16.9333696386985,0.0849747734438613,
125.132223973764));
#52883=CARTESIAN_POINT('Ctrl Pts',(17.0339933882744,-0.562441260921414,
125.171974352057));
#52884=CARTESIAN_POINT('Ctrl Pts',(17.390548421764,-1.11270270209401,125.211754651068));
#52885=CARTESIAN_POINT('Ctrl Pts',(17.9411197173863,-1.46956608382521,125.251560899613));
#52886=CARTESIAN_POINT('Ctrl Pts',(18.5897895263485,-1.570476072409,125.291389109069));
#52887=CARTESIAN_POINT('Ctrl Pts',(19.2233842915933,-1.39755490178516,125.331235276345));
#52888=CARTESIAN_POINT('Ctrl Pts',(19.7312635698777,-0.980776005995196,
125.371095387577));
#52889=CARTESIAN_POINT('Ctrl Pts',(20.0246830575117,-0.392757399099882,
125.410965418396));
#52890=CARTESIAN_POINT('Ctrl Pts',(20.0523356967461,0.263918904922262,125.45084133669));
#52891=CARTESIAN_POINT('Ctrl Pts',(19.8093430859602,0.874642369917206,125.490719106622));
#52892=CARTESIAN_POINT('Ctrl Pts',(19.338117939541,1.33282146051242,125.530594691345));
#52893=CARTESIAN_POINT('Ctrl Pts',(18.7209447529552,1.55852867925055,125.570464057095));
#52894=CARTESIAN_POINT('Ctrl Pts',(18.0655795919603,1.51247445386863,125.610323173319));
#52895=CARTESIAN_POINT('Ctrl Pts',(17.4863946151243,1.20286152519264,125.650168015395));
#52896=CARTESIAN_POINT('Ctrl Pts',(17.08437402484,0.68392126836871,125.689994568545));
#52897=CARTESIAN_POINT('Ctrl Pts',(16.929468039317,0.0463936644794652,125.729798830645));
#52898=CARTESIAN_POINT('Ctrl Pts',(17.0483951994113,-0.598374148289317,
125.769576816299));
#52899=CARTESIAN_POINT('Ctrl Pts',(17.4200245578257,-1.13791782047621,125.809324557098));
#52900=CARTESIAN_POINT('Ctrl Pts',(17.9791373208165,-1.47831538930677,125.849038104005));
#52901=CARTESIAN_POINT('Ctrl Pts',(18.6278970714101,-1.56057234280656,125.888713531393));
#52902=CARTESIAN_POINT('Ctrl Pts',(19.2530067739201,-1.37086750720055,125.928346939608));
#52903=CARTESIAN_POINT('Ctrl Pts',(19.7455372169818,-0.942876630111474,
125.967934459145));
#52904=CARTESIAN_POINT('Ctrl Pts',(20.0199490743694,-0.351783080761525,
126.007472250877));
#52905=CARTESIAN_POINT('Ctrl Pts',(20.0289798900698,0.298956955377318,126.046956508333));
#52906=CARTESIAN_POINT('Ctrl Pts',(19.7717997014967,0.895760095633046,126.086383461411));
#52907=CARTESIAN_POINT('Ctrl Pts',(19.2940254107556,1.33478268233592,126.125749379074));
#52908=CARTESIAN_POINT('Ctrl Pts',(18.6796145554874,1.54002675564106,126.165050573152));
#52909=CARTESIAN_POINT('Ctrl Pts',(18.0360819363224,1.47652170954235,126.204283398858));
#52910=CARTESIAN_POINT('Ctrl Pts',(17.4756475553532,1.15629106504151,126.243444256678));
#52911=CARTESIAN_POINT('Ctrl Pts',(17.0956282178994,0.636085037276605,126.282529595954));
#52912=CARTESIAN_POINT('Ctrl Pts',(16.9615059717559,0.00730541265974819,
126.321535917403));
#52913=CARTESIAN_POINT('Ctrl Pts',(17.0956248257272,-0.62008509447962,126.360459776655));
#52914=CARTESIAN_POINT('Ctrl Pts',(17.4734700822054,-1.13683065414485,126.399297784896));
#52915=CARTESIAN_POINT('Ctrl Pts',(18.0281490556148,-1.45344460991142,126.43804661051));
#52916=CARTESIAN_POINT('Ctrl Pts',(18.6622538987967,-1.51573411677912,126.476702982318));
#52917=CARTESIAN_POINT('Ctrl Pts',(19.2649987922204,-1.31408906543418,126.515263692086));
#52918=CARTESIAN_POINT('Ctrl Pts',(19.731610851688,-0.884941277427619,126.553725597545));
#52919=CARTESIAN_POINT('Ctrl Pts',(19.9815743866459,-0.304177503036399,
126.592085623336));
#52920=CARTESIAN_POINT('Ctrl Pts',(19.9725463963688,0.326301385032026,126.630340762356));
#52921=CARTESIAN_POINT('Ctrl Pts',(19.7075342584873,0.896490569366356,126.668488078281));
#52922=CARTESIAN_POINT('Ctrl Pts',(19.2341192578344,1.30750680377586,126.70652470863));
#52923=CARTESIAN_POINT('Ctrl Pts',(18.635904943503,1.48876449058148,126.744447866081));
#52924=CARTESIAN_POINT('Ctrl Pts',(18.0177319941314,1.41011257811453,126.782254841743));
#52925=CARTESIAN_POINT('Ctrl Pts',(17.4872732878289,1.08684624833835,126.819943002246));
#52926=CARTESIAN_POINT('Ctrl Pts',(17.1362552397195,0.576755853808402,126.857509799078));
#52927=CARTESIAN_POINT('Ctrl Pts',(17.0245670874354,-0.0302098809080251,
126.894952757996));
#52928=CARTESIAN_POINT('Ctrl Pts',(17.1700489322066,-0.62783585744949,126.932269505093));
#52929=CARTESIAN_POINT('Ctrl Pts',(17.5456363009555,-1.11223706751881,126.969457722877));
#52930=CARTESIAN_POINT('Ctrl Pts',(18.0844346743395,-1.39997160299426,127.006515235409));
#52931=CARTESIAN_POINT('Ctrl Pts',(18.6915498483127,-1.44237197701727,127.043439851825));
#52932=CARTESIAN_POINT('Ctrl Pts',(19.2610012684699,-1.2338864451594,127.080229666573));
#52933=CARTESIAN_POINT('Ctrl Pts',(19.6217471892279,-0.882743718249303,
127.110773685143));
#52934=CARTESIAN_POINT('Ctrl Pts',(19.805122901504,-0.532909080357985,127.135139757539));
#52935=CARTESIAN_POINT('Ctrl Pts',(19.9119297871484,-0.153404834080003,
127.159459066494));
#52936=CARTESIAN_POINT('Ctrl Pts',(19.8907835817646,0.345745192049258,127.189770694683));
#52937=CARTESIAN_POINT('Ctrl Pts',(19.6238862093633,0.880005756149412,127.226002377005));
#52938=CARTESIAN_POINT('Ctrl Pts',(19.1639432332974,1.25716124729007,127.262090500425));
#52939=CARTESIAN_POINT('Ctrl Pts',(18.5923414539904,1.4129249048356,127.298033459251));
#52940=CARTESIAN_POINT('Ctrl Pts',(18.009376013041,1.32200688726968,127.333829961582));
#52941=CARTESIAN_POINT('Ctrl Pts',(17.5164251968782,1.00223104074899,127.369478700124));
#52942=CARTESIAN_POINT('Ctrl Pts',(17.1984201622755,0.511061484236086,127.404978528688));
#52943=CARTESIAN_POINT('Ctrl Pts',(17.1091447607243,-0.0647150657709647,
127.440328369783));
#52944=CARTESIAN_POINT('Ctrl Pts',(17.2621761209424,-0.624337498948366,
127.47552726517));
#52945=CARTESIAN_POINT('Ctrl Pts',(17.6288480874875,-1.07071164630888,127.510574350276));
#52946=CARTESIAN_POINT('Ctrl Pts',(18.1436098481768,-1.32726550817446,127.545468867205));
#52947=CARTESIAN_POINT('Ctrl Pts',(18.7157402346546,-1.35108485996325,127.580210160365));
#52948=CARTESIAN_POINT('Ctrl Pts',(19.245344894428,-1.14007961976173,127.614797677075));
#52949=CARTESIAN_POINT('Ctrl Pts',(19.640802728471,-0.732985556833016,127.649230973288));
#52950=CARTESIAN_POINT('Ctrl Pts',(19.8346190767915,-0.202266924232661,
127.68350970104));
#52951=CARTESIAN_POINT('Ctrl Pts',(19.794941200486,0.358782068939732,127.717633632851));
#52952=CARTESIAN_POINT('Ctrl Pts',(19.53076983591,0.852439588636981,127.751602617564));
#52953=CARTESIAN_POINT('Ctrl Pts',(19.090026891229,1.19357867870462,127.785416661368));
#52954=CARTESIAN_POINT('Ctrl Pts',(18.5508679670964,1.32434237931937,127.819075778772));
#52955=CARTESIAN_POINT('Ctrl Pts',(18.0078302825239,1.22394906443107,127.852580278532));
#52956=CARTESIAN_POINT('Ctrl Pts',(17.5552573816975,0.911952688854262,127.885930186338));
#52957=CARTESIAN_POINT('Ctrl Pts',(17.2709072300368,0.444489100297998,127.919126443317));
#52958=CARTESIAN_POINT('Ctrl Pts',(17.2026017157444,-0.0958390632178888,
127.95216844486));
#52959=CARTESIAN_POINT('Ctrl Pts',(17.3602499056931,-0.614522317041156,
127.98505884808));
#52960=CARTESIAN_POINT('Ctrl Pts',(17.7142513339655,-1.02169725457206,128.017794748452));
#52961=CARTESIAN_POINT('Ctrl Pts',(18.2016487037711,-1.24768921999965,128.050383328832));
#52962=CARTESIAN_POINT('Ctrl Pts',(18.7359726277051,-1.25494106694358,128.082813363425));
#52963=CARTESIAN_POINT('Ctrl Pts',(19.2248728288001,-1.04408787605343,128.115109897118));
#52964=CARTESIAN_POINT('Ctrl Pts',(19.5831890659344,-0.65421290817496,128.147230907527));
#52965=CARTESIAN_POINT('Ctrl Pts',(19.7492083587371,-0.153536892969666,
128.179236143029));
#52966=CARTESIAN_POINT('Ctrl Pts',(19.7078812619029,0.281365767131694,128.205782412348));
#52967=CARTESIAN_POINT('Ctrl Pts',(19.5690632182825,0.594917565556771,128.226900693016));
#52968=CARTESIAN_POINT('Ctrl Pts',(19.4172180661828,0.803935885721005,128.242751399009));
#52969=CARTESIAN_POINT('Ctrl Pts',(19.2267655611754,0.976197794016201,128.258576146578));
#52970=CARTESIAN_POINT('Ctrl Pts',(19.0095330421784,1.10340832807125,128.274317652345));
#52971=CARTESIAN_POINT('Ctrl Pts',(18.7723693852942,1.18134487520901,128.289992329285));
#52972=CARTESIAN_POINT('Ctrl Pts',(18.6008172746989,1.19991945929139,128.300512808918));
#52973=CARTESIAN_POINT('Ctrl Pts',(18.5113472588518,1.200672491065,128.305809153521));
#52974=CARTESIAN_POINT('Ctrl Pts',(18.5130339424071,1.20056362969837,113.106041784737));
#52975=CARTESIAN_POINT('Ctrl Pts',(18.3796380772671,1.19944089238864,113.113938401934));
#52976=CARTESIAN_POINT('Ctrl Pts',(18.212995110346,1.1725142972848,113.124339511499));
#52977=CARTESIAN_POINT('Ctrl Pts',(17.9826591490378,1.08305259160243,113.139896234827));
#52978=CARTESIAN_POINT('Ctrl Pts',(17.803524665933,0.978054082781836,113.152884087551));
#52979=CARTESIAN_POINT('Ctrl Pts',(17.6157274597086,0.808171438104614,113.168486383471));
#52980=CARTESIAN_POINT('Ctrl Pts',(17.4669698936293,0.603184371142723,113.184027320395));
#52981=CARTESIAN_POINT('Ctrl Pts',(17.3317154043875,0.297605532561133,113.204606209043));
#52982=CARTESIAN_POINT('Ctrl Pts',(17.2920324724794,-0.124072418916653,
113.230343010212));
#52983=CARTESIAN_POINT('Ctrl Pts',(17.4520170046263,-0.605055189514055,
113.261099028093));
#52984=CARTESIAN_POINT('Ctrl Pts',(17.7934912025519,-0.975855665840217,
113.291676037855));
#52985=CARTESIAN_POINT('Ctrl Pts',(18.2552189298271,-1.17453711052494,113.322168039442));
#52986=CARTESIAN_POINT('Ctrl Pts',(18.7551481137232,-1.16725239972225,113.35250943295));
#52987=CARTESIAN_POINT('Ctrl Pts',(19.2070991942618,-0.957223190961011,
113.382741513919));
#52988=CARTESIAN_POINT('Ctrl Pts',(19.5322973485556,-0.582468238754353,
113.412845200661));
#52989=CARTESIAN_POINT('Ctrl Pts',(19.67562911591,-0.109392115546574,113.4428364914));
#52990=CARTESIAN_POINT('Ctrl Pts',(19.6134333463132,0.379063695104254,113.472709212202));
#52991=CARTESIAN_POINT('Ctrl Pts',(19.3581335051897,0.797942154392361,113.502471576948));
#52992=CARTESIAN_POINT('Ctrl Pts',(18.9554988299117,1.07499280853608,113.532123455326));
#52993=CARTESIAN_POINT('Ctrl Pts',(18.4765513487883,1.16311071322141,113.561669163361));
#52994=CARTESIAN_POINT('Ctrl Pts',(18.0050418257343,1.04832938392337,113.591111034677));
#52995=CARTESIAN_POINT('Ctrl Pts',(17.6228462935274,0.751992898776048,113.620452417211));
#52996=CARTESIAN_POINT('Ctrl Pts',(17.3957735356024,0.326816053916071,113.649696269244));
#52997=CARTESIAN_POINT('Ctrl Pts',(17.3622692515483,-0.152473939923612,
113.678845838443));
#52998=CARTESIAN_POINT('Ctrl Pts',(17.5269312773492,-0.602238859891372,
113.707904360153));
#52999=CARTESIAN_POINT('Ctrl Pts',(17.8599195062755,-0.944488824492963,
113.736875095012));
#53000=CARTESIAN_POINT('Ctrl Pts',(18.3023688496958,-1.12037212295033,113.765761510337));
#53001=CARTESIAN_POINT('Ctrl Pts',(18.7767195011618,-1.10026390590182,113.79456682245));
#53002=CARTESIAN_POINT('Ctrl Pts',(19.20036232763,-0.888732269322817,113.823294822786));
#53003=CARTESIAN_POINT('Ctrl Pts',(19.4998782438405,-0.523565915353651,
113.851948718461));
#53004=CARTESIAN_POINT('Ctrl Pts',(19.6238287528582,-0.069042122852276,
113.880532304547));
#53005=CARTESIAN_POINT('Ctrl Pts',(19.5514932889337,0.395397386636452,113.909049120675));
#53006=CARTESIAN_POINT('Ctrl Pts',(19.2963413863882,0.788895724742068,113.937502807462));
#53007=CARTESIAN_POINT('Ctrl Pts',(18.9035408070196,1.04336396475033,113.965897201427));
#53008=CARTESIAN_POINT('Ctrl Pts',(18.5189033647821,1.10305718516976,113.989512715973));
#53009=CARTESIAN_POINT('Ctrl Pts',(18.2170935930471,1.05362629581146,114.008379364579));
#53010=CARTESIAN_POINT('Ctrl Pts',(17.9322721627584,0.942922183815482,114.027229373729));
#53011=CARTESIAN_POINT('Ctrl Pts',(17.6324657495509,0.696846674343144,114.050761688215));
#53012=CARTESIAN_POINT('Ctrl Pts',(17.425055503591,0.280959502915125,114.078956524793));
#53013=CARTESIAN_POINT('Ctrl Pts',(17.4055967944488,-0.18267754383417,114.10711104627));
#53014=CARTESIAN_POINT('Ctrl Pts',(17.576990714563,-0.613287408704696,114.135229246085));
#53015=CARTESIAN_POINT('Ctrl Pts',(17.9089222268986,-0.935960644535223,
114.163315083866));
#53016=CARTESIAN_POINT('Ctrl Pts',(18.3432587594393,-1.09476592174151,114.191372484275));
#53017=CARTESIAN_POINT('Ctrl Pts',(18.8041739436501,-1.0623506219891,114.219405440553));
#53018=CARTESIAN_POINT('Ctrl Pts',(19.2113568643764,-0.844671996115093,
114.247417994911));
#53019=CARTESIAN_POINT('Ctrl Pts',(19.4939565663678,-0.479881778207605,
114.275414073228));
#53020=CARTESIAN_POINT('Ctrl Pts',(19.602870578309,-0.0316875262133413,
114.303397813562));
#53021=CARTESIAN_POINT('Ctrl Pts',(19.5192551399362,0.421780427746786,114.331373149327));
#53022=CARTESIAN_POINT('Ctrl Pts',(19.2577675592491,0.801476804257206,114.359344171195));
#53023=CARTESIAN_POINT('Ctrl Pts',(18.8640009332427,1.04126649915409,114.38731491532));
#53024=CARTESIAN_POINT('Ctrl Pts',(18.4065801432745,1.09932167624799,114.415289415434));
#53025=CARTESIAN_POINT('Ctrl Pts',(17.9652147903995,0.96545323156242,114.443271718198));
#53026=CARTESIAN_POINT('Ctrl Pts',(17.6168702254584,0.662865250839041,114.471265856675));
#53027=CARTESIAN_POINT('Ctrl Pts',(17.4223821071987,0.244151515100728,114.499275850459));
#53028=CARTESIAN_POINT('Ctrl Pts',(17.4158632785575,-0.217801781149448,
114.527305731795));
#53029=CARTESIAN_POINT('Ctrl Pts',(17.5987504131071,-0.642504769055747,
114.555359471907));
#53030=CARTESIAN_POINT('Ctrl Pts',(17.9394763579509,-0.955758872656263,
114.583441117837));
#53031=CARTESIAN_POINT('Ctrl Pts',(18.3789494100587,-1.10274388324017,114.611554520772));
#53032=CARTESIAN_POINT('Ctrl Pts',(18.7637182180745,-1.06484365534075,114.635012295721));
#53033=CARTESIAN_POINT('Ctrl Pts',(19.0424508871426,-0.942156957769831,
114.653798255564));
#53034=CARTESIAN_POINT('Ctrl Pts',(19.2899308634949,-0.764306884233674,
114.672598064115));
#53035=CARTESIAN_POINT('Ctrl Pts',(19.518838095101,-0.45130503992922,114.696125280008));
#53036=CARTESIAN_POINT('Ctrl Pts',(19.6162389073555,0.00455291390653928,
114.724405194968));
#53037=CARTESIAN_POINT('Ctrl Pts',(19.5188245336469,0.461234783976204,114.752736506486));
#53038=CARTESIAN_POINT('Ctrl Pts',(19.2428261053621,0.839051333697012,114.781122846759));
#53039=CARTESIAN_POINT('Ctrl Pts',(18.8357513946072,1.07166142270989,114.809568076315));
#53040=CARTESIAN_POINT('Ctrl Pts',(18.3681476504267,1.11783506684874,114.838075840133));
#53041=CARTESIAN_POINT('Ctrl Pts',(17.9214186539348,0.968636637637708,114.866649900509));
#53042=CARTESIAN_POINT('Ctrl Pts',(17.5737644205555,0.649236686622199,114.89529376417));
#53043=CARTESIAN_POINT('Ctrl Pts',(17.3863524615981,0.214541218418958,114.924011236812));
#53044=CARTESIAN_POINT('Ctrl Pts',(17.3922208704093,-0.207242974567453,
114.94960607363));
#53045=CARTESIAN_POINT('Ctrl Pts',(17.5227598690108,-0.548669402825176,
114.972054178389));
#53046=CARTESIAN_POINT('Ctrl Pts',(17.6641415820603,-0.736782609523537,
114.986512013638));
#53047=CARTESIAN_POINT('Ctrl Pts',(17.7781139017909,-0.842900640788488,
114.996163146039));
#53048=CARTESIAN_POINT('Ctrl Pts',(17.8386189394227,-0.89190163183184,115.000990777876));
#53049=CARTESIAN_POINT('Ctrl Pts',(17.9025047204443,-0.936525093453351,
115.005820975394));
#53050=CARTESIAN_POINT('Ctrl Pts',(18.0361866047991,-1.01671821007154,115.01548556243));
#53051=CARTESIAN_POINT('Ctrl Pts',(18.2569977876937,-1.10101938230418,115.030001946653));
#53052=CARTESIAN_POINT('Ctrl Pts',(18.5715829573991,-1.12761634912618,115.049395535593));
#53053=CARTESIAN_POINT('Ctrl Pts',(18.8819962126928,-1.06591766988281,115.068830862058));
#53054=CARTESIAN_POINT('Ctrl Pts',(19.1636267310059,-0.920442194840922,
115.088307050796));
#53055=CARTESIAN_POINT('Ctrl Pts',(19.3947687720096,-0.70212716075079,115.10782662024));
#53056=CARTESIAN_POINT('Ctrl Pts',(19.5563007110438,-0.427877912966269,
115.12738920833));
#53057=CARTESIAN_POINT('Ctrl Pts',(19.6635151319163,-0.0156350059498499,
115.153532473423));
#53058=CARTESIAN_POINT('Ctrl Pts',(19.5902298913756,0.417659782748033,115.179766516309));
#53059=CARTESIAN_POINT('Ctrl Pts',(19.3810030950217,0.729410953616704,115.202803646746));
#53060=CARTESIAN_POINT('Ctrl Pts',(19.2284838333689,0.878004295306615,115.215992109533));
#53061=CARTESIAN_POINT('Ctrl Pts',(19.0560409141327,1.00394927534599,115.229196429705));
#53062=CARTESIAN_POINT('Ctrl Pts',(18.8841989149175,1.08097496755606,115.240771440897));
#53063=CARTESIAN_POINT('Ctrl Pts',(18.7286133688239,1.1198781075186,115.250708898067));
#53064=CARTESIAN_POINT('Ctrl Pts',(18.6496731094318,1.13387301836795,115.255680590934));
#53065=CARTESIAN_POINT('Ctrl Pts',(18.5831584169845,1.14091923213438,115.259826351878));
#53066=CARTESIAN_POINT('Ctrl Pts',(18.529723859708,1.14368192373088,115.263144386349));
#53067=CARTESIAN_POINT('Ctrl Pts',(18.3127780164777,1.14782594742841,115.276605547771));
#53068=CARTESIAN_POINT('Ctrl Pts',(17.9179435637465,1.04727289839551,115.301097431437));
#53069=CARTESIAN_POINT('Ctrl Pts',(17.5797257591974,0.733975186272521,115.328828941497));
#53070=CARTESIAN_POINT('Ctrl Pts',(17.4287664162094,0.450044946400393,115.348699385795));
#53071=CARTESIAN_POINT('Ctrl Pts',(17.377297606354,0.297583470120713,115.358650468053));
#53072=CARTESIAN_POINT('Ctrl Pts',(17.3519609865365,0.171470130867239,115.366620991551));
#53073=CARTESIAN_POINT('Ctrl Pts',(17.3216820304358,-0.0841604199737449,
115.382574280005));
#53074=CARTESIAN_POINT('Ctrl Pts',(17.3965706674047,-0.509890259835511,
115.408571625553));
#53075=CARTESIAN_POINT('Ctrl Pts',(17.7713689197723,-0.980625185002351,
115.444744657348));
#53076=CARTESIAN_POINT('Ctrl Pts',(18.2819379865731,-1.19600603977953,115.478069008485));
#53077=CARTESIAN_POINT('Ctrl Pts',(18.7809183594824,-1.17713157755211,115.508498307924));
#53078=CARTESIAN_POINT('Ctrl Pts',(19.1943175486507,-0.99711316860877,115.535989892722));
#53079=CARTESIAN_POINT('Ctrl Pts',(19.5146598255097,-0.676954515020953,
115.563588212045));
#53080=CARTESIAN_POINT('Ctrl Pts',(19.6661763275141,-0.32989171948242,115.586676645489));
#53081=CARTESIAN_POINT('Ctrl Pts',(19.7052193472369,-0.0324134677453485,
115.605202352555));
#53082=CARTESIAN_POINT('Ctrl Pts',(19.692655682188,0.192603294558637,115.619123708899));
#53083=CARTESIAN_POINT('Ctrl Pts',(19.6473498976196,0.375330813104559,115.630748323528));
#53084=CARTESIAN_POINT('Ctrl Pts',(19.5910991581474,0.514700455878096,115.640061743476));
#53085=CARTESIAN_POINT('Ctrl Pts',(19.4876393156613,0.715280090270079,115.654045643533));
#53086=CARTESIAN_POINT('Ctrl Pts',(19.2627069666146,0.976847606906025,115.675074306831));
#53087=CARTESIAN_POINT('Ctrl Pts',(18.8544665534226,1.19281133282252,115.703225108284));
#53088=CARTESIAN_POINT('Ctrl Pts',(18.393677139478,1.24490620452606,115.731490065512));
#53089=CARTESIAN_POINT('Ctrl Pts',(18.056361634715,1.15465435594138,115.752775030142));
#53090=CARTESIAN_POINT('Ctrl Pts',(17.8544284561031,1.04536165171525,115.767001240127));
#53091=CARTESIAN_POINT('Ctrl Pts',(17.7270316965588,0.960272597146169,115.776494950284));
#53092=CARTESIAN_POINT('Ctrl Pts',(17.5260449274305,0.780780317627104,115.793134808535));
#53093=CARTESIAN_POINT('Ctrl Pts',(17.3905754983703,0.565699995287968,115.808633253397));
#53094=CARTESIAN_POINT('Ctrl Pts',(17.3245418584892,0.384620256252072,115.820582816104));
#53095=CARTESIAN_POINT('Ctrl Pts',(17.3071994994432,0.329457947086177,115.824169558128));
#53096=CARTESIAN_POINT('Ctrl Pts',(17.2924988163125,0.273477103726421,115.82775812202));
#53097=CARTESIAN_POINT('Ctrl Pts',(17.2804085467132,0.216862498090847,115.831348541136));
#53098=CARTESIAN_POINT('Ctrl Pts',(17.2709542538249,0.159706819127325,115.834940788347));
#53099=CARTESIAN_POINT('Ctrl Pts',(17.2619835886696,0.0829558301171504,
115.839732913633));
#53100=CARTESIAN_POINT('Ctrl Pts',(17.2518755906627,-0.129650604723723,
115.852921292731));
#53101=CARTESIAN_POINT('Ctrl Pts',(17.3177516317266,-0.478447503488098,
115.874558104341));
#53102=CARTESIAN_POINT('Ctrl Pts',(17.5704423404208,-0.880957856936553,
115.903526095127));
#53103=CARTESIAN_POINT('Ctrl Pts',(17.9542909508241,-1.16448384868491,115.932614015954));
#53104=CARTESIAN_POINT('Ctrl Pts',(18.417126376734,-1.28868540595138,115.961822241747));
#53105=CARTESIAN_POINT('Ctrl Pts',(18.8952608905801,-1.23500217847673,115.991151380529));
#53106=CARTESIAN_POINT('Ctrl Pts',(19.3225816532175,-1.00939401338301,116.020601817174));
#53107=CARTESIAN_POINT('Ctrl Pts',(19.5687260020783,-0.723472536993288,
116.043602420908));
#53108=CARTESIAN_POINT('Ctrl Pts',(19.6871366689245,-0.485101521697199,
116.060076548169));
#53109=CARTESIAN_POINT('Ctrl Pts',(19.7574170551575,-0.283927256490408,
116.073274006638));
#53110=CARTESIAN_POINT('Ctrl Pts',(19.8141138999387,0.0878915372728727,
116.096417002363));
#53111=CARTESIAN_POINT('Ctrl Pts',(19.6917792758234,0.626135643997373,116.129614388622));
#53112=CARTESIAN_POINT('Ctrl Pts',(19.2511975416191,1.12597766448505,116.169669102103));
#53113=CARTESIAN_POINT('Ctrl Pts',(18.622047619994,1.35545557509057,116.209941813808));
#53114=CARTESIAN_POINT('Ctrl Pts',(17.9560191179098,1.25556816985742,116.250432479901));
#53115=CARTESIAN_POINT('Ctrl Pts',(17.4948646415439,0.906628969258929,116.285204179477));
#53116=CARTESIAN_POINT('Ctrl Pts',(17.2559669240318,0.500241385841883,116.314159466878));
#53117=CARTESIAN_POINT('Ctrl Pts',(17.1297804940034,0.015714509245307,116.344909451306));
#53118=CARTESIAN_POINT('Ctrl Pts',(17.237512260039,-0.622576246018601,116.383518153498));
#53119=CARTESIAN_POINT('Ctrl Pts',(17.7578889155714,-1.2058175514389,116.430121193854));
#53120=CARTESIAN_POINT('Ctrl Pts',(18.5130575993667,-1.42399276281197,116.47699518141));
#53121=CARTESIAN_POINT('Ctrl Pts',(19.2728466936298,-1.20579250691246,116.524138179076));
#53122=CARTESIAN_POINT('Ctrl Pts',(19.8032798723121,-0.613305417176101,
116.571547805714));
#53123=CARTESIAN_POINT('Ctrl Pts',(19.915047421943,0.0433029384755907,116.611275982938));
#53124=CARTESIAN_POINT('Ctrl Pts',(19.7843821034173,0.54631812459105,116.643188946666));
#53125=CARTESIAN_POINT('Ctrl Pts',(19.5864236858098,0.883085765125937,116.667188711933));
#53126=CARTESIAN_POINT('Ctrl Pts',(19.3014292475285,1.15192941594928,116.691252738917));
#53127=CARTESIAN_POINT('Ctrl Pts',(18.8365401016989,1.3933575076252,116.723423700013));
#53128=CARTESIAN_POINT('Ctrl Pts',(18.160779938749,1.43204211152419,116.763796184507));
#53129=CARTESIAN_POINT('Ctrl Pts',(17.4456352832677,1.0373977222983,116.812493703962));
#53130=CARTESIAN_POINT('Ctrl Pts',(17.0481573163662,0.319374993023183,116.861437446236));
#53131=CARTESIAN_POINT('Ctrl Pts',(17.0938117001638,-0.504232219701305,
116.910623011974));
#53132=CARTESIAN_POINT('Ctrl Pts',(17.5729853188264,-1.18048171398732,116.960045601005));
#53133=CARTESIAN_POINT('Ctrl Pts',(18.3420871113973,-1.49965465644313,117.009700188431));
#53134=CARTESIAN_POINT('Ctrl Pts',(19.1668659216703,-1.36005147654203,117.05958143723));
#53135=CARTESIAN_POINT('Ctrl Pts',(19.7937047525059,-0.800566639011249,
117.109683748806));
#53136=CARTESIAN_POINT('Ctrl Pts',(20.0277875120747,0.0101379512286132,
117.160001253962));
#53137=CARTESIAN_POINT('Ctrl Pts',(19.7936847629856,0.824483128183414,117.210527832844));
#53138=CARTESIAN_POINT('Ctrl Pts',(19.1596616311847,1.39171327988103,117.261257100749));
#53139=CARTESIAN_POINT('Ctrl Pts',(18.3177908939756,1.53521530422674,117.312182432211));
#53140=CARTESIAN_POINT('Ctrl Pts',(17.5256836268175,1.20758890493412,117.363296973471));
#53141=CARTESIAN_POINT('Ctrl Pts',(17.0275455794861,0.506255522428237,117.414593637324));
#53142=CARTESIAN_POINT('Ctrl Pts',(16.9787373259702,-0.35553973474002,117.466065106827));
#53143=CARTESIAN_POINT('Ctrl Pts',(17.3973002169671,-1.11364573044326,117.517703870815));
#53144=CARTESIAN_POINT('Ctrl Pts',(18.1573683126717,-1.53416286108214,117.569502207969));
#53145=CARTESIAN_POINT('Ctrl Pts',(19.0272538362356,-1.48564336837537,117.621452211899));
#53146=CARTESIAN_POINT('Ctrl Pts',(19.7398503747652,-0.980418717802992,
117.673545759339));
#53147=CARTESIAN_POINT('Ctrl Pts',(20.0754586522521,-0.171264234164207,
117.725774634931));
#53148=CARTESIAN_POINT('Ctrl Pts',(19.9528984809521,0.549983689228882,117.769404367946));
#53149=CARTESIAN_POINT('Ctrl Pts',(19.6356116093765,1.02260359458153,117.804367384591));
#53150=CARTESIAN_POINT('Ctrl Pts',(19.2010969873656,1.39125738920211,117.839368176335));
#53151=CARTESIAN_POINT('Ctrl Pts',(18.4951761944866,1.59511231389331,117.883187939005));
#53152=CARTESIAN_POINT('Ctrl Pts',(17.6460434343933,1.35061332593586,117.935872096955));
#53153=CARTESIAN_POINT('Ctrl Pts',(17.0561860951254,0.69088986844999,117.988648088627));
#53154=CARTESIAN_POINT('Ctrl Pts',(16.9074971438262,-0.183028294006347,
118.041506623448));
#53155=CARTESIAN_POINT('Ctrl Pts',(17.2470534207198,-1.00316234166999,118.094438626915));
#53156=CARTESIAN_POINT('Ctrl Pts',(17.9717910595105,-1.51758676734159,118.14743475339));
#53157=CARTESIAN_POINT('Ctrl Pts',(18.8600432872684,-1.56756420344383,118.200485682854));
#53158=CARTESIAN_POINT('Ctrl Pts',(19.6394161118673,-1.13697309564611,118.253581949951));
#53159=CARTESIAN_POINT('Ctrl Pts',(20.0704659672594,-0.357096634960048,
118.306714148656));
#53160=CARTESIAN_POINT('Ctrl Pts',(20.0205702328933,0.532844361309807,118.359872635996));
#53161=CARTESIAN_POINT('Ctrl Pts',(19.504486863852,1.26036618044964,118.413048064539));
#53162=CARTESIAN_POINT('Ctrl Pts',(18.8180055338568,1.54444373835792,118.457366755587));
#53163=CARTESIAN_POINT('Ctrl Pts',(18.2407925832158,1.52713411330168,118.492820814792));
#53164=CARTESIAN_POINT('Ctrl Pts',(17.8284336500578,1.39613252265381,118.519409239185));
#53165=CARTESIAN_POINT('Ctrl Pts',(17.4685051427223,1.1554090378971,118.545995092116));
#53166=CARTESIAN_POINT('Ctrl Pts',(17.1893258099538,0.824898120829929,118.572576342922));
#53167=CARTESIAN_POINT('Ctrl Pts',(17.0125879486417,0.429862370286751,118.599152630315));
#53168=CARTESIAN_POINT('Ctrl Pts',(16.9521470208911,0.00161163153818327,
118.625721994921));
#53169=CARTESIAN_POINT('Ctrl Pts',(17.0125764443851,-0.42667872826605,118.652283949504));
#53170=CARTESIAN_POINT('Ctrl Pts',(17.1597806759054,-0.755367532112567,
118.674411046438));
#53171=CARTESIAN_POINT('Ctrl Pts',(17.3285403893103,-0.986405868394619,
118.692108255428));
#53172=CARTESIAN_POINT('Ctrl Pts',(17.5279443674188,-1.19111295414712,118.70980104078));
#53173=CARTESIAN_POINT('Ctrl Pts',(17.9466035736572,-1.47210445803857,118.740754696099));
#53174=CARTESIAN_POINT('Ctrl Pts',(18.6767611048209,-1.59634272918696,118.784942220793));
#53175=CARTESIAN_POINT('Ctrl Pts',(19.4977275477546,-1.25611034638129,118.837908121638));
#53176=CARTESIAN_POINT('Ctrl Pts',(19.9249220966151,-0.65331003248227,118.881989304197));
#53177=CARTESIAN_POINT('Ctrl Pts',(20.0218459481189,-0.160631817687348,
118.912811545655));
#53178=CARTESIAN_POINT('Ctrl Pts',(20.0180508629822,0.12358736647769,118.930414576253));
#53179=CARTESIAN_POINT('Ctrl Pts',(19.9743985426673,0.404842513306318,118.948009763686));
#53180=CARTESIAN_POINT('Ctrl Pts',(19.8465496236101,0.738729994358177,118.969990762044));
#53181=CARTESIAN_POINT('Ctrl Pts',(19.503237250369,1.19676088527163,119.00512939206));
#53182=CARTESIAN_POINT('Ctrl Pts',(18.8596729577346,1.55243356672786,119.048992892846));
#53183=CARTESIAN_POINT('Ctrl Pts',(17.9799831327098,1.50276019726124,119.101523819356));
#53184=CARTESIAN_POINT('Ctrl Pts',(17.263212307717,0.993819888846933,119.153941103703));
#53185=CARTESIAN_POINT('Ctrl Pts',(16.9839792247278,0.318663513392033,119.197519819886));
#53186=CARTESIAN_POINT('Ctrl Pts',(17.001110435418,-0.247819246073101,119.232317729451));
#53187=CARTESIAN_POINT('Ctrl Pts',(17.1079830203791,-0.584651791505382,
119.254037650762));
#53188=CARTESIAN_POINT('Ctrl Pts',(17.2300818521728,-0.797813714445423,
119.269226964678));
#53189=CARTESIAN_POINT('Ctrl Pts',(17.3117280880498,-0.9113604666153,119.277901992599));
#53190=CARTESIAN_POINT('Ctrl Pts',(17.4012920935501,-1.0188850040393,119.286574041755));
#53191=CARTESIAN_POINT('Ctrl Pts',(17.5267955079385,-1.14092085905138,119.297408117074));
#53192=CARTESIAN_POINT('Ctrl Pts',(17.7528270107813,-1.30615819007779,119.31473153276));
#53193=CARTESIAN_POINT('Ctrl Pts',(18.0742528290313,-1.44998548783811,119.336361940194));
#53194=CARTESIAN_POINT('Ctrl Pts',(18.4921163795425,-1.50892176698877,119.362281087325));
#53195=CARTESIAN_POINT('Ctrl Pts',(18.9093083092125,-1.44998013204778,119.388160932157));
#53196=CARTESIAN_POINT('Ctrl Pts',(19.2932994283458,-1.27810698095492,119.414001246931));
#53197=CARTESIAN_POINT('Ctrl Pts',(19.6141891347275,-1.00707517579684,119.43980038992));
#53198=CARTESIAN_POINT('Ctrl Pts',(19.8471250805189,-0.658373354783552,
119.465558201273));
#53199=CARTESIAN_POINT('Ctrl Pts',(19.9742228972475,-0.259467245505255,
119.491272617658));
#53200=CARTESIAN_POINT('Ctrl Pts',(19.9858753700794,0.158301952850977,119.516944194725));
#53201=CARTESIAN_POINT('Ctrl Pts',(19.8990241695029,0.494979507521757,119.538299135457));
#53202=CARTESIAN_POINT('Ctrl Pts',(19.7757742210683,0.741612695103491,119.555361011189));
#53203=CARTESIAN_POINT('Ctrl Pts',(19.58069155028,1.0254111001558,119.576668756615));
#53204=CARTESIAN_POINT('Ctrl Pts',(19.2012637945808,1.33666302774039,119.606445571674));
#53205=CARTESIAN_POINT('Ctrl Pts',(18.59413116038,1.50218145374168,119.644622711453));
#53206=CARTESIAN_POINT('Ctrl Pts',(17.9741889539315,1.40557451760412,119.682689594233));
#53207=CARTESIAN_POINT('Ctrl Pts',(17.4493194520646,1.0651884348338,119.720643422888));
#53208=CARTESIAN_POINT('Ctrl Pts',(17.1103034219914,0.541698384717174,119.758481493696));
#53209=CARTESIAN_POINT('Ctrl Pts',(17.0149844688412,-0.0726480667363822,
119.796201073521));
#53210=CARTESIAN_POINT('Ctrl Pts',(17.1783582983629,-0.670477000498041,
119.833799757369));
#53211=CARTESIAN_POINT('Ctrl Pts',(17.5050878418038,-1.06819893534445,119.865028891154));
#53212=CARTESIAN_POINT('Ctrl Pts',(17.8458525729069,-1.28516330407485,119.889949495029));
#53213=CARTESIAN_POINT('Ctrl Pts',(18.2235157805367,-1.42666993037966,119.914827505529));
#53214=CARTESIAN_POINT('Ctrl Pts',(18.7343004495072,-1.44806142418328,119.945845031736));
#53215=CARTESIAN_POINT('Ctrl Pts',(19.3022641117884,-1.22179759041786,119.98293553694));
#53216=CARTESIAN_POINT('Ctrl Pts',(19.7267504298182,-0.784916367409439,
120.019893470825));
#53217=CARTESIAN_POINT('Ctrl Pts',(19.9350082684945,-0.214809342616007,
120.056716728399));
#53218=CARTESIAN_POINT('Ctrl Pts',(19.8923964259192,0.388373946010418,120.093403372529));
#53219=CARTESIAN_POINT('Ctrl Pts',(19.6082151774614,0.919535325612133,120.129951516022));
#53220=CARTESIAN_POINT('Ctrl Pts',(19.1336807132418,1.28688374926404,120.166359391381));
#53221=CARTESIAN_POINT('Ctrl Pts',(18.5527927781208,1.42780271129681,120.202625307385));
#53222=CARTESIAN_POINT('Ctrl Pts',(17.9672849430062,1.31962837356636,120.238747690412));
#53223=CARTESIAN_POINT('Ctrl Pts',(17.5604664448896,1.03912928877408,120.268728808256));
#53224=CARTESIAN_POINT('Ctrl Pts',(17.3255478081665,0.730808963275233,120.29264048669));
#53225=CARTESIAN_POINT('Ctrl Pts',(17.1598505083254,0.381251616548514,120.316503198891));
#53226=CARTESIAN_POINT('Ctrl Pts',(17.0983099735108,-0.104991940913315,
120.34623918748));
#53227=CARTESIAN_POINT('Ctrl Pts',(17.2685940660949,-0.665398892142992,
120.381773515751));
#53228=CARTESIAN_POINT('Ctrl Pts',(17.6512792739107,-1.10550385025771,120.41715783718));
#53229=CARTESIAN_POINT('Ctrl Pts',(18.1781005502915,-1.34987930889349,120.452391196463));
#53230=CARTESIAN_POINT('Ctrl Pts',(18.7562794468606,-1.35772126535799,120.487472684011));
#53231=CARTESIAN_POINT('Ctrl Pts',(19.2849262650991,-1.12972301595998,120.522401531095));
#53232=CARTESIAN_POINT('Ctrl Pts',(19.6726290138236,-0.707545247949752,
120.557177051768));
#53233=CARTESIAN_POINT('Ctrl Pts',(19.8532773460226,-0.16623998601176,120.59179867559));
#53234=CARTESIAN_POINT('Ctrl Pts',(19.797325294628,0.399107448838622,120.626265930169));
#53235=CARTESIAN_POINT('Ctrl Pts',(19.516604963237,0.890078600748408,120.66057845095));
#53236=CARTESIAN_POINT('Ctrl Pts',(19.0618960487862,1.22206271419135,120.694735976808));
#53237=CARTESIAN_POINT('Ctrl Pts',(18.5137492588806,1.33883473443734,120.728738352884));
#53238=CARTESIAN_POINT('Ctrl Pts',(17.968216849916,1.22206908408025,120.762585529099));
#53239=CARTESIAN_POINT('Ctrl Pts',(17.5200207911922,0.894176786428842,120.796277560609));
#53240=CARTESIAN_POINT('Ctrl Pts',(17.2461072346647,0.414037560067,120.829814607784));
#53241=CARTESIAN_POINT('Ctrl Pts',(17.1924430147546,-0.133565974408157,
120.863196936287));
#53242=CARTESIAN_POINT('Ctrl Pts',(17.366317551762,-0.652915584466722,120.896424916945));
#53243=CARTESIAN_POINT('Ctrl Pts',(17.7354356853631,-1.05408452248002,120.929499025204));
#53244=CARTESIAN_POINT('Ctrl Pts',(18.2338946800392,-1.26850207170023,120.962419840475));
#53245=CARTESIAN_POINT('Ctrl Pts',(18.7739421572114,-1.26066264713202,120.995188046564));
#53246=CARTESIAN_POINT('Ctrl Pts',(19.261417515124,-1.03398313097046,121.02780443056));
#53247=CARTESIAN_POINT('Ctrl Pts',(19.6121606614966,-0.629846282234725,
121.060269883735));
#53248=CARTESIAN_POINT('Ctrl Pts',(19.7665300506899,-0.120063655066437,
121.092585397355));
#53249=CARTESIAN_POINT('Ctrl Pts',(19.6995288695014,0.405875592196416,121.124752068354));
#53250=CARTESIAN_POINT('Ctrl Pts',(19.4248220741339,0.856499430305402,121.156771086707));
#53251=CARTESIAN_POINT('Ctrl Pts',(18.9920077149049,1.15425452722384,121.188643758256));
#53252=CARTESIAN_POINT('Ctrl Pts',(18.477675702841,1.24882569485176,121.22037145959));
#53253=CARTESIAN_POINT('Ctrl Pts',(17.9718722366947,1.12564015935962,121.25195571884));
#53254=CARTESIAN_POINT('Ctrl Pts',(17.5623444137067,0.808028409142753,121.283398060944));
#53255=CARTESIAN_POINT('Ctrl Pts',(17.3193477993976,0.35291029010133,121.314700295335));
#53256=CARTESIAN_POINT('Ctrl Pts',(17.2835915860888,-0.159531772662667,
121.345863968405));
#53257=CARTESIAN_POINT('Ctrl Pts',(17.4155057372333,-0.519645729494795,
121.369134581872));
#53258=CARTESIAN_POINT('Ctrl Pts',(17.5594893836391,-0.723752038926638,
121.384605922907));
#53259=CARTESIAN_POINT('Ctrl Pts',(17.668999693357,-0.848911852993158,121.39490936142));
#53260=CARTESIAN_POINT('Ctrl Pts',(17.8931906723513,-1.03579597290683,121.412910620692));
#53261=CARTESIAN_POINT('Ctrl Pts',(18.2857522897131,-1.19187578457209,121.438544180847));
#53262=CARTESIAN_POINT('Ctrl Pts',(18.7902002679314,-1.17038056405782,121.469173977415));
#53263=CARTESIAN_POINT('Ctrl Pts',(19.2399332524197,-0.945736597983726,
121.499675716141));
#53264=CARTESIAN_POINT('Ctrl Pts',(19.5574022269321,-0.558563760582848,
121.530051638976));
#53265=CARTESIAN_POINT('Ctrl Pts',(19.6884983642052,-0.0774725349686712,
121.560304199798));
#53266=CARTESIAN_POINT('Ctrl Pts',(19.6119798866289,0.413247003691924,121.590435869102));
#53267=CARTESIAN_POINT('Ctrl Pts',(19.3427638331946,0.828274604425165,121.620449235126));
#53268=CARTESIAN_POINT('Ctrl Pts',(18.9291167211882,1.09611529685852,121.650346948405));
#53269=CARTESIAN_POINT('Ctrl Pts',(18.4439871351089,1.17136126566376,121.680131747619));
#53270=CARTESIAN_POINT('Ctrl Pts',(17.9721852197242,1.04237957129896,121.709806443118));
#53271=CARTESIAN_POINT('Ctrl Pts',(17.5955767614254,0.733067066500168,121.739373920544));
#53272=CARTESIAN_POINT('Ctrl Pts',(17.3789145552552,0.298448464042141,121.768837139486));
#53273=CARTESIAN_POINT('Ctrl Pts',(17.3587311152265,-0.185091286281474,
121.798199127953));
#53274=CARTESIAN_POINT('Ctrl Pts',(17.5372040232563,-0.633201450870468,
121.827462989564));
#53275=CARTESIAN_POINT('Ctrl Pts',(17.882013145033,-0.968245111307221,121.856631880607));
#53276=CARTESIAN_POINT('Ctrl Pts',(18.3321736501231,-1.13271867310312,121.885709046681));
#53277=CARTESIAN_POINT('Ctrl Pts',(18.8087973084627,-1.09908843399563,121.914697746937));
#53278=CARTESIAN_POINT('Ctrl Pts',(19.2288806489506,-0.874386164600571,
121.943601393848));
#53279=CARTESIAN_POINT('Ctrl Pts',(19.5197284804084,-0.498764010730529,
121.972423284531));
#53280=CARTESIAN_POINT('Ctrl Pts',(19.631488858918,-0.0383710896155189,
122.001167096572));
#53281=CARTESIAN_POINT('Ctrl Pts',(19.5456822019558,0.42631741060901,122.029836034946));
#53282=CARTESIAN_POINT('Ctrl Pts',(19.2782376706958,0.814460654457481,122.058433950357));
#53283=CARTESIAN_POINT('Ctrl Pts',(18.8765333476415,1.05894522909086,122.086964325726));
#53284=CARTESIAN_POINT('Ctrl Pts',(18.411053545632,1.11790498477854,122.115430833469));
#53285=CARTESIAN_POINT('Ctrl Pts',(17.9630346452634,0.981894731140524,122.143837222082));
#53286=CARTESIAN_POINT('Ctrl Pts',(17.6103416604701,0.675370135250457,122.172187197682));
#53287=CARTESIAN_POINT('Ctrl Pts',(17.4139663666992,0.252314060233207,122.200484547726));
#53288=CARTESIAN_POINT('Ctrl Pts',(17.4075180258619,-0.213249102834493,
122.228733136097));
#53289=CARTESIAN_POINT('Ctrl Pts',(17.5914890882151,-0.640162939071301,
122.256936743679));
#53290=CARTESIAN_POINT('Ctrl Pts',(17.9332829313857,-0.954248513992901,
122.285099331242));
#53291=CARTESIAN_POINT('Ctrl Pts',(18.3729700883329,-1.10114856672374,122.313224762676));
#53292=CARTESIAN_POINT('Ctrl Pts',(18.8337656364914,-1.0557099732899,122.341316973501));
#53293=CARTESIAN_POINT('Ctrl Pts',(19.2353976864752,-0.826269100476284,
122.369379975043));
#53294=CARTESIAN_POINT('Ctrl Pts',(19.5080473835103,-0.453137156095097,
122.397417661645));
#53295=CARTESIAN_POINT('Ctrl Pts',(19.6044460345045,-0.00152756021506351,
122.425434134331));
#53296=CARTESIAN_POINT('Ctrl Pts',(19.5080490631313,0.449785662790224,122.453433287289));
#53297=CARTESIAN_POINT('Ctrl Pts',(19.2358501405623,0.822201779793111,122.481419310144));
#53298=CARTESIAN_POINT('Ctrl Pts',(18.8354297261873,1.05088321709065,122.509395984532));
#53299=CARTESIAN_POINT('Ctrl Pts',(18.3766008448291,1.09606510988091,122.537367609601));
#53300=CARTESIAN_POINT('Ctrl Pts',(17.9393577912152,0.949926431334445,122.565338058587));
#53301=CARTESIAN_POINT('Ctrl Pts',(17.5998948604504,0.637888425774447,122.593311446551));
#53302=CARTESIAN_POINT('Ctrl Pts',(17.4174396576394,0.214366012794586,122.621291806824));
#53303=CARTESIAN_POINT('Ctrl Pts',(17.4231623787231,-0.1957658757123,122.646172972246));
#53304=CARTESIAN_POINT('Ctrl Pts',(17.5499930456385,-0.526830239172015,
122.667953798238));
#53305=CARTESIAN_POINT('Ctrl Pts',(17.7932141540085,-0.851346049715726,
122.692856554516));
#53306=CARTESIAN_POINT('Ctrl Pts',(18.2501761462134,-1.10418600330839,122.72400778286));
#53307=CARTESIAN_POINT('Ctrl Pts',(18.8769616675777,-1.06908370626514,122.761434859433));
#53308=CARTESIAN_POINT('Ctrl Pts',(19.3896239215073,-0.70545262307287,122.798917126171));
#53309=CARTESIAN_POINT('Ctrl Pts',(19.6307566921668,-0.12384402484574,122.836463844081));
#53310=CARTESIAN_POINT('Ctrl Pts',(19.5252616357798,0.498282873588724,122.874084352006));
#53311=CARTESIAN_POINT('Ctrl Pts',(19.1742691062997,0.891055442512747,122.905503881039));
#53312=CARTESIAN_POINT('Ctrl Pts',(18.7996171429706,1.05785424932804,122.930685519148));
#53313=CARTESIAN_POINT('Ctrl Pts',(18.5061980272808,1.09969585165476,122.948895536135));
#53314=CARTESIAN_POINT('Ctrl Pts',(18.2235705570867,1.06394203818006,122.966427195679));
#53315=CARTESIAN_POINT('Ctrl Pts',(17.8835419458233,0.931126744519063,122.988895417304));
#53316=CARTESIAN_POINT('Ctrl Pts',(17.540325572912,0.612977032071075,123.017034360395));
#53317=CARTESIAN_POINT('Ctrl Pts',(17.3907978799752,0.168200478695434,123.045250354356));
#53318=CARTESIAN_POINT('Ctrl Pts',(17.4097069157206,-0.198885785314081,
123.067872011256));
#53319=CARTESIAN_POINT('Ctrl Pts',(17.5175585534041,-0.550747043662346,
123.090527691658));
#53320=CARTESIAN_POINT('Ctrl Pts',(17.811694265428,-0.920088885831626,123.118912113209));
#53321=CARTESIAN_POINT('Ctrl Pts',(18.2916876292038,-1.12241961155101,123.150236055638));
#53322=CARTESIAN_POINT('Ctrl Pts',(18.7599954609617,-1.10466062303536,123.178796710933));
#53323=CARTESIAN_POINT('Ctrl Pts',(19.1475491472277,-0.935850007334233,
123.204568881909));
#53324=CARTESIAN_POINT('Ctrl Pts',(19.4474303836746,-0.636042641389887,
123.230410947105));
#53325=CARTESIAN_POINT('Ctrl Pts',(19.6175361159645,-0.246469240807822,
123.256325134572));
#53326=CARTESIAN_POINT('Ctrl Pts',(19.6336055704725,0.179639336476098,123.282313928802));
#53327=CARTESIAN_POINT('Ctrl Pts',(19.4924664396755,0.583268923924529,123.308379216194));
#53328=CARTESIAN_POINT('Ctrl Pts',(19.2594187855067,0.854320734565662,123.330166333392));
#53329=CARTESIAN_POINT('Ctrl Pts',(19.0225876601379,1.00901198977016,123.347636263176));
#53330=CARTESIAN_POINT('Ctrl Pts',(18.7174728526583,1.13601015551723,123.368049966962));
#53331=CARTESIAN_POINT('Ctrl Pts',(18.2558875246191,1.15934765713978,123.395834765122));
#53332=CARTESIAN_POINT('Ctrl Pts',(17.8157869453812,0.947553194065168,123.425209130312));
#53333=CARTESIAN_POINT('Ctrl Pts',(17.5553879829031,0.666356292508678,123.448787444948));
#53334=CARTESIAN_POINT('Ctrl Pts',(17.4178065523958,0.413637397213519,123.466510938034));
#53335=CARTESIAN_POINT('Ctrl Pts',(17.3221820932953,0.0406364433144716,
123.490196526986));
#53336=CARTESIAN_POINT('Ctrl Pts',(17.3772635808422,-0.400356807765698,
123.516935032653));
#53337=CARTESIAN_POINT('Ctrl Pts',(17.637978375011,-0.814840216527707,123.546767553284));
#53338=CARTESIAN_POINT('Ctrl Pts',(18.0081494220083,-1.08849077489295,123.574836116967));
#53339=CARTESIAN_POINT('Ctrl Pts',(18.4775112774984,-1.20283620753728,123.604140665495));
#53340=CARTESIAN_POINT('Ctrl Pts',(18.9728689947087,-1.11170713766108,123.634699102384));
#53341=CARTESIAN_POINT('Ctrl Pts',(19.3548250710418,-0.848888554637065,
123.662829393191));
#53342=CARTESIAN_POINT('Ctrl Pts',(19.543864380145,-0.572027787550067,123.683364369092));
#53343=CARTESIAN_POINT('Ctrl Pts',(19.6489401612735,-0.315921957158224,
123.700513727019));
#53344=CARTESIAN_POINT('Ctrl Pts',(19.7008713985811,-0.0552588957866882,
123.716838067645));
#53345=CARTESIAN_POINT('Ctrl Pts',(19.6726256840306,0.280232965878121,123.737517870146));
#53346=CARTESIAN_POINT('Ctrl Pts',(19.5522795280404,0.595728848538907,123.7582584388));
#53347=CARTESIAN_POINT('Ctrl Pts',(19.3486831682667,0.866369771861213,123.779059848981));
#53348=CARTESIAN_POINT('Ctrl Pts',(19.0773416884718,1.07066171040279,123.799923006162));
#53349=CARTESIAN_POINT('Ctrl Pts',(18.7855851467281,1.18212492987368,123.819104474902));
#53350=CARTESIAN_POINT('Ctrl Pts',(18.5041991856914,1.21572785039616,123.836587848181));
#53351=CARTESIAN_POINT('Ctrl Pts',(18.1646934338967,1.18499174658801,123.857615096215));
#53352=CARTESIAN_POINT('Ctrl Pts',(17.7653832410379,1.01332364019048,123.883988407248));
#53353=CARTESIAN_POINT('Ctrl Pts',(17.4105724745461,0.627640142468378,123.91578041595));
#53354=CARTESIAN_POINT('Ctrl Pts',(17.2434553757277,0.12848973275699,123.947718069321));
#53355=CARTESIAN_POINT('Ctrl Pts',(17.2950338468023,-0.397842330961294,
123.979802636553));
#53356=CARTESIAN_POINT('Ctrl Pts',(17.5582954032972,-0.859299372811185,
124.012035412185));
#53357=CARTESIAN_POINT('Ctrl Pts',(17.9890647139176,-1.17444949802056,124.044417524025));
#53358=CARTESIAN_POINT('Ctrl Pts',(18.5134073925165,-1.28668013802211,124.076950033579));
#53359=CARTESIAN_POINT('Ctrl Pts',(19.040299183268,-1.17444205619667,124.109633881169));
#53360=CARTESIAN_POINT('Ctrl Pts',(19.477419740777,-0.855306063337771,124.142469914755));
#53361=CARTESIAN_POINT('Ctrl Pts',(19.747318196117,-0.383277623495378,124.175458873959));
#53362=CARTESIAN_POINT('Ctrl Pts',(19.8011287001543,0.160339974187855,124.20860139743));
#53363=CARTESIAN_POINT('Ctrl Pts',(19.6274041961022,0.680932515573491,124.241898017848));
#53364=CARTESIAN_POINT('Ctrl Pts',(19.2544751124545,1.08703964110571,124.275349164061));
#53365=CARTESIAN_POINT('Ctrl Pts',(18.7458556784281,1.30641671855503,124.308955159866));
#53366=CARTESIAN_POINT('Ctrl Pts',(18.189437375636,1.29888227807384,124.342716224406));
#53367=CARTESIAN_POINT('Ctrl Pts',(17.6823055406022,1.06366182687317,124.37663247134));
#53368=CARTESIAN_POINT('Ctrl Pts',(17.3138010055331,0.639890347952039,124.410703908926));
#53369=CARTESIAN_POINT('Ctrl Pts',(17.1497814706464,0.100118900233251,124.444930440075));
#53370=CARTESIAN_POINT('Ctrl Pts',(17.2208555754922,-0.462100903720547,
124.479311862771));
#53371=CARTESIAN_POINT('Ctrl Pts',(17.5166919909782,-0.948431814978525,
124.513847869957));
#53372=CARTESIAN_POINT('Ctrl Pts',(17.9874589398796,-1.27295449876341,124.548538049416));
#53373=CARTESIAN_POINT('Ctrl Pts',(18.5522074356213,-1.37734955352004,124.583381884254));
#53374=CARTESIAN_POINT('Ctrl Pts',(19.1127907478127,-1.24137444588285,124.61837875334));
#53375=CARTESIAN_POINT('Ctrl Pts',(19.570927231329,-0.886752979347359,124.653527932135));
#53376=CARTESIAN_POINT('Ctrl Pts',(19.8454390955441,-0.373734529845406,
124.6888285926));
#53377=CARTESIAN_POINT('Ctrl Pts',(19.8866416789606,0.209138420975833,124.724279803654));
#53378=CARTESIAN_POINT('Ctrl Pts',(19.6853313203903,0.760317927546962,124.759880531932));
#53379=CARTESIAN_POINT('Ctrl Pts',(19.274746020493,1.18295333165501,124.795629642769));
#53380=CARTESIAN_POINT('Ctrl Pts',(18.7250932562895,1.40192119416919,124.831525901343));
#53381=CARTESIAN_POINT('Ctrl Pts',(18.1315421099629,1.37718539583083,124.8675679727));
#53382=CARTESIAN_POINT('Ctrl Pts',(17.5977335091393,1.11110962070016,124.90375442263));
#53383=CARTESIAN_POINT('Ctrl Pts',(17.2176675190692,0.648387246466477,124.940083718826));
#53384=CARTESIAN_POINT('Ctrl Pts',(17.0591358261671,0.0685399773490914,
124.976554232237));
#53385=CARTESIAN_POINT('Ctrl Pts',(17.1516223906728,-0.527757683984189,
125.013164238674));
#53386=CARTESIAN_POINT('Ctrl Pts',(17.4808337728012,-1.03617512245347,125.049911918955));
#53387=CARTESIAN_POINT('Ctrl Pts',(17.9908722758733,-1.36699968915259,125.086795359982));
#53388=CARTESIAN_POINT('Ctrl Pts',(18.5937293060452,-1.46098376939424,125.123812556508));
#53389=CARTESIAN_POINT('Ctrl Pts',(19.1844869028144,-1.29996231384015,125.160961412641));
#53390=CARTESIAN_POINT('Ctrl Pts',(19.6595994719402,-0.910336227375098,
125.198239744056));
#53391=CARTESIAN_POINT('Ctrl Pts',(19.935066233012,-0.358757208946706,125.235645278193));
#53392=CARTESIAN_POINT('Ctrl Pts',(19.9613007891063,0.259283810673803,125.273175655495));
#53393=CARTESIAN_POINT('Ctrl Pts',(19.7320620910867,0.836009611459873,125.310828431745));
#53394=CARTESIAN_POINT('Ctrl Pts',(19.2858368185977,1.27017821405643,125.348601079706));
#53395=CARTESIAN_POINT('Ctrl Pts',(18.6993793782574,1.48488146702807,125.386490991953));
#53396=CARTESIAN_POINT('Ctrl Pts',(18.0744929819311,1.44118677993217,125.424495481034));
#53397=CARTESIAN_POINT('Ctrl Pts',(17.5203309456295,1.14519868643357,125.462611781001));
#53398=CARTESIAN_POINT('Ctrl Pts',(17.1342996581372,0.647258515357208,125.500837050006));
#53399=CARTESIAN_POINT('Ctrl Pts',(16.9849097134977,0.0333749870028357,
125.539168372337));
#53400=CARTESIAN_POINT('Ctrl Pts',(17.0995994614457,-0.589654791868995,
125.577602761599));
#53401=CARTESIAN_POINT('Ctrl Pts',(17.4596986530298,-1.11285616969424,125.616137161058));
#53402=CARTESIAN_POINT('Ctrl Pts',(18.0034565556922,-1.44417105987669,125.654768445165));
#53403=CARTESIAN_POINT('Ctrl Pts',(18.6366460765495,-1.52468380343448,125.693493422678));
#53404=CARTESIAN_POINT('Ctrl Pts',(19.2489206681697,-1.33911367710705,125.732308838738));
#53405=CARTESIAN_POINT('Ctrl Pts',(19.7330798824833,-0.918702162929582,
125.771211378595));
#53406=CARTESIAN_POINT('Ctrl Pts',(20.003873712581,-0.335951044009737,125.810197667968));
#53407=CARTESIAN_POINT('Ctrl Pts',(20.0130409900718,0.307902407747933,125.849264274755));
#53408=CARTESIAN_POINT('Ctrl Pts',(19.7579238844887,0.900506033918292,125.888407712264));
#53409=CARTESIAN_POINT('Ctrl Pts',(19.282118126251,1.3380365586316,125.927624441706));
#53410=CARTESIAN_POINT('Ctrl Pts',(18.6680121178992,1.54342523826848,125.966910876023));
#53411=CARTESIAN_POINT('Ctrl Pts',(18.0224934653108,1.479959447458,126.006263380594));
#53412=CARTESIAN_POINT('Ctrl Pts',(17.4583073090084,1.1578549526847,126.045678274836));
#53413=CARTESIAN_POINT('Ctrl Pts',(17.0743240513896,0.632620214794982,126.08515183572));
#53414=CARTESIAN_POINT('Ctrl Pts',(16.9381771242321,-0.00452739822763612,
126.124680300394));
#53415=CARTESIAN_POINT('Ctrl Pts',(17.0743261534331,-0.64253589142097,126.164259870224));
#53416=CARTESIAN_POINT('Ctrl Pts',(17.4596567592957,-1.16991519259679,126.203886711707));
#53417=CARTESIAN_POINT('Ctrl Pts',(18.0274097244559,-1.49426106398949,126.243556958088));
#53418=CARTESIAN_POINT('Ctrl Pts',(18.6787710739259,-1.55848016466035,126.283266712911));
#53419=CARTESIAN_POINT('Ctrl Pts',(19.3001068465522,-1.35086105258382,126.323012052985));
#53420=CARTESIAN_POINT('Ctrl Pts',(19.7828302049358,-0.907210804819137,
126.36278903232));
#53421=CARTESIAN_POINT('Ctrl Pts',(20.0424196828473,-0.304667060645809,
126.402593683509));
#53422=CARTESIAN_POINT('Ctrl Pts',(20.0332506859797,0.351742851216847,126.442422019401));
#53423=CARTESIAN_POINT('Ctrl Pts',(19.7566314877895,0.947449108115339,126.4822700359));
#53424=CARTESIAN_POINT('Ctrl Pts',(19.2606259379933,1.37838027922372,126.522133716601));
#53425=CARTESIAN_POINT('Ctrl Pts',(18.6316832039008,1.56918550021926,126.562009034018));
#53426=CARTESIAN_POINT('Ctrl Pts',(17.9795384681277,1.4864383553722,126.601891956083));
#53427=CARTESIAN_POINT('Ctrl Pts',(17.4180219901316,1.14450714080288,126.64177843909));
#53428=CARTESIAN_POINT('Ctrl Pts',(17.0451507093673,0.60305178731209,126.681664446109));
#53429=CARTESIAN_POINT('Ctrl Pts',(16.9259721145279,-0.0434035665844907,
126.721545922569));
#53430=CARTESIAN_POINT('Ctrl Pts',(17.0812073691357,-0.682018342919702,
126.761418852013));
#53431=CARTESIAN_POINT('Ctrl Pts',(17.48361106064,-1.20135795626228,126.801279160675));
#53432=CARTESIAN_POINT('Ctrl Pts',(18.0628189959856,-1.51091507882325,126.841122901587));
#53433=CARTESIAN_POINT('Ctrl Pts',(18.7175753989508,-1.55685481943617,126.880945914479));
#53434=CARTESIAN_POINT('Ctrl Pts',(19.3336690282003,-1.33151582505569,126.920744475439));
#53435=CARTESIAN_POINT('Ctrl Pts',(19.7252122247228,-0.950635904975706,
126.95388579676));
#53436=CARTESIAN_POINT('Ctrl Pts',(19.9246599065469,-0.570211393078723,
126.980382990007));
#53437=CARTESIAN_POINT('Ctrl Pts',(20.0410084568928,-0.156926761860616,
127.00686812107));
#53438=CARTESIAN_POINT('Ctrl Pts',(20.0180960753438,0.387885002702108,127.03995229568));
#53439=CARTESIAN_POINT('Ctrl Pts',(19.7261197888881,0.972790423017701,127.079612454345));
#53440=CARTESIAN_POINT('Ctrl Pts',(19.2213375973188,1.38696677386596,127.119228496333));
#53441=CARTESIAN_POINT('Ctrl Pts',(18.5921407553839,1.55862427081998,127.158796244357));
#53442=CARTESIAN_POINT('Ctrl Pts',(17.9485754461998,1.45844625626644,127.19831204202));
#53443=CARTESIAN_POINT('Ctrl Pts',(17.4028219204161,1.10463821938839,127.237772008334));
#53444=CARTESIAN_POINT('Ctrl Pts',(17.0497229688341,0.55959920647719,127.277172437709));
#53445=CARTESIAN_POINT('Ctrl Pts',(16.9502018159956,-0.0810954772450534,
127.316509591208));
#53446=CARTESIAN_POINT('Ctrl Pts',(17.1207658108625,-0.705493479039353,
127.355779812835));
#53447=CARTESIAN_POINT('Ctrl Pts',(17.5307517205212,-1.20486476242342,127.39497947225));
#53448=CARTESIAN_POINT('Ctrl Pts',(18.107855145551,-1.49267495326757,127.434104996807));
#53449=CARTESIAN_POINT('Ctrl Pts',(18.7509009483514,-1.51960879688507,127.473152857691));
#53450=CARTESIAN_POINT('Ctrl Pts',(19.3476186900617,-1.28203401909253,127.512119582085));
#53451=CARTESIAN_POINT('Ctrl Pts',(19.7942807409555,-0.822448911396595,
127.551001750383));
#53452=CARTESIAN_POINT('Ctrl Pts',(20.013768325998,-0.221869682102491,127.589796006502));
#53453=CARTESIAN_POINT('Ctrl Pts',(19.9689094941412,0.414477136693096,127.628499035169));
#53454=CARTESIAN_POINT('Ctrl Pts',(19.668779827001,0.975626090422456,127.667107634863));
#53455=CARTESIAN_POINT('Ctrl Pts',(19.1668970355953,1.36425684437746,127.70561854479));
#53456=CARTESIAN_POINT('Ctrl Pts',(18.5516662094274,1.51360466839347,127.744028818514));
#53457=CARTESIAN_POINT('Ctrl Pts',(17.9307733025901,1.39894337967582,127.782335107277));
#53458=CARTESIAN_POINT('Ctrl Pts',(17.4123242174242,1.04167741959983,127.820535082458));
#53459=CARTESIAN_POINT('Ctrl Pts',(17.0859506034826,0.505353855619343,127.858624432456));
#53460=CARTESIAN_POINT('Ctrl Pts',(17.0073468000548,-0.115660539147105,
127.896603287419));
#53461=CARTESIAN_POINT('Ctrl Pts',(17.1887082901287,-0.712804426518825,
127.934463445259));
#53462=CARTESIAN_POINT('Ctrl Pts',(17.5968242247701,-1.18228848738728,127.972211070178));
#53463=CARTESIAN_POINT('Ctrl Pts',(18.1594647751005,-1.44338028586681,128.009830189198));
#53464=CARTESIAN_POINT('Ctrl Pts',(18.7773792661455,-1.45169262750987,128.04733985285));
#53465=CARTESIAN_POINT('Ctrl Pts',(19.3431050379592,-1.20800514227934,128.08469883111));
#53466=CARTESIAN_POINT('Ctrl Pts',(19.7588133155117,-0.755575471850324,
128.121972631757));
#53467=CARTESIAN_POINT('Ctrl Pts',(19.951297760402,-0.175292515373662,128.159067356881));
#53468=CARTESIAN_POINT('Ctrl Pts',(19.9034340295258,0.329415031944361,128.189872819389));
#53469=CARTESIAN_POINT('Ctrl Pts',(19.7415614504299,0.695520735101091,128.214527494858));
#53470=CARTESIAN_POINT('Ctrl Pts',(19.565222236119,0.937848553101471,128.232911803911));
#53471=CARTESIAN_POINT('Ctrl Pts',(19.3448274084493,1.13736399322295,128.251234940316));
#53472=CARTESIAN_POINT('Ctrl Pts',(19.091755510318,1.28568634008855,128.269574561488));
#53473=CARTESIAN_POINT('Ctrl Pts',(18.8137135895315,1.37704884322017,128.28795209244));
#53474=CARTESIAN_POINT('Ctrl Pts',(18.6151599929778,1.39831377343028,128.300122981779));
#53475=CARTESIAN_POINT('Ctrl Pts',(18.5130392122771,1.39917328141053,128.306168212023));
#53476=CARTESIAN_POINT('Ctrl Pts',(18.5113516871238,1.39953897393561,113.105914026714));
#53477=CARTESIAN_POINT('Ctrl Pts',(18.3589863122547,1.39825657818145,113.114933579443));
#53478=CARTESIAN_POINT('Ctrl Pts',(18.1642992852404,1.36721421031762,113.127075590873));
#53479=CARTESIAN_POINT('Ctrl Pts',(17.8942839195588,1.26218430764902,113.145316932379));
#53480=CARTESIAN_POINT('Ctrl Pts',(17.6851880183204,1.13963755329772,113.16047473423));
#53481=CARTESIAN_POINT('Ctrl Pts',(17.4673934822047,0.942389681177235,113.178581302361));
#53482=CARTESIAN_POINT('Ctrl Pts',(17.2940773743872,0.70403936319175,113.196661733656));
#53483=CARTESIAN_POINT('Ctrl Pts',(17.1357187151386,0.345774791719098,113.220785229217));
#53484=CARTESIAN_POINT('Ctrl Pts',(17.0894823718046,-0.145861162010181,
113.250790855953));
#53485=CARTESIAN_POINT('Ctrl Pts',(17.2759930636586,-0.706633555871871,
113.286647905341));
#53486=CARTESIAN_POINT('Ctrl Pts',(17.6749864517915,-1.14012578485946,113.322389111944));
#53487=CARTESIAN_POINT('Ctrl Pts',(18.2137084295675,-1.37171410552075,113.357954662974));
#53488=CARTESIAN_POINT('Ctrl Pts',(18.7974084932161,-1.36336584604869,113.393386644682));
#53489=CARTESIAN_POINT('Ctrl Pts',(19.3247627673478,-1.11816214646004,113.428659966589));
#53490=CARTESIAN_POINT('Ctrl Pts',(19.7041885325999,-0.680967221982905,
113.463785874814));
#53491=CARTESIAN_POINT('Ctrl Pts',(19.8712822536032,-0.129268651081804,
113.498757168997));
#53492=CARTESIAN_POINT('Ctrl Pts',(19.7987670025229,0.440037112002971,113.533576759984));
#53493=CARTESIAN_POINT('Ctrl Pts',(19.5013596035167,0.927912782061419,113.568241981718));
#53494=CARTESIAN_POINT('Ctrl Pts',(19.0327193807973,1.25032157235679,113.602753439165));
#53495=CARTESIAN_POINT('Ctrl Pts',(18.4757666540105,1.35273464100996,113.63711018654));
#53496=CARTESIAN_POINT('Ctrl Pts',(17.9280414761478,1.21933376337218,113.67131219649));
#53497=CARTESIAN_POINT('Ctrl Pts',(17.4845929117289,0.875417320108831,113.705359156385));
#53498=CARTESIAN_POINT('Ctrl Pts',(17.2214967953587,0.382626263301629,113.739251050795));
#53499=CARTESIAN_POINT('Ctrl Pts',(17.1828026342533,-0.172095488110439,
113.772987868005));
#53500=CARTESIAN_POINT('Ctrl Pts',(17.3731808698039,-0.691842439720159,
113.806569762154));
#53501=CARTESIAN_POINT('Ctrl Pts',(17.7574604796447,-1.08667234074387,113.839996948255));
#53502=CARTESIAN_POINT('Ctrl Pts',(18.2671343378151,-1.28916901243406,113.873269790971));
#53503=CARTESIAN_POINT('Ctrl Pts',(18.8125146649335,-1.26594080045812,113.906388695895));
#53504=CARTESIAN_POINT('Ctrl Pts',(19.2985966148297,-1.02310331013343,113.93935427002));
#53505=CARTESIAN_POINT('Ctrl Pts',(19.6414920790201,-0.604858544715025,
113.972167107524));
#53506=CARTESIAN_POINT('Ctrl Pts',(19.7830009043026,-0.0854650173762428,
114.004828006579));
#53507=CARTESIAN_POINT('Ctrl Pts',(19.7004051738126,0.443986345750033,114.037337813179));
#53508=CARTESIAN_POINT('Ctrl Pts',(19.4101107233049,0.891426522117437,114.069697472386));
#53509=CARTESIAN_POINT('Ctrl Pts',(18.9644376547088,1.17997469370865,114.101908096569));
#53510=CARTESIAN_POINT('Ctrl Pts',(18.5292359593294,1.2473874871807,114.128626980292));
#53511=CARTESIAN_POINT('Ctrl Pts',(18.1884808231005,1.1915529185394,114.149928831447));
#53512=CARTESIAN_POINT('Ctrl Pts',(17.867350669578,1.06670828297356,114.171182018965));
#53513=CARTESIAN_POINT('Ctrl Pts',(17.5301291320079,0.789751537535966,114.197657653242));
#53514=CARTESIAN_POINT('Ctrl Pts',(17.2976207784108,0.323162814182794,114.229284668447));
#53515=CARTESIAN_POINT('Ctrl Pts',(17.2760307589781,-0.195322300576695,
114.260769422979));
#53516=CARTESIAN_POINT('Ctrl Pts',(17.4672530148769,-0.675270737380106,
114.292113588026));
#53517=CARTESIAN_POINT('Ctrl Pts',(17.8361784311516,-1.03365374413639,114.323318935717));
#53518=CARTESIAN_POINT('Ctrl Pts',(18.3171896252618,-1.20932699187921,114.354387290873));
#53519=CARTESIAN_POINT('Ctrl Pts',(18.8257788687749,-1.17336834058296,114.385320598929));
#53520=CARTESIAN_POINT('Ctrl Pts',(19.2733928879841,-0.933855304247329,
114.416120915472));
#53521=CARTESIAN_POINT('Ctrl Pts',(19.5828209898627,-0.534110071302645,
114.446790313512));
#53522=CARTESIAN_POINT('Ctrl Pts',(19.7014910385769,-0.0449140169986757,
114.477331070014));
#53523=CARTESIAN_POINT('Ctrl Pts',(19.6103829036543,0.448052163986159,114.507745421826));
#53524=CARTESIAN_POINT('Ctrl Pts',(19.3270409336854,0.859114585275451,114.538035790502));
#53525=CARTESIAN_POINT('Ctrl Pts',(18.902219003043,1.11756691087476,114.568204633005));
#53526=CARTESIAN_POINT('Ctrl Pts',(18.4108359765105,1.17971542272961,114.598254500916));
#53527=CARTESIAN_POINT('Ctrl Pts',(17.938757082736,1.03630336296344,114.628188026478));
#53528=CARTESIAN_POINT('Ctrl Pts',(17.5678384414828,0.713813950315308,114.658007922532));
#53529=CARTESIAN_POINT('Ctrl Pts',(17.3617553520377,0.269607479199184,114.687716968681));
#53530=CARTESIAN_POINT('Ctrl Pts',(17.3550963866736,-0.218243764897947,
114.717318043725));
#53531=CARTESIAN_POINT('Ctrl Pts',(17.5475950744081,-0.664690998735179,
114.7468140547));
#53532=CARTESIAN_POINT('Ctrl Pts',(17.9043991100135,-0.992416595278079,
114.776208065471));
#53533=CARTESIAN_POINT('Ctrl Pts',(18.3624169483923,-1.14535975384611,114.805503046249));
#53534=CARTESIAN_POINT('Ctrl Pts',(18.7615170178427,-1.10585452867801,114.829835796926));
#53535=CARTESIAN_POINT('Ctrl Pts',(19.0496294954737,-0.978997161595419,
114.849255587645));
#53536=CARTESIAN_POINT('Ctrl Pts',(19.3048574786947,-0.79553250362716,114.868645042624));
#53537=CARTESIAN_POINT('Ctrl Pts',(19.5399712571078,-0.473714416566306,
114.892826185557));
#53538=CARTESIAN_POINT('Ctrl Pts',(19.6393850634584,-0.00730971802335478,
114.921757393726));
#53539=CARTESIAN_POINT('Ctrl Pts',(19.5399625820036,0.457663098314685,114.950606072505));
#53540=CARTESIAN_POINT('Ctrl Pts',(19.2600489521841,0.8404401746431,114.979375535716));
#53541=CARTESIAN_POINT('Ctrl Pts',(18.8493002660062,1.0748791204869,115.008069367643));
#53542=CARTESIAN_POINT('Ctrl Pts',(18.3798045540622,1.12100379325741,115.03669105096));
#53543=CARTESIAN_POINT('Ctrl Pts',(17.9334761702293,0.971691728884436,115.065244271503));
#53544=CARTESIAN_POINT('Ctrl Pts',(17.5878676214356,0.65385534597262,115.093732542151));
#53545=CARTESIAN_POINT('Ctrl Pts',(17.4025647057155,0.223459828864383,115.122159793198));
#53546=CARTESIAN_POINT('Ctrl Pts',(17.4085502873789,-0.19209819495059,115.147377124544));
#53547=CARTESIAN_POINT('Ctrl Pts',(17.5367356176809,-0.527142367594399,
115.169408004386));
#53548=CARTESIAN_POINT('Ctrl Pts',(17.6750977312951,-0.711158333094599,
115.183552912859));
#53549=CARTESIAN_POINT('Ctrl Pts',(17.7863885808917,-0.814774883732063,
115.192976963383));
#53550=CARTESIAN_POINT('Ctrl Pts',(17.8454247819276,-0.862585781096137,
115.197687300119));
#53551=CARTESIAN_POINT('Ctrl Pts',(17.9077104618947,-0.906089824707936,
115.202396522212));
#53552=CARTESIAN_POINT('Ctrl Pts',(18.0379443370074,-0.984212744282978,
115.211811648537));
#53553=CARTESIAN_POINT('Ctrl Pts',(18.2526617065583,-1.06613325129506,115.225926301068));
#53554=CARTESIAN_POINT('Ctrl Pts',(18.5576019510004,-1.0918497608244,115.244724894711));
#53555=CARTESIAN_POINT('Ctrl Pts',(18.8575606192194,-1.03215987599148,115.263506537009));
#53556=CARTESIAN_POINT('Ctrl Pts',(19.1288588143958,-0.891952186562153,
115.28227013416));
#53557=CARTESIAN_POINT('Ctrl Pts',(19.3508251361679,-0.682207124521765,
115.301018799015));
#53558=CARTESIAN_POINT('Ctrl Pts',(19.5054574638842,-0.419560801893519,
115.319752073714));
#53559=CARTESIAN_POINT('Ctrl Pts',(19.6077308631518,-0.0259263154196786,
115.344712356295));
#53560=CARTESIAN_POINT('Ctrl Pts',(19.5377477746489,0.38586915460951,115.369647933046));
#53561=CARTESIAN_POINT('Ctrl Pts',(19.3396914214431,0.680822124532718,115.391448755122));
#53562=CARTESIAN_POINT('Ctrl Pts',(19.1956630207076,0.821138998095959,115.403902493605));
#53563=CARTESIAN_POINT('Ctrl Pts',(19.0330562168647,0.939881008679034,115.416353054312));
#53564=CARTESIAN_POINT('Ctrl Pts',(18.8713590570001,1.01232560464736,115.427243762488));
#53565=CARTESIAN_POINT('Ctrl Pts',(18.725228959151,1.04886022864609,115.436577314987));
#53566=CARTESIAN_POINT('Ctrl Pts',(18.6511396870949,1.06199516467199,115.441243483769));
#53567=CARTESIAN_POINT('Ctrl Pts',(18.5887552060792,1.06860250803456,115.445131759822));
#53568=CARTESIAN_POINT('Ctrl Pts',(18.5386687908435,1.07119204246765,115.448241987292));
#53569=CARTESIAN_POINT('Ctrl Pts',(18.335367217824,1.07507497226287,115.460855897531));
#53570=CARTESIAN_POINT('Ctrl Pts',(17.9664424762471,0.980875509761386,115.483744741735));
#53571=CARTESIAN_POINT('Ctrl Pts',(17.6520792257115,0.689325937350842,115.509534368755));
#53572=CARTESIAN_POINT('Ctrl Pts',(17.5121694936909,0.42613007298751,115.527953977153));
#53573=CARTESIAN_POINT('Ctrl Pts',(17.4645396133996,0.2850154477201,115.537163914722));
#53574=CARTESIAN_POINT('Ctrl Pts',(17.441120994326,0.168435469558622,115.544532136209));
#53575=CARTESIAN_POINT('Ctrl Pts',(17.4131560783799,-0.0676969984065009,
115.559267961778));
#53576=CARTESIAN_POINT('Ctrl Pts',(17.4823658039121,-0.459825862112777,
115.583215931233));
#53577=CARTESIAN_POINT('Ctrl Pts',(17.8262853295745,-0.891269399178329,
115.616384804494));
#53578=CARTESIAN_POINT('Ctrl Pts',(18.2924680185614,-1.08762744645822,115.64680542441));
#53579=CARTESIAN_POINT('Ctrl Pts',(18.7462270489574,-1.0703230621042,115.674477878059));
#53580=CARTESIAN_POINT('Ctrl Pts',(19.1209344877883,-0.907026557236116,
115.699399300559));
#53581=CARTESIAN_POINT('Ctrl Pts',(19.4103418070842,-0.617613192611829,
115.724339949641));
#53582=CARTESIAN_POINT('Ctrl Pts',(19.546765896882,-0.304888187420353,115.745141645372));
#53583=CARTESIAN_POINT('Ctrl Pts',(19.581845245331,-0.0374613907239736,
115.76179592779));
#53584=CARTESIAN_POINT('Ctrl Pts',(19.5705544130237,0.16452246986593,115.774292242788));
#53585=CARTESIAN_POINT('Ctrl Pts',(19.5299314232032,0.3283161944619,115.78471254347));
#53586=CARTESIAN_POINT('Ctrl Pts',(19.4795616558565,0.453109334487188,115.793051979174));
#53587=CARTESIAN_POINT('Ctrl Pts',(19.3869833795747,0.632584070260413,115.805564455334));
#53588=CARTESIAN_POINT('Ctrl Pts',(19.1860046219035,0.866177552115459,115.824348246596));
#53589=CARTESIAN_POINT('Ctrl Pts',(18.8222879048801,1.05846861458212,115.84942542723));
#53590=CARTESIAN_POINT('Ctrl Pts',(18.4128715286235,1.10465772425926,115.874538537355));
#53591=CARTESIAN_POINT('Ctrl Pts',(18.1139470962793,1.02460139690338,115.8934021608));
#53592=CARTESIAN_POINT('Ctrl Pts',(17.935263979171,0.927889961734541,115.905990634769));
#53593=CARTESIAN_POINT('Ctrl Pts',(17.8226045130323,0.852641962694081,115.91438613578));
#53594=CARTESIAN_POINT('Ctrl Pts',(17.6450265571346,0.694036087225085,115.929088683311));
#53595=CARTESIAN_POINT('Ctrl Pts',(17.5255867282254,0.504314599272793,115.942757778983));
#53596=CARTESIAN_POINT('Ctrl Pts',(17.4674220030132,0.344811226726132,115.953283647491));
#53597=CARTESIAN_POINT('Ctrl Pts',(17.4521496715754,0.296233089264299,115.956442243962));
#53598=CARTESIAN_POINT('Ctrl Pts',(17.439207974003,0.246949331300578,115.959601506988));
#53599=CARTESIAN_POINT('Ctrl Pts',(17.4285669872276,0.197121087776645,115.962761544684));
#53600=CARTESIAN_POINT('Ctrl Pts',(17.4202486700005,0.146830936758464,115.965922273101));
#53601=CARTESIAN_POINT('Ctrl Pts',(17.412357915538,0.0793192050127272,115.970137566166));
#53602=CARTESIAN_POINT('Ctrl Pts',(17.4034732364542,-0.107616603328217,
115.981733364604));
#53603=CARTESIAN_POINT('Ctrl Pts',(17.461377849773,-0.41387644231022,116.000732291017));
#53604=CARTESIAN_POINT('Ctrl Pts',(17.6828616627857,-0.766524560243698,
116.026114794632));
#53605=CARTESIAN_POINT('Ctrl Pts',(18.0185767554592,-1.01440331549217,116.051551886574));
#53606=CARTESIAN_POINT('Ctrl Pts',(18.4225665632467,-1.12273838760728,116.077045286512));
#53607=CARTESIAN_POINT('Ctrl Pts',(18.83912791779,-1.07589746406352,116.102598001197));
#53608=CARTESIAN_POINT('Ctrl Pts',(19.2107527297005,-0.8796214031171,116.128212039234));
#53609=CARTESIAN_POINT('Ctrl Pts',(19.424451551719,-0.631313603440492,116.148184292881));
#53610=CARTESIAN_POINT('Ctrl Pts',(19.5271584694527,-0.424547170861779,
116.162474157721));
#53611=CARTESIAN_POINT('Ctrl Pts',(19.5880911897583,-0.250123727488174,
116.173916708735));
#53612=CARTESIAN_POINT('Ctrl Pts',(19.6371899862326,0.072010671089548,116.193966675555));
#53613=CARTESIAN_POINT('Ctrl Pts',(19.5312491458833,0.537649088107642,116.22268737364));
#53614=CARTESIAN_POINT('Ctrl Pts',(19.1506475461343,0.969263331407848,116.257281026004));
#53615=CARTESIAN_POINT('Ctrl Pts',(18.6080789065826,1.16704974088591,116.292009350826));
#53616=CARTESIAN_POINT('Ctrl Pts',(18.0345517634555,1.08093962226307,116.326877318219));
#53617=CARTESIAN_POINT('Ctrl Pts',(17.6379610394385,0.780764466937685,116.356784161276));
#53618=CARTESIAN_POINT('Ctrl Pts',(17.4326718707591,0.431520171549925,116.381667699098));
#53619=CARTESIAN_POINT('Ctrl Pts',(17.3243036095994,0.0153408501438764,
116.408079506778));
#53620=CARTESIAN_POINT('Ctrl Pts',(17.4168359598342,-0.532483913432153,
116.441216842383));
#53621=CARTESIAN_POINT('Ctrl Pts',(17.8631699482747,-1.03264209362388,116.481184742038));
#53622=CARTESIAN_POINT('Ctrl Pts',(18.5104604520464,-1.21960339016096,116.521361981733));
#53623=CARTESIAN_POINT('Ctrl Pts',(19.1614492145997,-1.03262237061467,116.561754669311));
#53624=CARTESIAN_POINT('Ctrl Pts',(19.6158431880161,-0.525056657258863,
116.602368748702));
#53625=CARTESIAN_POINT('Ctrl Pts',(19.711601838574,0.0374389790684584,116.636402738718));
#53626=CARTESIAN_POINT('Ctrl Pts',(19.5996504879164,0.468431902550626,116.66374624569));
#53627=CARTESIAN_POINT('Ctrl Pts',(19.4300177437899,0.75701849348732,116.684312306879));
#53628=CARTESIAN_POINT('Ctrl Pts',(19.185748019025,0.98745395999935,116.704937967889));
#53629=CARTESIAN_POINT('Ctrl Pts',(18.7872001223434,1.19443636121172,116.732518393314));
#53630=CARTESIAN_POINT('Ctrl Pts',(18.2076140535373,1.22767049755924,116.767145372071));
#53631=CARTESIAN_POINT('Ctrl Pts',(17.5937432616692,0.889007641910738,116.808944015097));
#53632=CARTESIAN_POINT('Ctrl Pts',(17.2521681574792,0.272180427293588,116.850993272138));
#53633=CARTESIAN_POINT('Ctrl Pts',(17.2913162457654,-0.436194779844278,
116.893296892387));
#53634=CARTESIAN_POINT('Ctrl Pts',(17.7038571015148,-1.01864243864716,116.935858467641));
#53635=CARTESIAN_POINT('Ctrl Pts',(18.3670800933445,-1.29404223866986,116.978681197049));
#53636=CARTESIAN_POINT('Ctrl Pts',(19.0795409122072,-1.17362287387417,117.021768008785));
#53637=CARTESIAN_POINT('Ctrl Pts',(19.6220674999244,-0.689641540177797,
117.065121491555));
#53638=CARTESIAN_POINT('Ctrl Pts',(19.8251990236932,0.0131357064283045,
117.108743921761));
#53639=CARTESIAN_POINT('Ctrl Pts',(19.6220412864902,0.720631070474546,117.152637244666));
#53640=CARTESIAN_POINT('Ctrl Pts',(19.0702069383145,1.21464681696053,117.196803085261));
#53641=CARTESIAN_POINT('Ctrl Pts',(18.3355975639786,1.34012022714546,117.241242736065));
#53642=CARTESIAN_POINT('Ctrl Pts',(17.6425703116435,1.05376306472665,117.285957159459));
#53643=CARTESIAN_POINT('Ctrl Pts',(17.2054487318153,0.438821315496588,117.330946987677));
#53644=CARTESIAN_POINT('Ctrl Pts',(17.1622294713761,-0.319048897988897,
117.376212520113));
#53645=CARTESIAN_POINT('Ctrl Pts',(17.531095775153,-0.98778618784794,117.421753723563));
#53646=CARTESIAN_POINT('Ctrl Pts',(18.2032302806575,-1.36002403472624,117.467570232336));
#53647=CARTESIAN_POINT('Ctrl Pts',(18.9750292819446,-1.31731515605936,117.513661349979));
#53648=CARTESIAN_POINT('Ctrl Pts',(19.6094611826802,-0.867937834405175,
117.560026043846));
#53649=CARTESIAN_POINT('Ctrl Pts',(19.9094757960212,-0.145559704600647,
117.60666296168));
#53650=CARTESIAN_POINT('Ctrl Pts',(19.7999774806316,0.500689885182389,117.645752497943));
#53651=CARTESIAN_POINT('Ctrl Pts',(19.5150122013445,0.925278807945587,117.677158402211));
#53652=CARTESIAN_POINT('Ctrl Pts',(19.1240773404713,1.25704056473757,117.708653378912));
#53653=CARTESIAN_POINT('Ctrl Pts',(18.4872767009066,1.44128037713583,117.748188539166));
#53654=CARTESIAN_POINT('Ctrl Pts',(17.7182695158132,1.22028704524381,117.795894191709));
#53655=CARTESIAN_POINT('Ctrl Pts',(17.1818536479469,0.6209694352788,117.84386042374));
#53656=CARTESIAN_POINT('Ctrl Pts',(17.0457729949993,-0.176241227277537,
117.892083891781));
#53657=CARTESIAN_POINT('Ctrl Pts',(17.356339229752,-0.927521629412933,117.940561028213));
#53658=CARTESIAN_POINT('Ctrl Pts',(18.0224285226418,-1.40087677191055,117.989287906266));
#53659=CARTESIAN_POINT('Ctrl Pts',(18.8423662647727,-1.44747689273984,118.038260331711));
#53660=CARTESIAN_POINT('Ctrl Pts',(19.564973581273,-1.04879126733954,118.087473779158));
#53661=CARTESIAN_POINT('Ctrl Pts',(19.9665731208934,-0.323199709536255,
118.136923494836));
#53662=CARTESIAN_POINT('Ctrl Pts',(19.9204307603646,0.508545196077463,118.186604326532));
#53663=CARTESIAN_POINT('Ctrl Pts',(19.4364850154724,1.19163922937571,118.236511041213));
#53664=CARTESIAN_POINT('Ctrl Pts',(18.7896014129428,1.45977975239074,118.278283324362));
#53665=CARTESIAN_POINT('Ctrl Pts',(18.2437658807907,1.44350219297019,118.311808461719));
#53666=CARTESIAN_POINT('Ctrl Pts',(17.8529857116712,1.31941501771739,118.337004909982));
#53667=CARTESIAN_POINT('Ctrl Pts',(17.5111199319821,1.09085297848017,118.362253631037));
#53668=CARTESIAN_POINT('Ctrl Pts',(17.2453545367621,0.776316639682611,118.387553332054));
#53669=CARTESIAN_POINT('Ctrl Pts',(17.0767100831229,0.399529811958646,118.412903698764));
#53670=CARTESIAN_POINT('Ctrl Pts',(17.0188671438186,-0.00986043940601462,
118.438303460264));
#53671=CARTESIAN_POINT('Ctrl Pts',(17.0766989112945,-0.420209281010889,
118.463752185059));
#53672=CARTESIAN_POINT('Ctrl Pts',(17.2180009588825,-0.735846803400231,
118.484999124376));
#53673=CARTESIAN_POINT('Ctrl Pts',(17.3803055651797,-0.958070010311263,
118.502020602052));
#53674=CARTESIAN_POINT('Ctrl Pts',(17.5723108800011,-1.15519143488245,118.519057008924));
#53675=CARTESIAN_POINT('Ctrl Pts',(17.976044057097,-1.42626434895589,118.548911965511));
#53676=CARTESIAN_POINT('Ctrl Pts',(18.6825732967982,-1.5469332305085,118.591674536592));
#53677=CARTESIAN_POINT('Ctrl Pts',(19.480862487031,-1.21670551212833,118.643163512056));
#53678=CARTESIAN_POINT('Ctrl Pts',(19.898397453744,-0.628314262383973,118.686209676539));
#53679=CARTESIAN_POINT('Ctrl Pts',(19.9934589586098,-0.145556018009749,
118.716410875295));
#53680=CARTESIAN_POINT('Ctrl Pts',(19.9897381597335,0.133405879333075,118.733688581356));
#53681=CARTESIAN_POINT('Ctrl Pts',(19.9468629952409,0.409779100114465,118.75097829491));
#53682=CARTESIAN_POINT('Ctrl Pts',(19.8210589677851,0.738453944597032,118.772614532919));
#53683=CARTESIAN_POINT('Ctrl Pts',(19.482458213577,1.19036691859332,118.807280917743));
#53684=CARTESIAN_POINT('Ctrl Pts',(18.8455916039526,1.54286230442063,118.850703191666));
#53685=CARTESIAN_POINT('Ctrl Pts',(17.9707351056379,1.49403227262935,118.902943815855));
#53686=CARTESIAN_POINT('Ctrl Pts',(17.2543258704413,0.986046184208814,118.955310331053));
#53687=CARTESIAN_POINT('Ctrl Pts',(16.9736545538739,0.308628892705175,118.999046375777));
#53688=CARTESIAN_POINT('Ctrl Pts',(16.9908076007375,-0.261884195942545,
119.034089856028));
#53689=CARTESIAN_POINT('Ctrl Pts',(17.0986304843311,-0.60187232667865,119.056013023723));
#53690=CARTESIAN_POINT('Ctrl Pts',(17.2220725601196,-0.817412115664082,
119.071370791807));
#53691=CARTESIAN_POINT('Ctrl Pts',(17.3046947454948,-0.932313588781289,
119.080149511234));
#53692=CARTESIAN_POINT('Ctrl Pts',(17.3953791605744,-1.041187868381,119.088930231404));
#53693=CARTESIAN_POINT('Ctrl Pts',(17.522559367852,-1.16486266553002,119.099909408076));
#53694=CARTESIAN_POINT('Ctrl Pts',(17.7518728090185,-1.33251390437618,119.117484980784));
#53695=CARTESIAN_POINT('Ctrl Pts',(18.0785092162954,-1.47873509889951,119.139467629877));
#53696=CARTESIAN_POINT('Ctrl Pts',(18.5041370739365,-1.5388357928971,119.165868977217));
#53697=CARTESIAN_POINT('Ctrl Pts',(18.9300650017773,-1.47872940044093,119.192290133091));
#53698=CARTESIAN_POINT('Ctrl Pts',(19.3230070662878,-1.30292433215567,119.218730941718));
#53699=CARTESIAN_POINT('Ctrl Pts',(19.6521414527707,-1.02501935198784,119.245189343596));
#53700=CARTESIAN_POINT('Ctrl Pts',(19.8916273980147,-0.666633644247205,
119.271665261632));
#53701=CARTESIAN_POINT('Ctrl Pts',(20.022628534436,-0.255704738726529,119.298156046695));
#53702=CARTESIAN_POINT('Ctrl Pts',(20.0347268900414,0.175649279097044,119.324662499476));
#53703=CARTESIAN_POINT('Ctrl Pts',(19.944906803099,0.524066451041732,119.346761205289));
#53704=CARTESIAN_POINT('Ctrl Pts',(19.817156023757,0.779729444103676,119.364447186537));
#53705=CARTESIAN_POINT('Ctrl Pts',(19.6147295341782,1.07423777764439,119.386558876142));
#53706=CARTESIAN_POINT('Ctrl Pts',(19.2202188753249,1.39809308905388,119.417528285369));
#53707=CARTESIAN_POINT('Ctrl Pts',(18.5867241883604,1.57103813761991,119.457366923459));
#53708=CARTESIAN_POINT('Ctrl Pts',(17.9376186369372,1.47011788769029,119.4972223696));
#53709=CARTESIAN_POINT('Ctrl Pts',(17.3861508706095,1.11275405579027,119.537090587226));
#53710=CARTESIAN_POINT('Ctrl Pts',(17.028676399318,0.561178042742845,119.576967614436));
#53711=CARTESIAN_POINT('Ctrl Pts',(16.9276717633489,-0.0883484362600774,
119.616849261155));
#53712=CARTESIAN_POINT('Ctrl Pts',(17.1007536383431,-0.722549055594297,
119.656731792094));
#53713=CARTESIAN_POINT('Ctrl Pts',(17.448299666744,-1.14590146394558,119.689964100819));
#53714=CARTESIAN_POINT('Ctrl Pts',(17.8117792744431,-1.37737020083668,119.716546697506));
#53715=CARTESIAN_POINT('Ctrl Pts',(18.215243549761,-1.52858309297296,119.743125722118));
#53716=CARTESIAN_POINT('Ctrl Pts',(18.762237993062,-1.55167189010214,119.776342653443));
#53717=CARTESIAN_POINT('Ctrl Pts',(19.3724575824767,-1.30880681937892,119.816187384569));
#53718=CARTESIAN_POINT('Ctrl Pts',(19.8300303495297,-0.838178157233193,
119.856012717496));
#53719=CARTESIAN_POINT('Ctrl Pts',(20.0553319706966,-0.222028446015196,
119.895814549444));
#53720=CARTESIAN_POINT('Ctrl Pts',(20.0093412860961,0.431937143886497,119.935588953089));
#53721=CARTESIAN_POINT('Ctrl Pts',(19.7004996494563,1.0096265526074,119.975331924619));
#53722=CARTESIAN_POINT('Ctrl Pts',(19.1830809519466,1.41042933555735,120.015039549248));
#53723=CARTESIAN_POINT('Ctrl Pts',(18.5477417148256,1.56476304383288,120.054707867703));
#53724=CARTESIAN_POINT('Ctrl Pts',(17.9054220875877,1.44629301140049,120.094333047644));
#53725=CARTESIAN_POINT('Ctrl Pts',(17.457794562179,1.13785264331078,120.127314767186));
#53726=CARTESIAN_POINT('Ctrl Pts',(17.1987941750473,0.797975612371571,120.15367472761));
#53727=CARTESIAN_POINT('Ctrl Pts',(17.0158521800977,0.412114272847593,120.180017209918));
#53728=CARTESIAN_POINT('Ctrl Pts',(16.947623315073,-0.125744883561413,120.212910946089));
#53729=CARTESIAN_POINT('Ctrl Pts',(17.136323471403,-0.747393162690755,120.252325078772));
#53730=CARTESIAN_POINT('Ctrl Pts',(17.5617842077802,-1.23696498855081,120.291677025785));
#53731=CARTESIAN_POINT('Ctrl Pts',(18.1491297132522,-1.50960991539734,120.330963166602));
#53732=CARTESIAN_POINT('Ctrl Pts',(18.7954584704689,-1.51854825462399,120.370179815259));
#53733=CARTESIAN_POINT('Ctrl Pts',(19.3879619651131,-1.26319238361003,120.409323412335));
#53734=CARTESIAN_POINT('Ctrl Pts',(19.8236300342295,-0.789026463960243,
120.448390403264));
#53735=CARTESIAN_POINT('Ctrl Pts',(20.0272069290065,-0.179520794684316,
120.487377310988));
#53736=CARTESIAN_POINT('Ctrl Pts',(19.9642079867834,0.458605653018268,120.526280699406));
#53737=CARTESIAN_POINT('Ctrl Pts',(19.6467700311826,1.01409833734176,120.565097195004));
#53738=CARTESIAN_POINT('Ctrl Pts',(19.1313271507666,1.39060526020685,120.603823479438));
#53739=CARTESIAN_POINT('Ctrl Pts',(18.5085629232136,1.52341751453039,120.642456297882));
#53740=CARTESIAN_POINT('Ctrl Pts',(17.8874269014854,1.39060921920092,120.680992458869));
#53741=CARTESIAN_POINT('Ctrl Pts',(17.376040183818,1.01665067198976,120.71942883698));
#53742=CARTESIAN_POINT('Ctrl Pts',(17.0628414097054,0.467903960283591,120.757762373191));
#53743=CARTESIAN_POINT('Ctrl Pts',(17.0012673452733,-0.159171624986709,
120.795990078213));
#53744=CARTESIAN_POINT('Ctrl Pts',(17.2006255114261,-0.755003713793607,
120.834109034869));
#53745=CARTESIAN_POINT('Ctrl Pts',(17.6247193648195,-1.21608511592836,120.87211640052));
#53746=CARTESIAN_POINT('Ctrl Pts',(18.1984219080174,-1.46298378556885,120.910009408484));
#53747=CARTESIAN_POINT('Ctrl Pts',(18.8210031809677,-1.45404564397339,120.947785368188));
#53748=CARTESIAN_POINT('Ctrl Pts',(19.3838435340945,-1.19242410821281,120.985441669183));
#53749=CARTESIAN_POINT('Ctrl Pts',(19.7894128883475,-0.725248797040647,
121.022975781176));
#53750=CARTESIAN_POINT('Ctrl Pts',(19.968194413284,-0.135131499300795,121.060385259496));
#53751=CARTESIAN_POINT('Ctrl Pts',(19.8906126551429,0.474463548421036,121.097667740759));
#53752=CARTESIAN_POINT('Ctrl Pts',(19.5719166839362,0.997380748400016,121.134820952923));
#53753=CARTESIAN_POINT('Ctrl Pts',(19.0692161746709,1.34329155662882,121.171842700173));
#53754=CARTESIAN_POINT('Ctrl Pts',(18.4712387268708,1.45330105771547,121.208730897588));
#53755=CARTESIAN_POINT('Ctrl Pts',(17.8826539013599,1.31000788465432,121.245483511077));
#53756=CARTESIAN_POINT('Ctrl Pts',(17.4057248129287,0.940178434972456,121.282098674275));
#53757=CARTESIAN_POINT('Ctrl Pts',(17.1225303971144,0.409857233817631,121.318574471326));
#53758=CARTESIAN_POINT('Ctrl Pts',(17.0808109556991,-0.18761576406713,121.354909351532));
#53759=CARTESIAN_POINT('Ctrl Pts',(17.234662884993,-0.60767734320799,121.382053320561));
#53760=CARTESIAN_POINT('Ctrl Pts',(17.4026562098279,-0.845818839371914,
121.400104492057));
#53761=CARTESIAN_POINT('Ctrl Pts',(17.5304295290375,-0.991852754127738,
121.412126298005));
#53762=CARTESIAN_POINT('Ctrl Pts',(17.7920501977231,-1.20994146748006,121.433133107686));
#53763=CARTESIAN_POINT('Ctrl Pts',(18.2502296129569,-1.39212149316642,121.463051648494));
#53764=CARTESIAN_POINT('Ctrl Pts',(18.8390918948479,-1.36703543517734,121.498806978423));
#53765=CARTESIAN_POINT('Ctrl Pts',(19.3641003985679,-1.10478925936658,121.534414063249));
#53766=CARTESIAN_POINT('Ctrl Pts',(19.7346755496411,-0.652838433166381,
121.569871802645));
#53767=CARTESIAN_POINT('Ctrl Pts',(19.8876619889454,-0.0913592885263403,
121.605179139474));
#53768=CARTESIAN_POINT('Ctrl Pts',(19.7983634546371,0.481182887673296,121.640335149));
#53769=CARTESIAN_POINT('Ctrl Pts',(19.4843596671287,0.96520447245087,121.675338992639));
#53770=CARTESIAN_POINT('Ctrl Pts',(19.0021632434605,1.27739010659383,121.710189943609));
#53771=CARTESIAN_POINT('Ctrl Pts',(18.4370107635688,1.3650059559128,121.744887374439));
#53772=CARTESIAN_POINT('Ctrl Pts',(17.8878131855026,1.21481569708191,121.779430764563));
#53773=CARTESIAN_POINT('Ctrl Pts',(17.4498271981239,0.855022050904291,121.813819696406));
#53774=CARTESIAN_POINT('Ctrl Pts',(17.19813616434,0.349998239521284,121.848053857948));
#53775=CARTESIAN_POINT('Ctrl Pts',(17.1747784662698,-0.211228605711279,
121.882133041112));
#53776=CARTESIAN_POINT('Ctrl Pts',(17.3817429545998,-0.73067256982998,121.916057144785));
#53777=CARTESIAN_POINT('Ctrl Pts',(17.780987988533,-1.11849653673519,121.949826170361));
#53778=CARTESIAN_POINT('Ctrl Pts',(18.3014175564027,-1.30855030916415,121.983440229557));
#53779=CARTESIAN_POINT('Ctrl Pts',(18.8515390403575,-1.26963899436222,122.016899529174));
#53780=CARTESIAN_POINT('Ctrl Pts',(19.3355425449402,-1.01063164342207,122.050204399541));
#53781=CARTESIAN_POINT('Ctrl Pts',(19.6699894411733,-0.578525953406879,
122.083355241515));
#53782=CARTESIAN_POINT('Ctrl Pts',(19.7981784976235,-0.049975975244043,
122.116352625486));
#53783=CARTESIAN_POINT('Ctrl Pts',(19.6997563641334,0.482371917081139,122.149197120449));
#53784=CARTESIAN_POINT('Ctrl Pts',(19.3939165927788,0.926015911083455,122.181889518331));
#53785=CARTESIAN_POINT('Ctrl Pts',(18.9356726261446,1.20475735757232,122.214430632586));
#53786=CARTESIAN_POINT('Ctrl Pts',(18.4060062045841,1.27170816166094,122.246821402389));
#53787=CARTESIAN_POINT('Ctrl Pts',(17.8975424573268,1.11719794305827,122.279062885459));
#53788=CARTESIAN_POINT('Ctrl Pts',(17.4983771377944,0.770086744703878,122.311156214457));
#53789=CARTESIAN_POINT('Ctrl Pts',(17.2768186093101,0.292410270944587,122.343102633485));
#53790=CARTESIAN_POINT('Ctrl Pts',(17.269719437291,-0.231700508547156,122.374903504129));
#53791=CARTESIAN_POINT('Ctrl Pts',(17.4763670890499,-0.710818699113158,
122.406560242296));
#53792=CARTESIAN_POINT('Ctrl Pts',(17.8589529235959,-1.06215785962516,122.438074418514));
#53793=CARTESIAN_POINT('Ctrl Pts',(18.3494690676881,-1.2258552099751,122.469447653676));
#53794=CARTESIAN_POINT('Ctrl Pts',(18.8617822651652,-1.17515551048656,122.500681677063));
#53795=CARTESIAN_POINT('Ctrl Pts',(19.306740267383,-0.92075115531246,122.531778343629));
#53796=CARTESIAN_POINT('Ctrl Pts',(19.6076666503762,-0.508600801661367,
122.562739531444));
#53797=CARTESIAN_POINT('Ctrl Pts',(19.7135494146674,-0.0116339705090276,
122.593567307384));
#53798=CARTESIAN_POINT('Ctrl Pts',(19.6076731364699,0.483114779154934,122.624263713906));
#53799=CARTESIAN_POINT('Ctrl Pts',(19.3102051188471,0.889762136113708,122.654831033973));
#53800=CARTESIAN_POINT('Ctrl Pts',(18.8744209204798,1.13840436181491,122.685271410186));
#53801=CARTESIAN_POINT('Ctrl Pts',(18.3771167267049,1.1871652605314,122.71558735378));
#53802=CARTESIAN_POINT('Ctrl Pts',(17.9051830307953,1.029208997682,122.745781222973));
#53803=CARTESIAN_POINT('Ctrl Pts',(17.5403703562541,0.693576750726723,122.77585559056));
#53804=CARTESIAN_POINT('Ctrl Pts',(17.3452208922813,0.240041357799779,122.805813070685));
#53805=CARTESIAN_POINT('Ctrl Pts',(17.3515208693343,-0.197222450308024,
122.832340402984));
#53806=CARTESIAN_POINT('Ctrl Pts',(17.4863244070343,-0.548895301526989,
122.85547963802));
#53807=CARTESIAN_POINT('Ctrl Pts',(17.7440611200262,-0.892625678754596,
122.881859502068));
#53808=CARTESIAN_POINT('Ctrl Pts',(18.2262426351603,-1.15890748220768,122.914714845542));
#53809=CARTESIAN_POINT('Ctrl Pts',(18.8833930837132,-1.12154607814807,122.953956867101));
#53810=CARTESIAN_POINT('Ctrl Pts',(19.417378773027,-0.742108947509844,122.993021846801));
#53811=CARTESIAN_POINT('Ctrl Pts',(19.6666571462621,-0.139392568668771,
123.031917160417));
#53812=CARTESIAN_POINT('Ctrl Pts',(19.557479197789,0.501041105718899,123.070650511539));
#53813=CARTESIAN_POINT('Ctrl Pts',(19.1979910414516,0.902623177622933,123.102799827228));
#53814=CARTESIAN_POINT('Ctrl Pts',(18.8164093817205,1.07240048839272,123.128446232696));
#53815=CARTESIAN_POINT('Ctrl Pts',(18.5184865862346,1.11482117402686,123.146934468807));
#53816=CARTESIAN_POINT('Ctrl Pts',(18.2324054828255,1.07857876720517,123.164681440727));
#53817=CARTESIAN_POINT('Ctrl Pts',(17.8891655916273,0.944438997380313,123.187362255959));
#53818=CARTESIAN_POINT('Ctrl Pts',(17.5443717314018,0.624378993516739,123.21564875382));
#53819=CARTESIAN_POINT('Ctrl Pts',(17.3952088655578,0.179660540296838,123.243854556847));
#53820=CARTESIAN_POINT('Ctrl Pts',(17.4140954128167,-0.185732646246057,
123.266373423675));
#53821=CARTESIAN_POINT('Ctrl Pts',(17.5212227395653,-0.535021075635455,
123.288863256363));
#53822=CARTESIAN_POINT('Ctrl Pts',(17.812244787014,-0.899924705335984,123.316922183842));
#53823=CARTESIAN_POINT('Ctrl Pts',(18.2842319058948,-1.09849765273693,123.347715096373));
#53824=CARTESIAN_POINT('Ctrl Pts',(18.7423557254701,-1.08094335039291,123.375655800996));
#53825=CARTESIAN_POINT('Ctrl Pts',(19.1198741467514,-0.916334604468255,
123.4007644734));
#53826=CARTESIAN_POINT('Ctrl Pts',(19.4107202134498,-0.625331903211328,
123.425837870652));
#53827=CARTESIAN_POINT('Ctrl Pts',(19.5749506858235,-0.248827358969858,
123.450878596324));
#53828=CARTESIAN_POINT('Ctrl Pts',(19.5902582672216,0.161256534828828,123.47588966774));
#53829=CARTESIAN_POINT('Ctrl Pts',(19.4548322547901,0.548086758583229,123.500873384082));
#53830=CARTESIAN_POINT('Ctrl Pts',(19.2322452136596,0.806774003836304,123.521673295525));
#53831=CARTESIAN_POINT('Ctrl Pts',(19.0068132440525,0.953991375109464,123.538302073525));
#53832=CARTESIAN_POINT('Ctrl Pts',(18.7169314442061,1.07461791635357,123.557694757307));
#53833=CARTESIAN_POINT('Ctrl Pts',(18.2799908654444,1.09642297116301,123.583995307696));
#53834=CARTESIAN_POINT('Ctrl Pts',(17.8656644604746,0.896711667502387,123.611657850074));
#53835=CARTESIAN_POINT('Ctrl Pts',(17.6214240384758,0.632872186368461,123.633778060455));
#53836=CARTESIAN_POINT('Ctrl Pts',(17.4927046928802,0.396360692377051,123.650363822077));
#53837=CARTESIAN_POINT('Ctrl Pts',(17.4034992587404,0.0481367539224208,
123.672474132222));
#53838=CARTESIAN_POINT('Ctrl Pts',(17.4549679685944,-0.361979267228126,
123.697342438129));
#53839=CARTESIAN_POINT('Ctrl Pts',(17.6965579170255,-0.745759415090237,
123.724971781578));
#53840=CARTESIAN_POINT('Ctrl Pts',(18.0382603256698,-0.998195883246386,
123.750875322465));
#53841=CARTESIAN_POINT('Ctrl Pts',(18.4698637772213,-1.10315324998456,123.777819593015));
#53842=CARTESIAN_POINT('Ctrl Pts',(18.9235437736981,-1.01950381091171,123.80580909134));
#53843=CARTESIAN_POINT('Ctrl Pts',(19.2719865687262,-0.779544885220034,
123.831478142263));
#53844=CARTESIAN_POINT('Ctrl Pts',(19.4438761068751,-0.527684719547219,
123.8501564127));
#53845=CARTESIAN_POINT('Ctrl Pts',(19.5392742119118,-0.295150402427171,
123.865727180495));
#53846=CARTESIAN_POINT('Ctrl Pts',(19.586310736526,-0.0588575645688193,
123.880524776365));
#53847=CARTESIAN_POINT('Ctrl Pts',(19.5607154879257,0.244538156461791,123.899226477669));
#53848=CARTESIAN_POINT('Ctrl Pts',(19.4520859293862,0.529189150664088,123.91794037051));
#53849=CARTESIAN_POINT('Ctrl Pts',(19.2687581561598,0.772802794422214,123.936666822134));
#53850=CARTESIAN_POINT('Ctrl Pts',(19.0249947092009,0.956277148756344,123.955407545818));
#53851=CARTESIAN_POINT('Ctrl Pts',(18.7634668055328,1.05614295662185,123.972600525356));
#53852=CARTESIAN_POINT('Ctrl Pts',(18.511720320822,1.08618824432886,123.988242368963));
#53853=CARTESIAN_POINT('Ctrl Pts',(18.2084450486932,1.05870460262302,124.007025488382));
#53854=CARTESIAN_POINT('Ctrl Pts',(17.8526151266173,0.905597689373487,124.030530147954));
#53855=CARTESIAN_POINT('Ctrl Pts',(17.5374400251935,0.562785005443856,124.058780242183));
#53856=CARTESIAN_POINT('Ctrl Pts',(17.3894936022145,0.120463896426673,124.087079007616));
#53857=CARTESIAN_POINT('Ctrl Pts',(17.4352024530028,-0.344609559390143,
124.115430101927));
#53858=CARTESIAN_POINT('Ctrl Pts',(17.6673292304641,-0.751235919597019,
124.1438373954));
#53859=CARTESIAN_POINT('Ctrl Pts',(18.0460913057333,-1.02818689353757,124.172304589377));
#53860=CARTESIAN_POINT('Ctrl Pts',(18.5059607229931,-1.12649870064859,124.200835414131));
#53861=CARTESIAN_POINT('Ctrl Pts',(18.9669634259195,-1.02818302776601,124.229433518268));
#53862=CARTESIAN_POINT('Ctrl Pts',(19.3485491824866,-0.749461895391517,
124.25810252464));
#53863=CARTESIAN_POINT('Ctrl Pts',(19.5836265981341,-0.338131649402405,
124.286845998617));
#53864=CARTESIAN_POINT('Ctrl Pts',(19.630327822603,0.134618946327238,124.315667460856));
#53865=CARTESIAN_POINT('Ctrl Pts',(19.479443753127,0.58648760418091,124.344570375802));
#53866=CARTESIAN_POINT('Ctrl Pts',(19.1562137849851,0.938351901614487,124.373558153265));
#53867=CARTESIAN_POINT('Ctrl Pts',(18.7161248921632,1.12808670585089,124.40263414441));
#53868=CARTESIAN_POINT('Ctrl Pts',(18.2354148456271,1.12150629368483,124.431801642351));
#53869=CARTESIAN_POINT('Ctrl Pts',(17.7978998529863,0.918503883878429,124.461063877912));
#53870=CARTESIAN_POINT('Ctrl Pts',(17.4803961934958,0.553291510869809,124.490424017647));
#53871=CARTESIAN_POINT('Ctrl Pts',(17.3392647593072,0.0886576147994413,
124.519885160673));
#53872=CARTESIAN_POINT('Ctrl Pts',(17.4004301179553,-0.394798461775283,
124.549450337333));
#53873=CARTESIAN_POINT('Ctrl Pts',(17.6546385235008,-0.812615333546038,
124.579122508661));
#53874=CARTESIAN_POINT('Ctrl Pts',(18.0588194470523,-1.09119301111203,124.608904563076));
#53875=CARTESIAN_POINT('Ctrl Pts',(18.543358419133,-1.1807302345264,124.638799314424));
#53876=CARTESIAN_POINT('Ctrl Pts',(19.0240583854348,-1.06410629338754,124.668809499231));
#53877=CARTESIAN_POINT('Ctrl Pts',(19.4167402982424,-0.76012623588515,124.698937775415));
#53878=CARTESIAN_POINT('Ctrl Pts',(19.6519563673511,-0.32051767699258,124.729186721845));
#53879=CARTESIAN_POINT('Ctrl Pts',(19.6872486278557,0.178847159515111,124.759558835612));
#53880=CARTESIAN_POINT('Ctrl Pts',(19.5147929916102,0.651019381077076,124.790056530126));
#53881=CARTESIAN_POINT('Ctrl Pts',(19.1630554166896,1.01308604539074,124.820682132959));
#53882=CARTESIAN_POINT('Ctrl Pts',(18.6921194093106,1.2007058017599,124.851437884561));
#53883=CARTESIAN_POINT('Ctrl Pts',(18.1834458222145,1.17952283900347,124.882325937953));
#53884=CARTESIAN_POINT('Ctrl Pts',(17.7258058475007,0.951436951498519,124.913348356572));
#53885=CARTESIAN_POINT('Ctrl Pts',(17.3998118739641,0.554588535229773,124.944507112499));
#53886=CARTESIAN_POINT('Ctrl Pts',(17.26373753905,0.0570046141073459,124.975804084871));
#53887=CARTESIAN_POINT('Ctrl Pts',(17.3431180960944,-0.455041055169738,
125.0072410587));
#53888=CARTESIAN_POINT('Ctrl Pts',(17.6259851648555,-0.891966644984383,
125.038819724726));
#53889=CARTESIAN_POINT('Ctrl Pts',(18.0646216855069,-1.17653632770684,125.070541677722));
#53890=CARTESIAN_POINT('Ctrl Pts',(18.5835903524298,-1.25749741759416,125.102408415057));
#53891=CARTESIAN_POINT('Ctrl Pts',(19.0926894321616,-1.11879529614231,125.134421335534));
#53892=CARTESIAN_POINT('Ctrl Pts',(19.5026149129719,-0.782711247384195,
125.166581738493));
#53893=CARTESIAN_POINT('Ctrl Pts',(19.7406123902142,-0.306315724372236,
125.198890823782));
#53894=CARTESIAN_POINT('Ctrl Pts',(19.763377196559,0.228205370079604,125.231349690489));
#53895=CARTESIAN_POINT('Ctrl Pts',(19.5649172248906,0.727715249646334,125.263959335904));
#53896=CARTESIAN_POINT('Ctrl Pts',(19.1779529512479,1.10434350393728,125.296720654766));
#53897=CARTESIAN_POINT('Ctrl Pts',(18.6685471091754,1.29093449008952,125.329634438753));
#53898=CARTESIAN_POINT('Ctrl Pts',(18.1248397471563,1.25301197202037,125.362701376505));
#53899=CARTESIAN_POINT('Ctrl Pts',(17.6418067436561,0.995129105561402,125.395922052864));
#53900=CARTESIAN_POINT('Ctrl Pts',(17.304675613873,0.560436926500678,125.429296948111));
#53901=CARTESIAN_POINT('Ctrl Pts',(17.1738931640657,0.0234819648278402,
125.462826437776));
#53902=CARTESIAN_POINT('Ctrl Pts',(17.2742957831578,-0.522569202305958,
125.496510792449));
#53903=CARTESIAN_POINT('Ctrl Pts',(17.5904222067807,-0.982091337162969,
125.530350177997));
#53904=CARTESIAN_POINT('Ctrl Pts',(18.0688496230519,-1.27374502034201,125.564344655041));
#53905=CARTESIAN_POINT('Ctrl Pts',(18.6272097306155,-1.34487226270198,125.598494178829));
#53906=CARTESIAN_POINT('Ctrl Pts',(19.1683660928709,-1.1809955468391,125.632798599234));
#53907=CARTESIAN_POINT('Ctrl Pts',(19.5973138861129,-0.808707366036644,
125.66725766123));
#53908=CARTESIAN_POINT('Ctrl Pts',(19.8378617402874,-0.291381019313683,
125.701871005098));
#53909=CARTESIAN_POINT('Ctrl Pts',(19.8461655054361,0.281611275571365,125.736638166297));
#53910=CARTESIAN_POINT('Ctrl Pts',(19.6187093753557,0.810340152829362,125.771558575736));
#53911=CARTESIAN_POINT('Ctrl Pts',(19.1932825865189,1.2017528384317,125.80663156022));
#53912=CARTESIAN_POINT('Ctrl Pts',(18.6427164183581,1.38605643974671,125.84185634338));
#53913=CARTESIAN_POINT('Ctrl Pts',(18.06241569551,1.32916466473217,125.877232046069));
#53914=CARTESIAN_POINT('Ctrl Pts',(17.5538188909499,1.03898710476137,125.912757686413));
#53915=CARTESIAN_POINT('Ctrl Pts',(17.2066554729585,0.564402394819162,125.948432180681));
#53916=CARTESIAN_POINT('Ctrl Pts',(17.0831057440289,-0.0129682738891071,
125.984254343941));
#53917=CARTESIAN_POINT('Ctrl Pts',(17.206661494287,-0.592804847205485,126.020222891627));
#53918=CARTESIAN_POINT('Ctrl Pts',(17.5576842541618,-1.07353244121064,126.056336440009));
#53919=CARTESIAN_POINT('Ctrl Pts',(18.0764978235536,-1.37013019917798,126.092593506525));
#53920=CARTESIAN_POINT('Ctrl Pts',(18.6735343577048,-1.42917975270743,126.128992511042));
#53921=CARTESIAN_POINT('Ctrl Pts',(19.244809461307,-1.23848730738719,126.165531776955));
#53922=CARTESIAN_POINT('Ctrl Pts',(19.6900510063658,-0.82954528750613,126.202209533138));
#53923=CARTESIAN_POINT('Ctrl Pts',(19.9303178180715,-0.27234395879086,126.239023914679));
#53924=CARTESIAN_POINT('Ctrl Pts',(19.9220090897997,0.336615072122217,126.275972963622));
#53925=CARTESIAN_POINT('Ctrl Pts',(19.6647751325692,0.891050062438758,126.31305462995));
#53926=CARTESIAN_POINT('Ctrl Pts',(19.2018945677896,1.2934708225086,126.350266774275));
#53927=CARTESIAN_POINT('Ctrl Pts',(18.6129942519167,1.47234279082316,126.387607168055));
#53928=CARTESIAN_POINT('Ctrl Pts',(18.0003383532154,1.39481561583623,126.425073498411));
#53929=CARTESIAN_POINT('Ctrl Pts',(17.4710441936286,1.07275201436481,126.462663362284));
#53930=CARTESIAN_POINT('Ctrl Pts',(17.1183317039518,0.560944190799558,126.50037427996));
#53931=CARTESIAN_POINT('Ctrl Pts',(17.005074408946,-0.0522090232566247,
126.538203675335));
#53932=CARTESIAN_POINT('Ctrl Pts',(17.1525942214981,-0.660000712358473,
126.576148919226));
#53933=CARTESIAN_POINT('Ctrl Pts',(17.5366335567734,-1.15599588704851,126.61420725445));
#53934=CARTESIAN_POINT('Ctrl Pts',(18.091387243059,-1.45273381657987,126.652375940072));
#53935=CARTESIAN_POINT('Ctrl Pts',(18.7206933102241,-1.49710973462917,126.690651984097));
#53936=CARTESIAN_POINT('Ctrl Pts',(19.3149140521246,-1.28001029482722,126.729032652734));
#53937=CARTESIAN_POINT('Ctrl Pts',(19.6939106937694,-0.911595961366083,
126.761100859654));
#53938=CARTESIAN_POINT('Ctrl Pts',(19.8874259515692,-0.542567102648363,
126.786804946702));
#53939=CARTESIAN_POINT('Ctrl Pts',(20.0005163718621,-0.140992715157832,
126.812540864656));
#53940=CARTESIAN_POINT('Ctrl Pts',(19.9783846453537,0.389756960668105,126.844770741793));
#53941=CARTESIAN_POINT('Ctrl Pts',(19.6931858388931,0.961601125511805,126.883538256357));
#53942=CARTESIAN_POINT('Ctrl Pts',(19.1982285350886,1.36801288546453,126.922394650787));
#53943=CARTESIAN_POINT('Ctrl Pts',(18.5790486568211,1.53717771774434,126.961336325338));
#53944=CARTESIAN_POINT('Ctrl Pts',(17.9434620985098,1.43847641014473,127.00036001531));
#53945=CARTESIAN_POINT('Ctrl Pts',(17.4025305069054,1.08807198436899,127.039462191361));
#53946=CARTESIAN_POINT('Ctrl Pts',(17.0512361470141,0.54624806009065,127.078639381396));
#53947=CARTESIAN_POINT('Ctrl Pts',(16.9517077315689,-0.0929686702243292,
127.117888002863));
#53948=CARTESIAN_POINT('Ctrl Pts',(17.1222463114711,-0.718163540663969,
127.157204457133));
#53949=CARTESIAN_POINT('Ctrl Pts',(17.5339434625442,-1.21998914182436,127.19658508366));
#53950=CARTESIAN_POINT('Ctrl Pts',(18.1155967869452,-1.51033102531911,127.236026186941));
#53951=CARTESIAN_POINT('Ctrl Pts',(18.7660430040738,-1.53781009856395,127.275524023559));
#53952=CARTESIAN_POINT('Ctrl Pts',(19.3717918130506,-1.29689267540796,127.315074816817));
#53953=CARTESIAN_POINT('Ctrl Pts',(19.8268676166408,-0.828987338375049,
127.354674747443));
#53954=CARTESIAN_POINT('Ctrl Pts',(20.0513901487869,-0.215314584492064,
127.394319979104));
#53955=CARTESIAN_POINT('Ctrl Pts',(20.0056247885481,0.437220847592708,127.434006605569));
#53956=CARTESIAN_POINT('Ctrl Pts',(19.6970292834836,1.01469415427502,127.473730785989));
#53957=CARTESIAN_POINT('Ctrl Pts',(19.1790406081284,1.41609068632597,127.513488447827));
#53958=CARTESIAN_POINT('Ctrl Pts',(18.5418069825858,1.57101927908706,127.553275902336));
#53959=CARTESIAN_POINT('Ctrl Pts',(17.8964518857884,1.45207521426841,127.593088663885));
#53960=CARTESIAN_POINT('Ctrl Pts',(17.3556834232758,1.07970902742724,127.632923803203));
#53961=CARTESIAN_POINT('Ctrl Pts',(17.0140118977188,0.51868953019775,127.67277499967));
#53962=CARTESIAN_POINT('Ctrl Pts',(16.9312778521344,-0.133172545850757,
127.712643022715));
#53963=CARTESIAN_POINT('Ctrl Pts',(17.1220561745599,-0.76213953351389,127.752514978792));
#53964=CARTESIAN_POINT('Ctrl Pts',(17.5531223975555,-1.25833079809336,127.792401469815));
#53965=CARTESIAN_POINT('Ctrl Pts',(18.1494131749782,-1.53533610223328,127.832275370586));
#53966=CARTESIAN_POINT('Ctrl Pts',(18.8065933902536,-1.54432387682768,127.872171702413));
#53967=CARTESIAN_POINT('Ctrl Pts',(19.4100846272743,-1.28470708623083,127.912013923037));
#53968=CARTESIAN_POINT('Ctrl Pts',(19.8553100567167,-0.800375183111611,
127.951925887971));
#53969=CARTESIAN_POINT('Ctrl Pts',(20.0620620209392,-0.177762818146075,
127.991730529943));
#53970=CARTESIAN_POINT('Ctrl Pts',(20.0107296154146,0.365589401403285,128.024893024048));
#53971=CARTESIAN_POINT('Ctrl Pts',(19.8357953855363,0.761539243405002,128.051554711982));
#53972=CARTESIAN_POINT('Ctrl Pts',(19.6452972740319,1.02316795505993,128.071406241808));
#53973=CARTESIAN_POINT('Ctrl Pts',(19.407210271182,1.23882439608857,128.091206748466));
#53974=CARTESIAN_POINT('Ctrl Pts',(19.1325396712143,1.39988486175236,128.11111275206));
#53975=CARTESIAN_POINT('Ctrl Pts',(18.8296995883577,1.49940467423635,128.13113008268));
#53976=CARTESIAN_POINT('Ctrl Pts',(18.6146747329585,1.52230732399087,128.14430771094));
#53977=CARTESIAN_POINT('Ctrl Pts',(18.5048864505563,1.5232313661321,128.150806833261));
#53978=CARTESIAN_POINT('Ctrl Pts',(18.503702102348,1.49187608452152,112.989819674269));
#53979=CARTESIAN_POINT('Ctrl Pts',(18.3422645099611,1.49051733169978,112.999376273846));
#53980=CARTESIAN_POINT('Ctrl Pts',(18.1342705602965,1.45751807004094,113.012344390846));
#53981=CARTESIAN_POINT('Ctrl Pts',(17.8452633513425,1.34504789031967,113.031870507882));
#53982=CARTESIAN_POINT('Ctrl Pts',(17.6217687342541,1.21407386996056,113.048070801922));
#53983=CARTESIAN_POINT('Ctrl Pts',(17.3892912666459,1.00346179778602,113.067402258741));
#53984=CARTESIAN_POINT('Ctrl Pts',(17.2037216055837,0.748497642797482,113.086747828487));
#53985=CARTESIAN_POINT('Ctrl Pts',(17.0336365108725,0.363545641583294,113.112667763901));
#53986=CARTESIAN_POINT('Ctrl Pts',(16.9838992701375,-0.164270544608415,
113.144881746288));
#53987=CARTESIAN_POINT('Ctrl Pts',(17.184414544988,-0.767606361945544,113.183457189884));
#53988=CARTESIAN_POINT('Ctrl Pts',(17.6148373907955,-1.23555595231335,113.22202910865));
#53989=CARTESIAN_POINT('Ctrl Pts',(18.1969329026072,-1.48583931834946,113.260456741484));
#53990=CARTESIAN_POINT('Ctrl Pts',(18.8291856162506,-1.47700694025217,113.298838743469));
#53991=CARTESIAN_POINT('Ctrl Pts',(19.4015066537589,-1.21098811797121,113.33711466563));
#53992=CARTESIAN_POINT('Ctrl Pts',(19.8142041984067,-0.735692713550003,
113.375312027302));
#53993=CARTESIAN_POINT('Ctrl Pts',(19.9963547857532,-0.134671109049916,
113.413410387617));
#53994=CARTESIAN_POINT('Ctrl Pts',(19.917330891654,0.486756209803174,113.451417790248));
#53995=CARTESIAN_POINT('Ctrl Pts',(19.5922047575127,1.02032870198499,113.489324957824));
#53996=CARTESIAN_POINT('Ctrl Pts',(19.078874366281,1.37362515945365,113.52713270191));
#53997=CARTESIAN_POINT('Ctrl Pts',(18.4676774825549,1.48612836610816,113.564836685417));
#53998=CARTESIAN_POINT('Ctrl Pts',(17.8655356424751,1.33958682630473,113.602435135098));
#53999=CARTESIAN_POINT('Ctrl Pts',(17.3771760059416,0.960974919452283,113.639925184264));
#54000=CARTESIAN_POINT('Ctrl Pts',(17.0869162747918,0.417523224711967,113.677304608079));
#54001=CARTESIAN_POINT('Ctrl Pts',(17.0440749027117,-0.195226772711976,
113.71457097036));
#54002=CARTESIAN_POINT('Ctrl Pts',(17.2545974993079,-0.770247029667065,
113.751722040204));
#54003=CARTESIAN_POINT('Ctrl Pts',(17.6802710535475,-1.20773830122854,113.788755639842));
#54004=CARTESIAN_POINT('Ctrl Pts',(18.2456876606402,-1.43247667120123,113.825669614301));
#54005=CARTESIAN_POINT('Ctrl Pts',(18.8515648963708,-1.40675519342341,113.862462044251));
#54006=CARTESIAN_POINT('Ctrl Pts',(19.3922868480658,-1.13670944017846,113.899130819509));
#54007=CARTESIAN_POINT('Ctrl Pts',(19.7742257196495,-0.670960827012895,
113.935674250634));
#54008=CARTESIAN_POINT('Ctrl Pts',(19.9320734373548,-0.0918667144545759,
113.972090450819));
#54009=CARTESIAN_POINT('Ctrl Pts',(19.8399466317867,0.499115736790983,114.008377780349));
#54010=CARTESIAN_POINT('Ctrl Pts',(19.5156401611027,0.999094041612395,114.04453464138));
#54011=CARTESIAN_POINT('Ctrl Pts',(19.0172239827432,1.32186020605331,114.080559487712));
#54012=CARTESIAN_POINT('Ctrl Pts',(18.5300585493413,1.39736634472576,114.110469050883));
#54013=CARTESIAN_POINT('Ctrl Pts',(18.1483743883582,1.33483384505807,114.134329289553));
#54014=CARTESIAN_POINT('Ctrl Pts',(17.7885335979758,1.19494779695115,114.158144392525));
#54015=CARTESIAN_POINT('Ctrl Pts',(17.4104234910095,0.884458943355539,114.187828360597));
#54016=CARTESIAN_POINT('Ctrl Pts',(17.149528329175,0.360991850767247,114.223311911424));
#54017=CARTESIAN_POINT('Ctrl Pts',(17.1252556722554,-0.221068002059184,
114.258657303518));
#54018=CARTESIAN_POINT('Ctrl Pts',(17.3400117396107,-0.760164790222631,
114.293863534424));
#54019=CARTESIAN_POINT('Ctrl Pts',(17.7545646722328,-1.16290679171789,114.328929746419));
#54020=CARTESIAN_POINT('Ctrl Pts',(18.2952857435863,-1.36040896104986,114.363855170088));
#54021=CARTESIAN_POINT('Ctrl Pts',(18.8671866034673,-1.31998953853843,114.398639127519));
#54022=CARTESIAN_POINT('Ctrl Pts',(19.3706351176622,-1.05061228142374,114.433281034536));
#54023=CARTESIAN_POINT('Ctrl Pts',(19.7187089419615,-0.600950303027163,
114.467780414332));
#54024=CARTESIAN_POINT('Ctrl Pts',(19.8522062868052,-0.0506348125539401,
114.502136873029));
#54025=CARTESIAN_POINT('Ctrl Pts',(19.7497138563351,0.503904640082804,114.536350121929));
#54026=CARTESIAN_POINT('Ctrl Pts',(19.431010210694,0.966252463287474,114.570419973524));
#54027=CARTESIAN_POINT('Ctrl Pts',(18.9532691100971,1.25688267561954,114.604346322718));
#54028=CARTESIAN_POINT('Ctrl Pts',(18.4008406216132,1.32673243891578,114.638129178272));
#54029=CARTESIAN_POINT('Ctrl Pts',(17.8703226360875,1.16554167126788,114.671768634545));
#54030=CARTESIAN_POINT('Ctrl Pts',(17.4536942068799,0.803271481279279,114.705264891447));
#54031=CARTESIAN_POINT('Ctrl Pts',(17.2223629014042,0.304561077237039,114.738618237817));
#54032=CARTESIAN_POINT('Ctrl Pts',(17.2149314218132,-0.242783176148081,
114.77182907043));
#54033=CARTESIAN_POINT('Ctrl Pts',(17.4307882423904,-0.743289781556822,
114.804897864875));
#54034=CARTESIAN_POINT('Ctrl Pts',(17.8305161533526,-1.11037437400687,114.837825225747));
#54035=CARTESIAN_POINT('Ctrl Pts',(18.3431414371818,-1.28149381786692,114.870611792906));
#54036=CARTESIAN_POINT('Ctrl Pts',(18.7893553523156,-1.23727626130552,114.897817313457));
#54037=CARTESIAN_POINT('Ctrl Pts',(19.1112128056895,-1.09554793991547,114.919512124933));
#54038=CARTESIAN_POINT('Ctrl Pts',(19.396175350928,-0.890697859688692,114.941160733749));
#54039=CARTESIAN_POINT('Ctrl Pts',(19.6584018411182,-0.531669188250831,
114.968135177746));
#54040=CARTESIAN_POINT('Ctrl Pts',(19.76908647096,-0.0120339067964489,115.000367371872));
#54041=CARTESIAN_POINT('Ctrl Pts',(19.6583942300963,0.505266606576981,115.032463636213));
#54042=CARTESIAN_POINT('Ctrl Pts',(19.3473557859062,0.93046495841335,115.064425180333));
#54043=CARTESIAN_POINT('Ctrl Pts',(18.8916950780005,1.19043640343731,115.096253363284));
#54044=CARTESIAN_POINT('Ctrl Pts',(18.3717570032792,1.24142340224108,115.127949584784));
#54045=CARTESIAN_POINT('Ctrl Pts',(17.8783677920246,1.07626545587742,115.15951539726));
#54046=CARTESIAN_POINT('Ctrl Pts',(17.4970559877627,0.725456658754698,115.190952339247));
#54047=CARTESIAN_POINT('Ctrl Pts',(17.2930596087315,0.251374726199106,115.222262219888));
#54048=CARTESIAN_POINT('Ctrl Pts',(17.2997368545718,-0.205413166433051,
115.249981653063));
#54049=CARTESIAN_POINT('Ctrl Pts',(17.4404319127292,-0.573042786265209,
115.274156363673));
#54050=CARTESIAN_POINT('Ctrl Pts',(17.592066785102,-0.774671677260083,115.289656127754));
#54051=CARTESIAN_POINT('Ctrl Pts',(17.7139015205345,-0.888101474402246,
115.29997296064));
#54052=CARTESIAN_POINT('Ctrl Pts',(17.7785097005419,-0.940424780251118,
115.305127839623));
#54053=CARTESIAN_POINT('Ctrl Pts',(17.8466470444457,-0.98801547265171,115.310279486813));
#54054=CARTESIAN_POINT('Ctrl Pts',(17.989070409944,-1.07344813179845,115.320575730976));
#54055=CARTESIAN_POINT('Ctrl Pts',(18.2236591817274,-1.16292300047207,115.335996045863));
#54056=CARTESIAN_POINT('Ctrl Pts',(18.5563155957279,-1.19093988306076,115.3565030506));
#54057=CARTESIAN_POINT('Ctrl Pts',(18.8830047845655,-1.12589266484945,115.376958878633));
#54058=CARTESIAN_POINT('Ctrl Pts',(19.1780050081399,-0.9733951898541,115.397362889332));
#54059=CARTESIAN_POINT('Ctrl Pts',(19.4189487015537,-0.745659756110988,
115.417716885332));
#54060=CARTESIAN_POINT('Ctrl Pts',(19.586513319755,-0.460981781034244,115.438020595246));
#54061=CARTESIAN_POINT('Ctrl Pts',(19.6971134584733,-0.0350499051287504,
115.465026998031));
#54062=CARTESIAN_POINT('Ctrl Pts',(19.6213835081677,0.409308743056556,115.491936476127));
#54063=CARTESIAN_POINT('Ctrl Pts',(19.4081815400465,0.726708802320049,115.515399793606));
#54064=CARTESIAN_POINT('Ctrl Pts',(19.2533820709519,0.877517364647426,115.528784631642));
#54065=CARTESIAN_POINT('Ctrl Pts',(19.0787709601167,1.00501199378957,115.542153884178));
#54066=CARTESIAN_POINT('Ctrl Pts',(18.9053740303453,1.0826747173383,115.553831967145));
#54067=CARTESIAN_POINT('Ctrl Pts',(18.7488682526583,1.1217999761029,115.56382821947));
#54068=CARTESIAN_POINT('Ctrl Pts',(18.6695549654301,1.13586113853869,115.568823416288));
#54069=CARTESIAN_POINT('Ctrl Pts',(18.6028029629378,1.14293032142239,115.57298384464));
#54070=CARTESIAN_POINT('Ctrl Pts',(18.5492301296799,1.14569963267631,115.576310658733));
#54071=CARTESIAN_POINT('Ctrl Pts',(18.3318189962245,1.14985398886929,115.589799489503));
#54072=CARTESIAN_POINT('Ctrl Pts',(17.93807646621,1.04913122524392,115.61423125823));
#54073=CARTESIAN_POINT('Ctrl Pts',(17.6038273489929,0.738872428658555,115.641663000481));
#54074=CARTESIAN_POINT('Ctrl Pts',(17.4553862402826,0.459584671101082,115.661208854169));
#54075=CARTESIAN_POINT('Ctrl Pts',(17.404909185234,0.310016726484566,115.670970109025));
#54076=CARTESIAN_POINT('Ctrl Pts',(17.3801146498094,0.186574169585243,115.67877223044));
#54077=CARTESIAN_POINT('Ctrl Pts',(17.3505224034491,-0.0633246010535821,
115.694366612529));
#54078=CARTESIAN_POINT('Ctrl Pts',(17.4237971555624,-0.477375899585048,
115.719655510759));
#54079=CARTESIAN_POINT('Ctrl Pts',(17.7858376869751,-0.931108485774203,
115.754551104908));
#54080=CARTESIAN_POINT('Ctrl Pts',(18.2745211046451,-1.13667010750685,115.786433819311));
#54081=CARTESIAN_POINT('Ctrl Pts',(18.7484690587498,-1.11846305743127,115.81533834407));
#54082=CARTESIAN_POINT('Ctrl Pts',(19.1386709996485,-0.948289610488192,
115.84129311261));
#54083=CARTESIAN_POINT('Ctrl Pts',(19.4390996247751,-0.647682388358762,
115.867191006533));
#54084=CARTESIAN_POINT('Ctrl Pts',(19.5802476090257,-0.323886197170617,
115.888726654306));
#54085=CARTESIAN_POINT('Ctrl Pts',(19.6164608276318,-0.0476515215733575,
115.905929464203));
#54086=CARTESIAN_POINT('Ctrl Pts',(19.6048021299846,0.160672150153393,115.918818002215));
#54087=CARTESIAN_POINT('Ctrl Pts',(19.5629552356086,0.329344380429827,115.92954886288));
#54088=CARTESIAN_POINT('Ctrl Pts',(19.5111419167609,0.457709038523884,115.938127090231));
#54089=CARTESIAN_POINT('Ctrl Pts',(19.4159798157258,0.642183917490576,115.950988089536));
#54090=CARTESIAN_POINT('Ctrl Pts',(19.2097310734986,0.881763831274916,115.970258025515));
#54091=CARTESIAN_POINT('Ctrl Pts',(18.8376888372652,1.07831902356411,115.995905289709));
#54092=CARTESIAN_POINT('Ctrl Pts',(18.420246143728,1.12529003433152,116.021509895766));
#54093=CARTESIAN_POINT('Ctrl Pts',(18.1164398186431,1.04383241287061,116.040683067193));
#54094=CARTESIAN_POINT('Ctrl Pts',(17.935182926549,0.945722916711651,116.053453203537));
#54095=CARTESIAN_POINT('Ctrl Pts',(17.8209867836636,0.869446264038907,116.061963256023));
#54096=CARTESIAN_POINT('Ctrl Pts',(17.6412091504734,0.708850503681455,116.076848878371));
#54097=CARTESIAN_POINT('Ctrl Pts',(17.5206165699508,0.517177860963483,116.090655859422));
#54098=CARTESIAN_POINT('Ctrl Pts',(17.4619719522485,0.356352158450434,116.101269186923));
#54099=CARTESIAN_POINT('Ctrl Pts',(17.4465783138213,0.307388824240754,116.104452776497));
#54100=CARTESIAN_POINT('Ctrl Pts',(17.4335399348317,0.257734727890675,116.107635795408));
#54101=CARTESIAN_POINT('Ctrl Pts',(17.4228231536783,0.207551498411839,116.110818346632));
#54102=CARTESIAN_POINT('Ctrl Pts',(17.4144491679001,0.156922359184113,116.114000351126));
#54103=CARTESIAN_POINT('Ctrl Pts',(17.4065086961841,0.0889837600333896,
116.118242356133));
#54104=CARTESIAN_POINT('Ctrl Pts',(17.3975764169991,-0.0990303571900397,
116.129904811033));
#54105=CARTESIAN_POINT('Ctrl Pts',(17.4557897410273,-0.406430268110572,
116.148975549028));
#54106=CARTESIAN_POINT('Ctrl Pts',(17.6775193909147,-0.759239865060753,
116.174374346993));
#54107=CARTESIAN_POINT('Ctrl Pts',(18.0124729574942,-1.00640471012008,116.199748244809));
#54108=CARTESIAN_POINT('Ctrl Pts',(18.4142334421369,-1.11401582947692,116.225098996324));
#54109=CARTESIAN_POINT('Ctrl Pts',(18.8271625055921,-1.0674620377526,116.250429703679));
#54110=CARTESIAN_POINT('Ctrl Pts',(19.1943590995122,-0.873386967180604,
116.275742455032));
#54111=CARTESIAN_POINT('Ctrl Pts',(19.4048227403936,-0.628698108618376,
116.295418901538));
#54112=CARTESIAN_POINT('Ctrl Pts',(19.5057918819382,-0.425410293547205,
116.309468193535));
#54113=CARTESIAN_POINT('Ctrl Pts',(19.5656339219958,-0.254098208903609,
116.320706689353));
#54114=CARTESIAN_POINT('Ctrl Pts',(19.6137410150594,0.0618235256489764,
116.340368827849));
#54115=CARTESIAN_POINT('Ctrl Pts',(19.5099378325633,0.517016389985175,116.368448290932));
#54116=CARTESIAN_POINT('Ctrl Pts',(19.1391182957214,0.937107132493867,116.40213348579));
#54117=CARTESIAN_POINT('Ctrl Pts',(18.6128054716757,1.12867451927067,116.435815336319));
#54118=CARTESIAN_POINT('Ctrl Pts',(18.058785719797,1.04521466627339,116.469499752536));
#54119=CARTESIAN_POINT('Ctrl Pts',(17.6772819616439,0.756169197308419,116.498279566654));
#54120=CARTESIAN_POINT('Ctrl Pts',(17.4803749568857,0.421072765008975,116.522153929673));
#54121=CARTESIAN_POINT('Ctrl Pts',(17.3766797417797,0.0225849405462479,
116.547440772492));
#54122=CARTESIAN_POINT('Ctrl Pts',(17.465295524311,-0.500202217111396,116.579066566679));
#54123=CARTESIAN_POINT('Ctrl Pts',(17.889792472491,-0.975335446352908,116.617054365501));
#54124=CARTESIAN_POINT('Ctrl Pts',(18.502637561406,-1.15197604515318,116.655087623956));
#54125=CARTESIAN_POINT('Ctrl Pts',(19.1163786805987,-0.975332764938637,
116.693175009599));
#54126=CARTESIAN_POINT('Ctrl Pts',(19.5429506803428,-0.49832909128163,116.73132532745));
#54127=CARTESIAN_POINT('Ctrl Pts',(19.6323015217028,0.0281297749259298,
116.763176460355));
#54128=CARTESIAN_POINT('Ctrl Pts',(19.5277627412065,0.430370844822526,116.788697635011));
#54129=CARTESIAN_POINT('Ctrl Pts',(19.369679999767,0.6992353885053,116.807859099239));
#54130=CARTESIAN_POINT('Ctrl Pts',(19.1424632389321,0.913533103672042,116.827043111286));
#54131=CARTESIAN_POINT('Ctrl Pts',(18.772367790744,1.10567953941629,116.852652017112));
#54132=CARTESIAN_POINT('Ctrl Pts',(18.2355341126458,1.13621815304612,116.884723808745));
#54133=CARTESIAN_POINT('Ctrl Pts',(17.6689198164127,0.823295827742766,116.923314310429));
#54134=CARTESIAN_POINT('Ctrl Pts',(17.3547647490283,0.255422345016107,116.962017521189));
#54135=CARTESIAN_POINT('Ctrl Pts',(17.3909543071043,-0.394665908212814,
117.00084115596));
#54136=CARTESIAN_POINT('Ctrl Pts',(17.7687099122216,-0.927569838505474,
117.039793042541));
#54137=CARTESIAN_POINT('Ctrl Pts',(18.3741755754646,-1.17872989356506,117.078880711992));
#54138=CARTESIAN_POINT('Ctrl Pts',(19.0228384514425,-1.06886607959656,117.118111607769));
#54139=CARTESIAN_POINT('Ctrl Pts',(19.5155163757392,-0.629071317918103,
117.15749296697));
#54140=CARTESIAN_POINT('Ctrl Pts',(19.6994420911959,0.00797209925389068,
117.197031859252));
#54141=CARTESIAN_POINT('Ctrl Pts',(19.515500647011,0.647878257780649,117.23673514959));
#54142=CARTESIAN_POINT('Ctrl Pts',(19.0171733063539,1.09376372921043,117.27660952184));
#54143=CARTESIAN_POINT('Ctrl Pts',(18.3550699462677,1.20669326786917,117.316661446212));
#54144=CARTESIAN_POINT('Ctrl Pts',(17.731513825934,0.948886060096873,117.356897172836));
#54145=CARTESIAN_POINT('Ctrl Pts',(17.3388450878967,0.396256579223924,117.39732273553));
#54146=CARTESIAN_POINT('Ctrl Pts',(17.3001759338416,-0.283860165024669,
117.437943945886));
#54147=CARTESIAN_POINT('Ctrl Pts',(17.6309104423397,-0.883255559054568,
117.478766367029));
#54148=CARTESIAN_POINT('Ctrl Pts',(18.2328525117844,-1.21651929036585,117.519795325694));
#54149=CARTESIAN_POINT('Ctrl Pts',(18.9234234044072,-1.17823144343809,117.561035895459));
#54150=CARTESIAN_POINT('Ctrl Pts',(19.4906656002749,-0.776372273993139,
117.602492914177));
#54151=CARTESIAN_POINT('Ctrl Pts',(19.7587364840262,-0.13078846109893,117.644170910344));
#54152=CARTESIAN_POINT('Ctrl Pts',(19.6608941213843,0.446513363382881,117.679090346474));
#54153=CARTESIAN_POINT('Ctrl Pts',(19.4063763506229,0.825732225186209,117.707140502678));
#54154=CARTESIAN_POINT('Ctrl Pts',(19.0572403859771,1.12201758553148,117.735267815038));
#54155=CARTESIAN_POINT('Ctrl Pts',(18.4885802358337,1.2865381867526,117.770572480421));
#54156=CARTESIAN_POINT('Ctrl Pts',(17.801838273725,1.08919683440124,117.813174713138));
#54157=CARTESIAN_POINT('Ctrl Pts',(17.3227121836494,0.553921475501694,117.856016594786));
#54158=CARTESIAN_POINT('Ctrl Pts',(17.2010966707053,-0.158326099518395,
117.899101101152));
#54159=CARTESIAN_POINT('Ctrl Pts',(17.4786390279773,-0.829851682392695,
117.942430781901));
#54160=CARTESIAN_POINT('Ctrl Pts',(18.0742946344301,-1.25323173475652,117.986007964128));
#54161=CARTESIAN_POINT('Ctrl Pts',(18.8080726935777,-1.29501226255686,118.029834639599));
#54162=CARTESIAN_POINT('Ctrl Pts',(19.4553159300046,-0.938010475541138,
118.073912516848));
#54163=CARTESIAN_POINT('Ctrl Pts',(19.8154307819553,-0.287585555372444,
118.118242990085));
#54164=CARTESIAN_POINT('Ctrl Pts',(19.7741366820081,0.458836644666698,118.16282715909));
#54165=CARTESIAN_POINT('Ctrl Pts',(19.3394435327949,1.07263691503397,118.207665807633));
#54166=CARTESIAN_POINT('Ctrl Pts',(18.7575552739269,1.31396042818269,118.24524382035));
#54167=CARTESIAN_POINT('Ctrl Pts',(18.2660136694013,1.29932960507879,118.275433796398));
#54168=CARTESIAN_POINT('Ctrl Pts',(17.9138511199113,1.18752313651639,118.298140055659));
#54169=CARTESIAN_POINT('Ctrl Pts',(17.6055358088652,0.98141598551866,118.320910047554));
#54170=CARTESIAN_POINT('Ctrl Pts',(17.3656586969673,0.69755141465935,118.343743757908));
#54171=CARTESIAN_POINT('Ctrl Pts',(17.2133153242065,0.357232692236245,118.366641084558));
#54172=CARTESIAN_POINT('Ctrl Pts',(17.1610033132225,-0.0128449924121692,
118.389601986026));
#54173=CARTESIAN_POINT('Ctrl Pts',(17.2133047298867,-0.384104530010112,
118.412626315514));
#54174=CARTESIAN_POINT('Ctrl Pts',(17.3412396152671,-0.669931994924582,
118.431866032995));
#54175=CARTESIAN_POINT('Ctrl Pts',(17.4883028212069,-0.871293451744624,
118.447289433679));
#54176=CARTESIAN_POINT('Ctrl Pts',(17.6623643786738,-1.04999788798832,118.46273378822));
#54177=CARTESIAN_POINT('Ctrl Pts',(18.0285864515854,-1.29592018799767,118.489816685333));
#54178=CARTESIAN_POINT('Ctrl Pts',(18.6703881436677,-1.40571108227618,118.528663586766));
#54179=CARTESIAN_POINT('Ctrl Pts',(19.3970876386868,-1.1053408950482,118.575529603312));
#54180=CARTESIAN_POINT('Ctrl Pts',(19.7780709579159,-0.568789994131528,
118.614791183341));
#54181=CARTESIAN_POINT('Ctrl Pts',(19.8649536567208,-0.127762187171968,
118.642381544121));
#54182=CARTESIAN_POINT('Ctrl Pts',(19.8615540247625,0.127284981139844,118.658178190531));
#54183=CARTESIAN_POINT('Ctrl Pts',(19.8223396408192,0.380112246085207,118.673994886313));
#54184=CARTESIAN_POINT('Ctrl Pts',(19.7071782081534,0.681042071721743,118.693803936495));
#54185=CARTESIAN_POINT('Ctrl Pts',(19.3968645270032,1.09527626728677,118.725578754282));
#54186=CARTESIAN_POINT('Ctrl Pts',(18.8122225330156,1.41911251137611,118.76544746249));
#54187=CARTESIAN_POINT('Ctrl Pts',(18.007042177151,1.3744471680488,118.813526770773));
#54188=CARTESIAN_POINT('Ctrl Pts',(17.3459220719172,0.90601479701624,118.86183971331));
#54189=CARTESIAN_POINT('Ctrl Pts',(17.0861041214154,0.279551870891405,118.902291882144));
#54190=CARTESIAN_POINT('Ctrl Pts',(17.1019462138081,-0.24916096313258,118.93476676582));
#54191=CARTESIAN_POINT('Ctrl Pts',(17.2019719756035,-0.564646975838234,
118.955109853082));
#54192=CARTESIAN_POINT('Ctrl Pts',(17.3166223801635,-0.764853864695036,
118.96937458627));
#54193=CARTESIAN_POINT('Ctrl Pts',(17.3934033772786,-0.871630377869911,
118.977532651056));
#54194=CARTESIAN_POINT('Ctrl Pts',(17.477703283774,-0.972842734233704,118.985695303595));
#54195=CARTESIAN_POINT('Ctrl Pts',(17.5959908064179,-1.08787346995914,118.995906958726));
#54196=CARTESIAN_POINT('Ctrl Pts',(17.80940624637,-1.24391112239919,119.012264402582));
#54197=CARTESIAN_POINT('Ctrl Pts',(18.1137047432836,-1.38016569420815,119.032744595313));
#54198=CARTESIAN_POINT('Ctrl Pts',(18.5107756099825,-1.43627485577155,119.057374894024));
#54199=CARTESIAN_POINT('Ctrl Pts',(18.9086887725081,-1.38015979004093,119.082057931785));
#54200=CARTESIAN_POINT('Ctrl Pts',(19.2763086985662,-1.21572919182316,119.106793694273));
#54201=CARTESIAN_POINT('Ctrl Pts',(19.5846796723198,-0.955406316030372,
119.131580970565));
#54202=CARTESIAN_POINT('Ctrl Pts',(19.809392321284,-0.619204248974561,119.15641978872));
#54203=CARTESIAN_POINT('Ctrl Pts',(19.9325091524558,-0.233138195850857,
119.181308555028));
#54204=CARTESIAN_POINT('Ctrl Pts',(19.9439344589339,0.172710845827226,119.206247801915));
#54205=CARTESIAN_POINT('Ctrl Pts',(19.859333630366,0.501021221890519,119.227070700593));
#54206=CARTESIAN_POINT('Ctrl Pts',(19.7388322341717,0.742192001820556,119.243753783559));
#54207=CARTESIAN_POINT('Ctrl Pts',(19.5477513775307,1.02020898738615,119.264627237985));
#54208=CARTESIAN_POINT('Ctrl Pts',(19.1748525603661,1.32647007207184,119.293905797606));
#54209=CARTESIAN_POINT('Ctrl Pts',(18.5746327535004,1.49048570425054,119.33165434782));
#54210=CARTESIAN_POINT('Ctrl Pts',(17.9581548867158,1.3947907252162,119.369505012355));
#54211=CARTESIAN_POINT('Ctrl Pts',(17.433136470404,1.05474858337055,119.407455104193));
#54212=CARTESIAN_POINT('Ctrl Pts',(17.0919383518421,0.528571566609064,119.445501954772));
#54213=CARTESIAN_POINT('Ctrl Pts',(16.9951890882095,-0.0925769725045345,
119.48364264785));
#54214=CARTESIAN_POINT('Ctrl Pts',(17.1609540266251,-0.700571381474122,
119.52187456006));
#54215=CARTESIAN_POINT('Ctrl Pts',(17.4948116280989,-1.10745799563107,119.553807683116));
#54216=CARTESIAN_POINT('Ctrl Pts',(17.8447023681615,-1.33030493897242,119.579397106812));
#54217=CARTESIAN_POINT('Ctrl Pts',(18.2335472691901,-1.47606655473774,119.605014075801));
#54218=CARTESIAN_POINT('Ctrl Pts',(18.7616932453127,-1.49849508652994,119.637086847695));
#54219=CARTESIAN_POINT('Ctrl Pts',(19.3523944101162,-1.26357563907783,119.675653098896));
#54220=CARTESIAN_POINT('Ctrl Pts',(19.796491636114,-0.807043559144156,119.714295292846));
#54221=CARTESIAN_POINT('Ctrl Pts',(20.0157970505624,-0.207778260258124,
119.753010147915));
#54222=CARTESIAN_POINT('Ctrl Pts',(19.9711184784079,0.429920342496358,119.791794464769));
#54223=CARTESIAN_POINT('Ctrl Pts',(19.6693616238384,0.994715766881195,119.830644916317));
#54224=CARTESIAN_POINT('Ctrl Pts',(19.1623979919676,1.38763506879075,119.869558191545));
#54225=CARTESIAN_POINT('Ctrl Pts',(18.5382405530733,1.53942785144906,119.908530869871));
#54226=CARTESIAN_POINT('Ctrl Pts',(17.9055587368166,1.42291065228989,119.947559593151));
#54227=CARTESIAN_POINT('Ctrl Pts',(17.4634685402937,1.11845970679053,119.980127250936));
#54228=CARTESIAN_POINT('Ctrl Pts',(17.2072047563733,0.782220751904666,120.006205932695));
#54229=CARTESIAN_POINT('Ctrl Pts',(17.0259624642235,0.400010121518591,120.032300468687));
#54230=CARTESIAN_POINT('Ctrl Pts',(16.9581031072095,-0.133786264742428,
120.064946918911));
#54231=CARTESIAN_POINT('Ctrl Pts',(17.1456963710106,-0.752388312245989,
120.104164686953));
#54232=CARTESIAN_POINT('Ctrl Pts',(17.5699893730723,-1.2408823945971,120.143420804628));
#54233=CARTESIAN_POINT('Ctrl Pts',(18.1573322171588,-1.51371900905838,120.182711703032));
#54234=CARTESIAN_POINT('Ctrl Pts',(18.8053948529502,-1.52285657093314,120.222033701872));
#54235=CARTESIAN_POINT('Ctrl Pts',(19.4010838377385,-1.26631875735931,120.261383165299));
#54236=CARTESIAN_POINT('Ctrl Pts',(19.8402963026219,-0.788554594843257,
120.30075640158));
#54237=CARTESIAN_POINT('Ctrl Pts',(20.0461617582727,-0.172750782040334,
120.340149724409));
#54238=CARTESIAN_POINT('Ctrl Pts',(19.9825174326225,0.473697806244577,120.379559422821));
#54239=CARTESIAN_POINT('Ctrl Pts',(19.6602768883809,1.03794772706267,120.4189817794));
#54240=CARTESIAN_POINT('Ctrl Pts',(19.1355536795428,1.42145008827222,120.45841306485));
#54241=CARTESIAN_POINT('Ctrl Pts',(18.4998707433376,1.55719588396314,120.497849545716));
#54242=CARTESIAN_POINT('Ctrl Pts',(17.864163205303,1.42145001008791,120.537287485317));
#54243=CARTESIAN_POINT('Ctrl Pts',(17.3393787989982,1.03790924248084,120.57672314656));
#54244=CARTESIAN_POINT('Ctrl Pts',(17.017074206874,0.473557355218691,120.616152792451));
#54245=CARTESIAN_POINT('Ctrl Pts',(16.953408471598,-0.173057796539594,120.655572689844));
#54246=CARTESIAN_POINT('Ctrl Pts',(17.1593374262179,-0.789068501312153,
120.694979112502));
#54247=CARTESIAN_POINT('Ctrl Pts',(17.5987249550259,-1.26702928001241,120.734368344241));
#54248=CARTESIAN_POINT('Ctrl Pts',(18.1946971056568,-1.52369644517567,120.773736681215));
#54249=CARTESIAN_POINT('Ctrl Pts',(18.8431194373237,-1.51455574960213,120.813080431625));
#54250=CARTESIAN_POINT('Ctrl Pts',(19.4308298620431,-1.24155842999136,120.852395921515));
#54251=CARTESIAN_POINT('Ctrl Pts',(19.8554281123154,-0.752716870273097,
120.891679493858));
#54252=CARTESIAN_POINT('Ctrl Pts',(20.0431536703053,-0.133645042672799,
120.930927518414));
#54253=CARTESIAN_POINT('Ctrl Pts',(19.9617251011364,0.507468436214418,120.970136382216));
#54254=CARTESIAN_POINT('Ctrl Pts',(19.6259005154625,1.05880076011582,121.009302510876));
#54255=CARTESIAN_POINT('Ctrl Pts',(19.0948017776786,1.42444673699063,121.048422333788));
#54256=CARTESIAN_POINT('Ctrl Pts',(18.4614843836788,1.5411183959411,121.087492358667));
#54257=CARTESIAN_POINT('Ctrl Pts',(17.8366037551925,1.38915003243965,121.12650904033));
#54258=CARTESIAN_POINT('Ctrl Pts',(17.3290377823205,0.995758540539347,121.165469034314));
#54259=CARTESIAN_POINT('Ctrl Pts',(17.0268896562641,0.430268183212111,121.204368725407));
#54260=CARTESIAN_POINT('Ctrl Pts',(16.9821482492727,-0.208328248111488,
121.243205126464));
#54261=CARTESIAN_POINT('Ctrl Pts',(17.1468513998485,-0.658338107284023,
121.272281854363));
#54262=CARTESIAN_POINT('Ctrl Pts',(17.3270527013809,-0.913793541276511,
121.2916449787));
#54263=CARTESIAN_POINT('Ctrl Pts',(17.46418185158,-1.0705239622011,121.304547220258));
#54264=CARTESIAN_POINT('Ctrl Pts',(17.7451790402857,-1.30479380949971,121.327111265409));
#54265=CARTESIAN_POINT('Ctrl Pts',(18.2380695380599,-1.50090249377063,121.359299336153));
#54266=CARTESIAN_POINT('Ctrl Pts',(18.872952337819,-1.47399830138094,121.397848602223));
#54267=CARTESIAN_POINT('Ctrl Pts',(19.4402270507624,-1.19079335758157,121.43631807797));
#54268=CARTESIAN_POINT('Ctrl Pts',(19.8415184192534,-0.701595659415583,
121.47470479001));
#54269=CARTESIAN_POINT('Ctrl Pts',(20.0076038779129,-0.0925460055625223,
121.513005657936));
#54270=CARTESIAN_POINT('Ctrl Pts',(19.9106710958716,0.529786710311653,121.551217745528));
#54271=CARTESIAN_POINT('Ctrl Pts',(19.5688165951267,1.05697212875173,121.589338130621));
#54272=CARTESIAN_POINT('Ctrl Pts',(19.0427596201426,1.39770166829743,121.62736397679));
#54273=CARTESIAN_POINT('Ctrl Pts',(18.4249973670875,1.4935958090029,121.665292499313));
#54274=CARTESIAN_POINT('Ctrl Pts',(17.8235396206654,1.32923563625104,121.703120986417));
#54275=CARTESIAN_POINT('Ctrl Pts',(17.3429817574642,0.934618133209399,121.740846791978));
#54276=CARTESIAN_POINT('Ctrl Pts',(17.0662946299328,0.379687410860908,121.778467339518));
#54277=CARTESIAN_POINT('Ctrl Pts',(17.0404764052604,-0.238080819165208,
121.815980124477));
#54278=CARTESIAN_POINT('Ctrl Pts',(17.2685662738785,-0.810825747926414,
121.853382712339));
#54279=CARTESIAN_POINT('Ctrl Pts',(17.7093700547578,-1.23915893357272,121.890672750573));
#54280=CARTESIAN_POINT('Ctrl Pts',(18.2849022360115,-1.44943799786466,121.927847950456));
#54281=CARTESIAN_POINT('Ctrl Pts',(18.8942013046416,-1.4064333916413,121.964906125628));
#54282=CARTESIAN_POINT('Ctrl Pts',(19.4310600024741,-1.11924200067342,122.001845121409));
#54283=CARTESIAN_POINT('Ctrl Pts',(19.8025684779115,-0.639390170128088,
122.038662952609));
#54284=CARTESIAN_POINT('Ctrl Pts',(19.9451989003155,-0.051637223723163,
122.075357550695));
#54285=CARTESIAN_POINT('Ctrl Pts',(19.8356891395559,0.541102670830277,122.111927198002));
#54286=CARTESIAN_POINT('Ctrl Pts',(19.4948233406496,1.03568092690009,122.1483699589));
#54287=CARTESIAN_POINT('Ctrl Pts',(18.9834812980339,1.34680051480277,122.184684197437));
#54288=CARTESIAN_POINT('Ctrl Pts',(18.3917927004701,1.42165473989535,122.220868285127));
#54289=CARTESIAN_POINT('Ctrl Pts',(17.823211725378,1.24893790158853,122.256920676789));
#54290=CARTESIAN_POINT('Ctrl Pts',(17.376424697306,0.860487459682125,122.292839947562));
#54291=CARTESIAN_POINT('Ctrl Pts',(17.1282004735361,0.325438701500939,122.328624743665));
#54292=CARTESIAN_POINT('Ctrl Pts',(17.1201969314303,-0.262093773310703,
122.364273793238));
#54293=CARTESIAN_POINT('Ctrl Pts',(17.3519746550279,-0.799579240414161,
122.39978595058));
#54294=CARTESIAN_POINT('Ctrl Pts',(17.7813972457046,-1.19397853058097,122.435160118652));
#54295=CARTESIAN_POINT('Ctrl Pts',(18.3322852669273,-1.3778564057377,122.470395332238));
#54296=CARTESIAN_POINT('Ctrl Pts',(18.9079366722081,-1.32091501639784,122.50549070087));
#54297=CARTESIAN_POINT('Ctrl Pts',(19.408110174119,-1.03496607388862,122.540445426145));
#54298=CARTESIAN_POINT('Ctrl Pts',(19.7464914273704,-0.571545265474727,
122.575258824259));
#54299=CARTESIAN_POINT('Ctrl Pts',(19.8655874804599,-0.0126175132191439,
122.609930280511));
#54300=CARTESIAN_POINT('Ctrl Pts',(19.7464983590342,0.543905007067228,122.644459305606));
#54301=CARTESIAN_POINT('Ctrl Pts',(19.4118682240342,1.00135709037548,122.678845474284));
#54302=CARTESIAN_POINT('Ctrl Pts',(18.9216435947912,1.28105760502164,122.713088499641));
#54303=CARTESIAN_POINT('Ctrl Pts',(18.3622701529655,1.33589566146183,122.747188144647));
#54304=CARTESIAN_POINT('Ctrl Pts',(17.8315352721831,1.15824493019145,122.781144309059));
#54305=CARTESIAN_POINT('Ctrl Pts',(17.4213882328109,0.780879052378252,122.814956965966));
#54306=CARTESIAN_POINT('Ctrl Pts',(17.2020806893666,0.271141102260439,122.848626198319));
#54307=CARTESIAN_POINT('Ctrl Pts',(17.209183784722,-0.220082502602327,122.878427070648));
#54308=CARTESIAN_POINT('Ctrl Pts',(17.3605649792115,-0.61497008299745,122.904410163103));
#54309=CARTESIAN_POINT('Ctrl Pts',(17.6498776696226,-1.00079015878131,122.934020544251));
#54310=CARTESIAN_POINT('Ctrl Pts',(18.1907942060837,-1.29941447755314,122.97087522974));
#54311=CARTESIAN_POINT('Ctrl Pts',(18.9271744385363,-1.25743252782069,123.014848789226));
#54312=CARTESIAN_POINT('Ctrl Pts',(19.5247563273938,-0.832644021409292,
123.058571824615));
#54313=CARTESIAN_POINT('Ctrl Pts',(19.80324675155,-0.158914336827329,123.102046150492));
#54314=CARTESIAN_POINT('Ctrl Pts',(19.681237596879,0.555806024003187,123.145273911019));
#54315=CARTESIAN_POINT('Ctrl Pts',(19.2805996484641,1.00313565776361,123.181093571345));
#54316=CARTESIAN_POINT('Ctrl Pts',(18.8560336820417,1.19200190630298,123.209628597104));
#54317=CARTESIAN_POINT('Ctrl Pts',(18.5248663207615,1.2391334244017,123.230179459196));
#54318=CARTESIAN_POINT('Ctrl Pts',(18.2071745052378,1.19886853894009,123.249887786568));
#54319=CARTESIAN_POINT('Ctrl Pts',(17.826353246682,1.05001593167474,123.275052032664));
#54320=CARTESIAN_POINT('Ctrl Pts',(17.4444385755585,0.695322823220176,123.306391013143));
#54321=CARTESIAN_POINT('Ctrl Pts',(17.2796430128223,0.203571410228621,123.337577098318));
#54322=CARTESIAN_POINT('Ctrl Pts',(17.3005198205283,-0.199770590504172,
123.362435390156));
#54323=CARTESIAN_POINT('Ctrl Pts',(17.4186728528587,-0.584917553785751,
123.38723397063));
#54324=CARTESIAN_POINT('Ctrl Pts',(17.7391439823498,-0.986504330030103,
123.418120743375));
#54325=CARTESIAN_POINT('Ctrl Pts',(18.2575183309786,-1.204406059504,123.451935767405));
#54326=CARTESIAN_POINT('Ctrl Pts',(18.7594894991427,-1.18507959151576,123.482551288236));
#54327=CARTESIAN_POINT('Ctrl Pts',(19.1723107596392,-1.00498843556934,123.510009958442));
#54328=CARTESIAN_POINT('Ctrl Pts',(19.4896744215185,-0.687329613632877,
123.537374781882));
#54329=CARTESIAN_POINT('Ctrl Pts',(19.6684610038165,-0.277235805793136,
123.564647175546));
#54330=CARTESIAN_POINT('Ctrl Pts',(19.6850058219944,0.168442379631604,123.591828854406));
#54331=CARTESIAN_POINT('Ctrl Pts',(19.5380627655275,0.587887775867897,123.618921130316));
#54332=CARTESIAN_POINT('Ctrl Pts',(19.2971766673034,0.867720598171421,123.641425289948));
#54333=CARTESIAN_POINT('Ctrl Pts',(19.0536927608711,1.02670708997575,123.659385419846));
#54334=CARTESIAN_POINT('Ctrl Pts',(18.7409543977456,1.15682572255536,123.68030601116));
#54335=CARTESIAN_POINT('Ctrl Pts',(18.2706071539656,1.1801061135358,123.708616815304));
#54336=CARTESIAN_POINT('Ctrl Pts',(17.8261572337802,0.965650573995201,123.738296470758));
#54337=CARTESIAN_POINT('Ctrl Pts',(17.5648082264945,0.68326279516643,123.761969786547));
#54338=CARTESIAN_POINT('Ctrl Pts',(17.4273072068287,0.430564305475234,123.779689920843));
#54339=CARTESIAN_POINT('Ctrl Pts',(17.3322102326942,0.059145117553956,123.803271515764));
#54340=CARTESIAN_POINT('Ctrl Pts',(17.3871448081339,-0.37709051742884,123.829725176229));
#54341=CARTESIAN_POINT('Ctrl Pts',(17.6434368073176,-0.783983692022225,
123.859023845048));
#54342=CARTESIAN_POINT('Ctrl Pts',(18.0048650575429,-1.05085396041933,123.886417549706));
#54343=CARTESIAN_POINT('Ctrl Pts',(18.4599937002107,-1.16137052462561,123.914827963259));
#54344=CARTESIAN_POINT('Ctrl Pts',(18.9368144658537,-1.07328772322286,123.944247051069));
#54345=CARTESIAN_POINT('Ctrl Pts',(19.3017920039295,-0.821759581235761,
123.97114044685));
#54346=CARTESIAN_POINT('Ctrl Pts',(19.4813108346333,-0.558607347098734,
123.990653830343));
#54347=CARTESIAN_POINT('Ctrl Pts',(19.5808068475382,-0.316073333612912,
124.006894030936));
#54348=CARTESIAN_POINT('Ctrl Pts',(19.629751852434,-0.06998782398746,124.022304363409));
#54349=CARTESIAN_POINT('Ctrl Pts',(19.6031073407298,0.245268476315917,124.041737432005));
#54350=CARTESIAN_POINT('Ctrl Pts',(19.490435145498,0.54037060471732,124.061139593497));
#54351=CARTESIAN_POINT('Ctrl Pts',(19.30075188909,0.792347731402688,124.08051122595));
#54352=CARTESIAN_POINT('Ctrl Pts',(19.049131072318,0.981672676667765,124.099853680021));
#54353=CARTESIAN_POINT('Ctrl Pts',(18.7798028011389,1.08446740519912,124.117558351805));
#54354=CARTESIAN_POINT('Ctrl Pts',(18.5210831823971,1.1153216790555,124.133633467999));
#54355=CARTESIAN_POINT('Ctrl Pts',(18.2099403540505,1.08709601876646,124.152903665108));
#54356=CARTESIAN_POINT('Ctrl Pts',(17.8458847551693,0.930292968214851,124.176955303819));
#54357=CARTESIAN_POINT('Ctrl Pts',(17.5246246286783,0.580601914550535,124.205762463781));
#54358=CARTESIAN_POINT('Ctrl Pts',(17.3744527732723,0.131077359721622,124.234518546367));
#54359=CARTESIAN_POINT('Ctrl Pts',(17.420912508539,-0.33984008099323,124.263226930259));
#54360=CARTESIAN_POINT('Ctrl Pts',(17.6552915800908,-0.750058113066199,
124.29189122665));
#54361=CARTESIAN_POINT('Ctrl Pts',(18.0362401675348,-1.02839061850904,124.320514971321));
#54362=CARTESIAN_POINT('Ctrl Pts',(18.4970485505493,-1.12672401782067,124.349101783714));
#54363=CARTESIAN_POINT('Ctrl Pts',(18.9572956550727,-1.02839086361948,124.377655277085));
#54364=CARTESIAN_POINT('Ctrl Pts',(19.3368462626138,-0.750940541881326,
124.406179103129));
#54365=CARTESIAN_POINT('Ctrl Pts',(19.5697640099691,-0.343039664832534,
124.434676926364));
#54366=CARTESIAN_POINT('Ctrl Pts',(19.6157329190913,0.12405321556001,124.463152433765));
#54367=CARTESIAN_POINT('Ctrl Pts',(19.4670145957621,0.568894309768287,124.491609324847));
#54368=CARTESIAN_POINT('Ctrl Pts',(19.1497451133398,0.914018292969703,124.520051311987));
#54369=CARTESIAN_POINT('Ctrl Pts',(18.7193548376009,1.09938769324324,124.548482116557));
#54370=CARTESIAN_POINT('Ctrl Pts',(18.2509114822612,1.09280765444621,124.576905469337));
#54371=CARTESIAN_POINT('Ctrl Pts',(17.8260645738587,0.895500222610984,124.605325106134));
#54372=CARTESIAN_POINT('Ctrl Pts',(17.5188553213113,0.541878966350906,124.63374476536));
#54373=CARTESIAN_POINT('Ctrl Pts',(17.382850290681,0.093564086594701,124.662168184265));
#54374=CARTESIAN_POINT('Ctrl Pts',(17.4418279527753,-0.37132399975189,124.690599097016));
#54375=CARTESIAN_POINT('Ctrl Pts',(17.6856332696909,-0.771738353190144,
124.719041234205));
#54376=CARTESIAN_POINT('Ctrl Pts',(18.0719208541219,-1.0377941227316,124.747498318936));
#54377=CARTESIAN_POINT('Ctrl Pts',(18.5334880205951,-1.12293055385139,124.775974064255));
#54378=CARTESIAN_POINT('Ctrl Pts',(18.9899319402798,-1.01203632565444,124.804472169489));
#54379=CARTESIAN_POINT('Ctrl Pts',(19.3616153839255,-0.724124170918624,
124.832996318148));
#54380=CARTESIAN_POINT('Ctrl Pts',(19.5835222166062,-0.309081980170988,
124.861550177472));
#54381=CARTESIAN_POINT('Ctrl Pts',(19.6165983611862,0.160946203785086,124.890137394828));
#54382=CARTESIAN_POINT('Ctrl Pts',(19.4546059082149,0.604064532424729,124.918761594942));
#54383=CARTESIAN_POINT('Ctrl Pts',(19.12529087406,0.942854524119908,124.947426376577));
#54384=CARTESIAN_POINT('Ctrl Pts',(18.6856469205026,1.11786424593928,124.976135310182));
#54385=CARTESIAN_POINT('Ctrl Pts',(18.2120799303225,1.09801324094038,125.004891937497));
#54386=CARTESIAN_POINT('Ctrl Pts',(17.7871660062907,0.886096535343215,125.033699768365));
#54387=CARTESIAN_POINT('Ctrl Pts',(17.4852914068756,0.518415965617182,125.062562277764));
#54388=CARTESIAN_POINT('Ctrl Pts',(17.3596644142994,0.058581772485024,125.091482902918));
#54389=CARTESIAN_POINT('Ctrl Pts',(17.4329608753223,-0.413461509346148,
125.120465040703));
#54390=CARTESIAN_POINT('Ctrl Pts',(17.6932446010896,-0.815297582192034,
125.149512047381));
#54391=CARTESIAN_POINT('Ctrl Pts',(18.0958948026965,-1.07639147921999,125.178627235761));
#54392=CARTESIAN_POINT('Ctrl Pts',(18.5712323214369,-1.15044002046434,125.207813872217));
#54393=CARTESIAN_POINT('Ctrl Pts',(19.0365458838211,-1.02356262279525,125.237075174163));
#54394=CARTESIAN_POINT('Ctrl Pts',(19.4104490395663,-0.716886765308683,
125.266414307353));
#54395=CARTESIAN_POINT('Ctrl Pts',(19.6270820726689,-0.283048207401995,
125.295834385718));
#54396=CARTESIAN_POINT('Ctrl Pts',(19.6476857815032,0.202818052033419,125.325338468895));
#54397=CARTESIAN_POINT('Ctrl Pts',(19.4675178551793,0.656058587293851,125.354929559319));
#54398=CARTESIAN_POINT('Ctrl Pts',(19.1168805933481,0.997217593821377,125.384610600053));
#54399=CARTESIAN_POINT('Ctrl Pts',(18.6560450313014,1.16593620672317,125.414384472115));
#54400=CARTESIAN_POINT('Ctrl Pts',(18.1649169151261,1.13160848108037,125.444253994345));
#54401=CARTESIAN_POINT('Ctrl Pts',(17.7292116516687,0.898915887111277,125.474221921416));
#54402=CARTESIAN_POINT('Ctrl Pts',(17.4255249022822,0.507242292692671,125.504290940928));
#54403=CARTESIAN_POINT('Ctrl Pts',(17.3078934945542,0.0240300154227973,
125.53446367174));
#54404=CARTESIAN_POINT('Ctrl Pts',(17.3982001119431,-0.466807092465915,
125.564742661308));
#54405=CARTESIAN_POINT('Ctrl Pts',(17.6821230641009,-0.87942821936793,125.595130385731));
#54406=CARTESIAN_POINT('Ctrl Pts',(18.1113783174984,-1.141051483794,125.625629247964));
#54407=CARTESIAN_POINT('Ctrl Pts',(18.6119087122778,-1.20476940486866,125.656241575366));
#54408=CARTESIAN_POINT('Ctrl Pts',(19.0966360138455,-1.05794126721894,125.686969618127));
#54409=CARTESIAN_POINT('Ctrl Pts',(19.4805851121993,-0.724663367359761,
125.717815547067));
#54410=CARTESIAN_POINT('Ctrl Pts',(19.6957581501257,-0.261839052557402,
125.748781453597));
#54411=CARTESIAN_POINT('Ctrl Pts',(19.7031582372028,0.250515854950012,125.779869348315));
#54412=CARTESIAN_POINT('Ctrl Pts',(19.4998395183547,0.723084549280525,125.811081158878));
#54413=CARTESIAN_POINT('Ctrl Pts',(19.1197116159269,1.07279807162807,125.84241872872));
#54414=CARTESIAN_POINT('Ctrl Pts',(18.627906276719,1.23741873324107,125.873883815249));
#54415=CARTESIAN_POINT('Ctrl Pts',(18.1096368884415,1.1866007561655,125.905478089829));
#54416=CARTESIAN_POINT('Ctrl Pts',(17.6554525278437,0.927464176176284,125.9372031366));
#54417=CARTESIAN_POINT('Ctrl Pts',(17.3454350244466,0.503660979214375,125.969060450953));
#54418=CARTESIAN_POINT('Ctrl Pts',(17.2350938113461,-0.0119586159299856,
126.001051438261));
#54419=CARTESIAN_POINT('Ctrl Pts',(17.3454405769833,-0.529852130208938,
126.033177412798));
#54420=CARTESIAN_POINT('Ctrl Pts',(17.6590169493212,-0.959319950908805,
126.065439597576));
#54421=CARTESIAN_POINT('Ctrl Pts',(18.1226226383629,-1.2243768780413,126.097839123514));
#54422=CARTESIAN_POINT('Ctrl Pts',(18.6563248547008,-1.2771846378208,126.130377028335));
#54423=CARTESIAN_POINT('Ctrl Pts',(19.167226814877,-1.10667254207858,126.163054255594));
#54424=CARTESIAN_POINT('Ctrl Pts',(19.5656267761898,-0.740794449404953,
126.195871654093));
#54425=CARTESIAN_POINT('Ctrl Pts',(19.7807587891991,-0.241970054075206,
126.228829977697));
#54426=CARTESIAN_POINT('Ctrl Pts',(19.7733541251805,0.303551363615882,126.261929884968));
#54427=CARTESIAN_POINT('Ctrl Pts',(19.5427940986679,0.800595193788684,126.295171938242));
#54428=CARTESIAN_POINT('Ctrl Pts',(19.1275540954992,1.16165967036617,126.328556603354));
#54429=CARTESIAN_POINT('Ctrl Pts',(18.5987999963076,1.322315594875,126.362084248977));
#54430=CARTESIAN_POINT('Ctrl Pts',(18.0482010527672,1.25269600798768,126.395755147454));
#54431=CARTESIAN_POINT('Ctrl Pts',(17.5720393499126,0.963030431464114,126.429569473199));
#54432=CARTESIAN_POINT('Ctrl Pts',(17.2543787451364,0.50219434471344,126.463527304884));
#54433=CARTESIAN_POINT('Ctrl Pts',(17.1522183182203,-0.050520473058097,
126.497628620392));
#54434=CARTESIAN_POINT('Ctrl Pts',(17.28528388398,-0.599054499403936,126.531873306385));
#54435=CARTESIAN_POINT('Ctrl Pts',(17.6322269450083,-1.04725813489579,126.566261140912));
#54436=CARTESIAN_POINT('Ctrl Pts',(18.1340686566346,-1.31578098033913,126.600791826669));
#54437=CARTESIAN_POINT('Ctrl Pts',(18.7041317748905,-1.35605913470818,126.635464928542));
#54438=CARTESIAN_POINT('Ctrl Pts',(19.2431776225041,-1.15920835547423,126.670279991304));
#54439=CARTESIAN_POINT('Ctrl Pts',(19.5875030126131,-0.824597610573135,
126.699410261134));
#54440=CARTESIAN_POINT('Ctrl Pts',(19.7634957162678,-0.489016487416052,
126.722784870598));
#54441=CARTESIAN_POINT('Ctrl Pts',(19.8664282376008,-0.123567048111276,
126.746206118278));
#54442=CARTESIAN_POINT('Ctrl Pts',(19.8463416048187,0.359992052614654,126.775570193968));
#54443=CARTESIAN_POINT('Ctrl Pts',(19.5861832716794,0.881849521800832,126.810945948462));
#54444=CARTESIAN_POINT('Ctrl Pts',(19.1338679365761,1.25337686761882,126.846459712541));
#54445=CARTESIAN_POINT('Ctrl Pts',(18.5670443327571,1.40834569449497,126.882110345098));
#54446=CARTESIAN_POINT('Ctrl Pts',(17.9841681512631,1.31793789072804,126.917896712725));
#54447=CARTESIAN_POINT('Ctrl Pts',(17.4871872481259,0.996134996799377,126.953817536565));
#54448=CARTESIAN_POINT('Ctrl Pts',(17.1638036554832,0.497567483767361,126.989871474656));
#54449=CARTESIAN_POINT('Ctrl Pts',(17.0719279933258,-0.091745800871305,
127.026057079263));
#54450=CARTESIAN_POINT('Ctrl Pts',(17.2293359710647,-0.669255689424998,
127.062372821794));
#54451=CARTESIAN_POINT('Ctrl Pts',(17.610241253734,-1.13374033526755,127.098817081293));
#54452=CARTESIAN_POINT('Ctrl Pts',(18.1495133445035,-1.4030660398855,127.135388152441));
#54453=CARTESIAN_POINT('Ctrl Pts',(18.7538151252911,-1.42872296525937,127.172084240549));
#54454=CARTESIAN_POINT('Ctrl Pts',(19.3177758940829,-1.20456511272855,127.208903469833));
#54455=CARTESIAN_POINT('Ctrl Pts',(19.7423836723087,-0.768176629582259,
127.245843874445));
#54456=CARTESIAN_POINT('Ctrl Pts',(19.9523892723162,-0.194574417684047,
127.282903420998));
#54457=CARTESIAN_POINT('Ctrl Pts',(19.9096554818046,0.416699120440095,127.320079963011));
#54458=CARTESIAN_POINT('Ctrl Pts',(19.6200821414386,0.958872434979693,127.357371346452));
#54459=CARTESIAN_POINT('Ctrl Pts',(19.1328479733187,1.33661667025399,127.394775187569));
#54460=CARTESIAN_POINT('Ctrl Pts',(18.5320571866121,1.4828332255706,127.432289321894));
#54461=CARTESIAN_POINT('Ctrl Pts',(17.9221948628147,1.37057956323489,127.469910942846));
#54462=CARTESIAN_POINT('Ctrl Pts',(17.4099532468711,1.01803725495168,127.507638323144));
#54463=CARTESIAN_POINT('Ctrl Pts',(17.0854953400889,0.485568884820926,127.545467204649));
#54464=CARTESIAN_POINT('Ctrl Pts',(17.006625668042,-0.134612140505952,127.583398399533));
#54465=CARTESIAN_POINT('Ctrl Pts',(17.188418776128,-0.734467438014115,127.621422779654));
#54466=CARTESIAN_POINT('Ctrl Pts',(17.6003366822749,-1.20887205801102,127.65954828209));
#54467=CARTESIAN_POINT('Ctrl Pts',(18.1716172541843,-1.47441118975859,127.69775474856));
#54468=CARTESIAN_POINT('Ctrl Pts',(18.8027604208616,-1.4832332174758,127.736069375441));
#54469=CARTESIAN_POINT('Ctrl Pts',(19.3838788005284,-1.23337426230525,127.774432416617));
#54470=CARTESIAN_POINT('Ctrl Pts',(19.8136026224869,-0.766189668421221,
127.812941446107));
#54471=CARTESIAN_POINT('Ctrl Pts',(20.0138145362224,-0.163792158425567,
127.851457167091));
#54472=CARTESIAN_POINT('Ctrl Pts',(19.9641501694412,0.363252169813094,127.883623693518));
#54473=CARTESIAN_POINT('Ctrl Pts',(19.79432217284,0.747620422811712,127.909505070839));
#54474=CARTESIAN_POINT('Ctrl Pts',(19.608996542054,1.00226608921801,127.928824308732));
#54475=CARTESIAN_POINT('Ctrl Pts',(19.3768569389481,1.21253337912636,127.948129329567));
#54476=CARTESIAN_POINT('Ctrl Pts',(19.108950972945,1.36963666110103,127.967545832416));
#54477=CARTESIAN_POINT('Ctrl Pts',(18.813603063098,1.46669294355822,127.98706761261));
#54478=CARTESIAN_POINT('Ctrl Pts',(18.6035448089217,1.48910415722868,127.999941776888));
#54479=CARTESIAN_POINT('Ctrl Pts',(18.4960527730771,1.49000887282122,128.006304968607));
#54480=CARTESIAN_POINT('Ctrl Pts',(18.49651553697,1.50499871401635,112.870284331898));
#54481=CARTESIAN_POINT('Ctrl Pts',(18.3336126008743,1.50362762800833,112.87992767523));
#54482=CARTESIAN_POINT('Ctrl Pts',(18.1233704382878,1.47030778167341,112.893035123571));
#54483=CARTESIAN_POINT('Ctrl Pts',(17.8312017734791,1.35658915071029,112.91277539402));
#54484=CARTESIAN_POINT('Ctrl Pts',(17.6051956153995,1.22416527432542,112.929156901125));
#54485=CARTESIAN_POINT('Ctrl Pts',(17.3699687728766,1.01106353608856,112.948717313545));
#54486=CARTESIAN_POINT('Ctrl Pts',(17.1818898541377,0.752733756695092,112.968320038741));
#54487=CARTESIAN_POINT('Ctrl Pts',(17.0092492859105,0.36200183096875,112.99462963671));
#54488=CARTESIAN_POINT('Ctrl Pts',(16.9586044369231,-0.174255285116374,
113.027359456216));
#54489=CARTESIAN_POINT('Ctrl Pts',(17.1626159288063,-0.788555902752346,
113.066633020249));
#54490=CARTESIAN_POINT('Ctrl Pts',(17.6017111768839,-1.26616594937551,113.105992819481));
#54491=CARTESIAN_POINT('Ctrl Pts',(18.1967581723796,-1.52214677887222,113.14527795291));
#54492=CARTESIAN_POINT('Ctrl Pts',(18.844504423364,-1.51325397885606,113.184601044115));
#54493=CARTESIAN_POINT('Ctrl Pts',(19.4320735597648,-1.24028824537934,113.223892539239));
#54494=CARTESIAN_POINT('Ctrl Pts',(19.8566981334926,-0.751475885302668,
113.263184243726));
#54495=CARTESIAN_POINT('Ctrl Pts',(20.0445669595258,-0.132045477816717,
113.302451626346));
#54496=CARTESIAN_POINT('Ctrl Pts',(19.9630909675482,0.509755478278449,113.341704280326));
#54497=CARTESIAN_POINT('Ctrl Pts',(19.6267635243402,1.0619677779827,113.380930598247));
#54498=CARTESIAN_POINT('Ctrl Pts',(19.0945974730579,1.42839035694035,113.420131303187));
#54499=CARTESIAN_POINT('Ctrl Pts',(18.4596682384706,1.54539663475943,113.459300732061));
#54500=CARTESIAN_POINT('Ctrl Pts',(17.8328788987336,1.39299167988022,113.498436286584));
#54501=CARTESIAN_POINT('Ctrl Pts',(17.3234976520339,0.998246828811687,113.537533977322));
#54502=CARTESIAN_POINT('Ctrl Pts',(17.0201012712623,0.43047223212316,113.576590529082));
#54503=CARTESIAN_POINT('Ctrl Pts',(16.9751265156656,-0.210968557547024,
113.615602351298));
#54504=CARTESIAN_POINT('Ctrl Pts',(17.1958026171018,-0.814087468865364,
113.654566025983));
#54505=CARTESIAN_POINT('Ctrl Pts',(17.6429797818494,-1.27385693352479,113.693478165596));
#54506=CARTESIAN_POINT('Ctrl Pts',(18.2381149235038,-1.51053956043059,113.732335298242));
#54507=CARTESIAN_POINT('Ctrl Pts',(18.8770399010279,-1.48353546536932,113.77113426794));
#54508=CARTESIAN_POINT('Ctrl Pts',(19.4483164054444,-1.19836309525062,113.809871477796));
#54509=CARTESIAN_POINT('Ctrl Pts',(19.8525979010098,-0.705553496904467,
113.848543962768));
#54510=CARTESIAN_POINT('Ctrl Pts',(20.0200408180881,-0.0916935590501383,
113.887148305216));
#54511=CARTESIAN_POINT('Ctrl Pts',(19.9223241392787,0.535881741945536,113.925681414906));
#54512=CARTESIAN_POINT('Ctrl Pts',(19.5774635624247,1.06775101120009,113.96414018534));
#54513=CARTESIAN_POINT('Ctrl Pts',(19.0465046155246,1.41172133274227,114.002521454301));
#54514=CARTESIAN_POINT('Ctrl Pts',(18.526648067714,1.49238331075636,114.034438886814));
#54515=CARTESIAN_POINT('Ctrl Pts',(18.1188516957653,1.42559012849739,114.059931011469));
#54516=CARTESIAN_POINT('Ctrl Pts',(17.7340973408627,1.27603701185301,114.085394830966));
#54517=CARTESIAN_POINT('Ctrl Pts',(17.329286118754,0.94373241691892,114.117170806693));
#54518=CARTESIAN_POINT('Ctrl Pts',(17.049492258478,0.382568260031224,114.155212625842));
#54519=CARTESIAN_POINT('Ctrl Pts',(17.0233344994864,-0.242377855811677,
114.193162521077));
#54520=CARTESIAN_POINT('Ctrl Pts',(17.2541617793634,-0.822071654025293,
114.231017692788));
#54521=CARTESIAN_POINT('Ctrl Pts',(17.7004709588697,-1.25579236892624,114.268775475679));
#54522=CARTESIAN_POINT('Ctrl Pts',(18.2834652007333,-1.46882945434736,114.306433293321));
#54523=CARTESIAN_POINT('Ctrl Pts',(18.9009375287065,-1.42527515643007,114.343988609376));
#54524=CARTESIAN_POINT('Ctrl Pts',(19.4452400385389,-1.13413243348152,114.381438939098));
#54525=CARTESIAN_POINT('Ctrl Pts',(19.8220671838761,-0.647455723515675,
114.418781942662));
#54526=CARTESIAN_POINT('Ctrl Pts',(19.9668177841584,-0.0510774300832363,
114.456015241884));
#54527=CARTESIAN_POINT('Ctrl Pts',(19.855686038565,0.550611907288274,114.493136645638));
#54528=CARTESIAN_POINT('Ctrl Pts',(19.5095622696879,1.05286323816987,114.530143966639));
#54529=CARTESIAN_POINT('Ctrl Pts',(18.9901066793641,1.36894922551202,114.567035111385));
#54530=CARTESIAN_POINT('Ctrl Pts',(18.3887907442047,1.4450452249503,114.603808080057));
#54531=CARTESIAN_POINT('Ctrl Pts',(17.810731402714,1.26947343893433,114.640460935603));
#54532=CARTESIAN_POINT('Ctrl Pts',(17.3563198980319,0.874426270620376,114.676991833415));
#54533=CARTESIAN_POINT('Ctrl Pts',(17.1037586025035,0.330076715915367,114.713399007585));
#54534=CARTESIAN_POINT('Ctrl Pts',(17.0955891084954,-0.267878922353754,
114.74968077348));
#54535=CARTESIAN_POINT('Ctrl Pts',(17.3315462787181,-0.815111405623883,
114.785835540599));
#54536=CARTESIAN_POINT('Ctrl Pts',(17.7688643629591,-1.2167760559352,114.821861785405));
#54537=CARTESIAN_POINT('Ctrl Pts',(18.3300985159098,-1.40416354888984,114.857758110311));
#54538=CARTESIAN_POINT('Ctrl Pts',(18.8189384921563,-1.35575323505928,114.887562293732));
#54539=CARTESIAN_POINT('Ctrl Pts',(19.1716912067797,-1.20042508413519,114.911339401126));
#54540=CARTESIAN_POINT('Ctrl Pts',(19.4840903420183,-0.975859670364661,
114.935072168859));
#54541=CARTESIAN_POINT('Ctrl Pts',(19.7716878728692,-0.582133605641874,
114.964654504561));
#54542=CARTESIAN_POINT('Ctrl Pts',(19.8931529911131,-0.0120119416229624,
115.000018638428));
#54543=CARTESIAN_POINT('Ctrl Pts',(19.7716793443981,0.555774460771906,115.035247022951));
#54544=CARTESIAN_POINT('Ctrl Pts',(19.4301928094659,1.02262655518765,115.07033883131));
#54545=CARTESIAN_POINT('Ctrl Pts',(18.9297825002282,1.30814522073825,115.105293244196));
#54546=CARTESIAN_POINT('Ctrl Pts',(18.3586637335548,1.36416104789949,115.140109582566));
#54547=CARTESIAN_POINT('Ctrl Pts',(17.816632406542,1.18272719467699,115.17478723275));
#54548=CARTESIAN_POINT('Ctrl Pts',(17.3976999462254,0.797309431344444,115.209325696987));
#54549=CARTESIAN_POINT('Ctrl Pts',(17.1735784716011,0.276454513248407,115.243724548093));
#54550=CARTESIAN_POINT('Ctrl Pts',(17.1809199116676,-0.22536964366726,115.274176940408));
#54551=CARTESIAN_POINT('Ctrl Pts',(17.3354710467395,-0.629195288576481,
115.300731925094));
#54552=CARTESIAN_POINT('Ctrl Pts',(17.502022403867,-0.850655511550889,115.31775626652));
#54553=CARTESIAN_POINT('Ctrl Pts',(17.6358232956015,-0.975224668920173,
115.329086323583));
#54554=CARTESIAN_POINT('Ctrl Pts',(17.7067764065314,-1.03268658588934,115.334747457085));
#54555=CARTESIAN_POINT('Ctrl Pts',(17.7816008739847,-1.08494819346858,115.340404694511));
#54556=CARTESIAN_POINT('Ctrl Pts',(17.9380013948717,-1.17876364558541,115.351711369109));
#54557=CARTESIAN_POINT('Ctrl Pts',(18.1955706816015,-1.27700122758528,115.368642182192));
#54558=CARTESIAN_POINT('Ctrl Pts',(18.5607517830549,-1.30775052484681,115.391154193319));
#54559=CARTESIAN_POINT('Ctrl Pts',(18.9192839923125,-1.23635697638592,115.413603956782));
#54560=CARTESIAN_POINT('Ctrl Pts',(19.24295722527,-1.06902914440793,115.435991388812));
#54561=CARTESIAN_POINT('Ctrl Pts',(19.5072304818416,-0.819230463869382,
115.458316697458));
#54562=CARTESIAN_POINT('Ctrl Pts',(19.690959734946,-0.507076536075454,115.480579842894));
#54563=CARTESIAN_POINT('Ctrl Pts',(19.8121732723121,-0.0402072384437589,
115.51018141997));
#54564=CARTESIAN_POINT('Ctrl Pts',(19.7291627781261,0.446553891594026,115.53965926837));
#54565=CARTESIAN_POINT('Ctrl Pts',(19.4957563328109,0.793998696574734,115.565344565252));
#54566=CARTESIAN_POINT('Ctrl Pts',(19.3263627711921,0.959025218074687,115.579991285573));
#54567=CARTESIAN_POINT('Ctrl Pts',(19.1353328686529,1.09850403796305,115.594617483237));
#54568=CARTESIAN_POINT('Ctrl Pts',(18.9457036306386,1.18342968358787,115.607388621145));
#54569=CARTESIAN_POINT('Ctrl Pts',(18.7746135630278,1.22619954854511,115.618316371275));
#54570=CARTESIAN_POINT('Ctrl Pts',(18.6879200730088,1.24156918634862,115.623776397083));
#54571=CARTESIAN_POINT('Ctrl Pts',(18.6149671512159,1.24929495538121,115.628323271269));
#54572=CARTESIAN_POINT('Ctrl Pts',(18.5564232901343,1.25232080760023,115.631958822256));
#54573=CARTESIAN_POINT('Ctrl Pts',(18.3188555044749,1.25686234907179,115.646698035442));
#54574=CARTESIAN_POINT('Ctrl Pts',(17.8888715430467,1.14680181043036,115.673379735934));
#54575=CARTESIAN_POINT('Ctrl Pts',(17.5243082161196,0.808308860592351,115.703303215303));
#54576=CARTESIAN_POINT('Ctrl Pts',(17.3625257033883,0.50390079334422,115.72460706276));
#54577=CARTESIAN_POINT('Ctrl Pts',(17.3075338582628,0.340949365208199,115.735241634511));
#54578=CARTESIAN_POINT('Ctrl Pts',(17.2805316366918,0.206509233398448,115.743738908119));
#54579=CARTESIAN_POINT('Ctrl Pts',(17.2483095255158,-0.0656048243204948,
115.760719371947));
#54580=CARTESIAN_POINT('Ctrl Pts',(17.3281117828854,-0.516084464963803,
115.788234052639));
#54581=CARTESIAN_POINT('Ctrl Pts',(17.7215430539041,-1.00896792873564,115.826146275045));
#54582=CARTESIAN_POINT('Ctrl Pts',(18.2516949275413,-1.2318489526899,115.860731644079));
#54583=CARTESIAN_POINT('Ctrl Pts',(18.765074033174,-1.21206507972195,115.892041349858));
#54584=CARTESIAN_POINT('Ctrl Pts',(19.1871807387752,-1.02791702813592,115.9201196661));
#54585=CARTESIAN_POINT('Ctrl Pts',(19.5117099232347,-0.703109660480611,
115.94809877643));
#54586=CARTESIAN_POINT('Ctrl Pts',(19.6639431963501,-0.353759299179872,
115.971332775432));
#54587=CARTESIAN_POINT('Ctrl Pts',(19.7029577450344,-0.0560681711860727,
115.989871790982));
#54588=CARTESIAN_POINT('Ctrl Pts',(19.6903956065854,0.168277428115539,116.003751582154));
#54589=CARTESIAN_POINT('Ctrl Pts',(19.6453583039838,0.349777156774072,116.01529861874));
#54590=CARTESIAN_POINT('Ctrl Pts',(19.5896345786186,0.487827454310805,116.024524180344));
#54591=CARTESIAN_POINT('Ctrl Pts',(19.4873268530305,0.686149792199375,116.038350531065));
#54592=CARTESIAN_POINT('Ctrl Pts',(19.2657788090282,0.94342374801498,116.059046301773));
#54593=CARTESIAN_POINT('Ctrl Pts',(18.8668133161929,1.15412635411037,116.086547373941));
#54594=CARTESIAN_POINT('Ctrl Pts',(18.4199331148969,1.20433642524023,116.113957070661));
#54595=CARTESIAN_POINT('Ctrl Pts',(18.0952779029817,1.11723399930278,116.134446884645));
#54596=CARTESIAN_POINT('Ctrl Pts',(17.9017889644904,1.01249991695947,116.148079023699));
#54597=CARTESIAN_POINT('Ctrl Pts',(17.7799369999649,0.93110838138898,116.157159621741));
#54598=CARTESIAN_POINT('Ctrl Pts',(17.5882472578648,0.759856044959128,116.173032149632));
#54599=CARTESIAN_POINT('Ctrl Pts',(17.4598618042694,0.5557237355446,116.187734998419));
#54600=CARTESIAN_POINT('Ctrl Pts',(17.3974802528664,0.384644782920287,116.199025088643));
#54601=CARTESIAN_POINT('Ctrl Pts',(17.3811086459147,0.332571473631556,116.202410852429));
#54602=CARTESIAN_POINT('Ctrl Pts',(17.3672458383465,0.27977617854763,116.205795247183));
#54603=CARTESIAN_POINT('Ctrl Pts',(17.3558537656234,0.226430775875569,116.209178339773));
#54604=CARTESIAN_POINT('Ctrl Pts',(17.3469543264664,0.172623320191819,116.212560079634));
#54605=CARTESIAN_POINT('Ctrl Pts',(17.3385176348533,0.100437721270174,116.217067299795));
#54606=CARTESIAN_POINT('Ctrl Pts',(17.3290322213833,-0.0992654325487338,
116.229454683121));
#54607=CARTESIAN_POINT('Ctrl Pts',(17.3908483892394,-0.425368273174374,
116.249686405889));
#54608=CARTESIAN_POINT('Ctrl Pts',(17.6256909219847,-0.79889129542694,116.276579485812));
#54609=CARTESIAN_POINT('Ctrl Pts',(17.9796947676307,-1.06001015743842,116.303392710883));
#54610=CARTESIAN_POINT('Ctrl Pts',(18.4034077753438,-1.17341375372982,116.330127316022));
#54611=CARTESIAN_POINT('Ctrl Pts',(18.8379681316464,-1.12433617754085,116.356785513166));
#54612=CARTESIAN_POINT('Ctrl Pts',(19.2235542763837,-0.92044124263072,116.383368803318));
#54613=CARTESIAN_POINT('Ctrl Pts',(19.4440554391474,-0.663980494317338,
116.403988454749));
#54614=CARTESIAN_POINT('Ctrl Pts',(19.5497056653311,-0.451252453324442,
116.418690018913));
#54615=CARTESIAN_POINT('Ctrl Pts',(19.6122761625615,-0.272121955888386,
116.430441476114));
#54616=CARTESIAN_POINT('Ctrl Pts',(19.6624926907458,0.0578739594259051,
116.450978681812));
#54617=CARTESIAN_POINT('Ctrl Pts',(19.5541359914442,0.532226076482499,116.480242353973));
#54618=CARTESIAN_POINT('Ctrl Pts',(19.1686764482267,0.968561647204002,116.515242131433));
#54619=CARTESIAN_POINT('Ctrl Pts',(18.6234304609746,1.16678220457797,116.550130731072));
#54620=CARTESIAN_POINT('Ctrl Pts',(18.0513874432561,1.08037506712942,116.58491296496));
#54621=CARTESIAN_POINT('Ctrl Pts',(17.6588194184233,0.782699663211421,116.614536530482));
#54622=CARTESIAN_POINT('Ctrl Pts',(17.4566975083438,0.43862940460328,116.639049224404));
#54623=CARTESIAN_POINT('Ctrl Pts',(17.3504735057365,0.0302010042763518,
116.664964912131));
#54624=CARTESIAN_POINT('Ctrl Pts',(17.441318190632,-0.504074055082703,116.697288303009));
#54625=CARTESIAN_POINT('Ctrl Pts',(17.8738322445769,-0.98766591140209,116.735970603409));
#54626=CARTESIAN_POINT('Ctrl Pts',(18.4956494809416,-1.16653777136026,116.774554938272));
#54627=CARTESIAN_POINT('Ctrl Pts',(19.1158561890266,-0.987678591541207,
116.813049296759));
#54628=CARTESIAN_POINT('Ctrl Pts',(19.5451029837921,-0.507162506325275,
116.851462000512));
#54629=CARTESIAN_POINT('Ctrl Pts',(19.6344500864472,0.0209568317628616,
116.883411031743));
#54630=CARTESIAN_POINT('Ctrl Pts',(19.529835344982,0.423259543631477,116.908938003123));
#54631=CARTESIAN_POINT('Ctrl Pts',(19.3719778191083,0.69166285162635,116.928067552668));
#54632=CARTESIAN_POINT('Ctrl Pts',(19.1455454752817,0.905164315225213,116.947183404083));
#54633=CARTESIAN_POINT('Ctrl Pts',(18.7774209857398,1.09622260692838,116.972653115984));
#54634=CARTESIAN_POINT('Ctrl Pts',(18.2449951046063,1.12623059429594,117.004460418568));
#54635=CARTESIAN_POINT('Ctrl Pts',(17.6853267542694,0.816754701388943,117.042589105265));
#54636=CARTESIAN_POINT('Ctrl Pts',(17.3763805857206,0.25760776168484,117.080686636608));
#54637=CARTESIAN_POINT('Ctrl Pts',(17.4122036778926,-0.379923978041567,
117.118761454777));
#54638=CARTESIAN_POINT('Ctrl Pts',(17.7815850748894,-0.900446847787842,
117.156822292918));
#54639=CARTESIAN_POINT('Ctrl Pts',(18.3711855462016,-1.14467562030106,117.194877755412));
#54640=CARTESIAN_POINT('Ctrl Pts',(19.0004142784978,-1.03777979468232,117.232936530983));
#54641=CARTESIAN_POINT('Ctrl Pts',(19.4764865869262,-0.612388047726278,
117.271007271204));
#54642=CARTESIAN_POINT('Ctrl Pts',(19.6533828286409,0.0014177969022171,
117.309098626614));
#54643=CARTESIAN_POINT('Ctrl Pts',(19.4764842231535,0.615731147059621,117.347219206504));
#54644=CARTESIAN_POINT('Ctrl Pts',(18.9994059623802,1.04220793738651,117.385377605214));
#54645=CARTESIAN_POINT('Ctrl Pts',(18.3677905909605,1.14964530042269,117.423582363643));
#54646=CARTESIAN_POINT('Ctrl Pts',(17.7749675945259,0.904241094560212,117.461841957937));
#54647=CARTESIAN_POINT('Ctrl Pts',(17.4029459302078,0.380199033566501,117.500164805045));
#54648=CARTESIAN_POINT('Ctrl Pts',(17.3666607130067,-0.26264953413493,117.53855925612));
#54649=CARTESIAN_POINT('Ctrl Pts',(17.6785947502515,-0.827443121223426,
117.577033557529));
#54650=CARTESIAN_POINT('Ctrl Pts',(18.2444674988179,-1.14045467464445,117.615595868649));
#54651=CARTESIAN_POINT('Ctrl Pts',(18.8917850917382,-1.10432648074206,117.654254235677));
#54652=CARTESIAN_POINT('Ctrl Pts',(19.4220254974689,-0.728402023842326,
117.693016621745));
#54653=CARTESIAN_POINT('Ctrl Pts',(19.6718587015237,-0.126164954214387,
117.731890784944));
#54654=CARTESIAN_POINT('Ctrl Pts',(19.5806405630026,0.411019352712336,117.764385541049));
#54655=CARTESIAN_POINT('Ctrl Pts',(19.3441675709589,0.763295298332512,117.790444769066));
#54656=CARTESIAN_POINT('Ctrl Pts',(19.0201301369936,1.03823903341511,117.816547739909));
#54657=CARTESIAN_POINT('Ctrl Pts',(18.493178198775,1.19052995092288,117.849260188486));
#54658=CARTESIAN_POINT('Ctrl Pts',(17.8581591562469,1.00786619563251,117.888656951998));
#54659=CARTESIAN_POINT('Ctrl Pts',(17.4160248614217,0.51366844782423,117.928202267748));
#54660=CARTESIAN_POINT('Ctrl Pts',(17.3041141976344,-0.142668645446928,
117.967903170292));
#54661=CARTESIAN_POINT('Ctrl Pts',(17.5595850207467,-0.760412353891034,
118.007766241407));
#54662=CARTESIAN_POINT('Ctrl Pts',(18.1068550165682,-1.1492371242961,118.04779801726));
#54663=CARTESIAN_POINT('Ctrl Pts',(18.7800314200528,-1.18744473707504,118.088004749543));
#54664=CARTESIAN_POINT('Ctrl Pts',(19.3730344071082,-0.860233663725908,
118.128392532671));
#54665=CARTESIAN_POINT('Ctrl Pts',(19.7025519711489,-0.26486780951679,118.168967176754));
#54666=CARTESIAN_POINT('Ctrl Pts',(19.6647053513366,0.417645340336696,118.209734371169));
#54667=CARTESIAN_POINT('Ctrl Pts',(19.267503779961,0.978374259812269,118.250699402105));
#54668=CARTESIAN_POINT('Ctrl Pts',(18.7362494566518,1.19864104439097,118.285006242352));
#54669=CARTESIAN_POINT('Ctrl Pts',(18.2877057344592,1.18528122231896,118.312555556409));
#54670=CARTESIAN_POINT('Ctrl Pts',(17.9664308123881,1.08327575222911,118.333270290751));
#54671=CARTESIAN_POINT('Ctrl Pts',(17.6852323698027,0.895287772551696,118.354037962367));
#54672=CARTESIAN_POINT('Ctrl Pts',(17.4664950224042,0.636435219092414,118.374859570174));
#54673=CARTESIAN_POINT('Ctrl Pts',(17.3276081719734,0.326162075674822,118.39573521112));
#54674=CARTESIAN_POINT('Ctrl Pts',(17.2799229603302,-0.0111919817315693,
118.41666582645));
#54675=CARTESIAN_POINT('Ctrl Pts',(17.327598035555,-0.349579187274582,118.437651539655));
#54676=CARTESIAN_POINT('Ctrl Pts',(17.4441956547223,-0.610077653010874,
118.455186324647));
#54677=CARTESIAN_POINT('Ctrl Pts',(17.5782188017048,-0.793582078732169,
118.469242010708));
#54678=CARTESIAN_POINT('Ctrl Pts',(17.7368454389062,-0.956441180317881,
118.483316881728));
#54679=CARTESIAN_POINT('Ctrl Pts',(18.0705782583969,-1.18054323096259,118.507997048192));
#54680=CARTESIAN_POINT('Ctrl Pts',(18.6554412304203,-1.28059964969612,118.543397636231));
#54681=CARTESIAN_POINT('Ctrl Pts',(19.3177414533384,-1.00686280515393,118.586110181979));
#54682=CARTESIAN_POINT('Ctrl Pts',(19.6650536664888,-0.517774642787662,
118.621899795047));
#54683=CARTESIAN_POINT('Ctrl Pts',(19.7442788642631,-0.115645277500642,
118.6470566672));
#54684=CARTESIAN_POINT('Ctrl Pts',(19.7411794524541,0.116933901702342,118.661461743122));
#54685=CARTESIAN_POINT('Ctrl Pts',(19.7054157650643,0.347518370662662,118.675886972296));
#54686=CARTESIAN_POINT('Ctrl Pts',(19.6003745425333,0.622016252827566,118.693955916805));
#54687=CARTESIAN_POINT('Ctrl Pts',(19.317257629013,0.99995885328799,118.722946752854));
#54688=CARTESIAN_POINT('Ctrl Pts',(18.7836518879622,1.29558280479233,118.759336777127));
#54689=CARTESIAN_POINT('Ctrl Pts',(18.0482527405502,1.2548599580439,118.803249169655));
#54690=CARTESIAN_POINT('Ctrl Pts',(17.4439365823436,0.826778385158046,118.847407475872));
#54691=CARTESIAN_POINT('Ctrl Pts',(17.2061922029869,0.253734869760506,118.884412115397));
#54692=CARTESIAN_POINT('Ctrl Pts',(17.2206748920695,-0.230259004950036,
118.914139911465));
#54693=CARTESIAN_POINT('Ctrl Pts',(17.3122772963604,-0.519205211008821,
118.932771615628));
#54694=CARTESIAN_POINT('Ctrl Pts',(17.4173179411385,-0.702637921404735,
118.945841005029));
#54695=CARTESIAN_POINT('Ctrl Pts',(17.4876798042075,-0.800486720086772,
118.953317008868));
#54696=CARTESIAN_POINT('Ctrl Pts',(17.564941377458,-0.89325038450052,118.960798213382));
#54697=CARTESIAN_POINT('Ctrl Pts',(17.6733776392394,-0.998701561839941,
118.970159456938));
#54698=CARTESIAN_POINT('Ctrl Pts',(17.869064246506,-1.1417814231385,118.985158206556));
#54699=CARTESIAN_POINT('Ctrl Pts',(18.1482054520686,-1.26678297579892,119.003945578663));
#54700=CARTESIAN_POINT('Ctrl Pts',(18.512660466752,-1.31830065871435,119.026552828765));
#54701=CARTESIAN_POINT('Ctrl Pts',(18.8781159084707,-1.26677700093841,119.049222381195));
#54702=CARTESIAN_POINT('Ctrl Pts',(19.2159631951799,-1.11568341872246,119.07195433768));
#54703=CARTESIAN_POINT('Ctrl Pts',(19.4995484771516,-0.876304025124276,
119.094748533567));
#54704=CARTESIAN_POINT('Ctrl Pts',(19.7063441509456,-0.566943680968072,
119.11760507113));
#54705=CARTESIAN_POINT('Ctrl Pts',(19.8197309451019,-0.211442999295146,
119.140523685235));
#54706=CARTESIAN_POINT('Ctrl Pts',(19.8302792102411,0.162535549658454,119.163504530996));
#54707=CARTESIAN_POINT('Ctrl Pts',(19.7522781137547,0.465296426729761,119.182706741));
#54708=CARTESIAN_POINT('Ctrl Pts',(19.6410989464218,0.687817901944263,119.19809956578));
#54709=CARTESIAN_POINT('Ctrl Pts',(19.4647313674719,0.944433947569229,119.217366235714));
#54710=CARTESIAN_POINT('Ctrl Pts',(19.1203100782122,1.22737777491237,119.244411622083));
#54711=CARTESIAN_POINT('Ctrl Pts',(18.5652296939497,1.37913493579527,119.279322521792));
#54712=CARTESIAN_POINT('Ctrl Pts',(17.9943789266596,1.29059989009301,119.314371048622));
#54713=CARTESIAN_POINT('Ctrl Pts',(17.5075663391158,0.975396843352528,119.349556416458));
#54714=CARTESIAN_POINT('Ctrl Pts',(17.1907406802648,0.486956739770124,119.38487780746));
#54715=CARTESIAN_POINT('Ctrl Pts',(17.1007177860647,-0.0904629952018157,
119.420334217929));
#54716=CARTESIAN_POINT('Ctrl Pts',(17.2549451352662,-0.656474628556876,
119.455924718063));
#54717=CARTESIAN_POINT('Ctrl Pts',(17.5661243855808,-1.03583821018366,119.485694096377));
#54718=CARTESIAN_POINT('Ctrl Pts',(17.8926570460436,-1.24382698529492,119.509575590226));
#54719=CARTESIAN_POINT('Ctrl Pts',(18.2558106009391,-1.37997354885633,119.533500603368));
#54720=CARTESIAN_POINT('Ctrl Pts',(18.7496196816727,-1.40102252601465,119.563488460007));
#54721=CARTESIAN_POINT('Ctrl Pts',(19.302802351283,-1.1811288001459,119.599602804378));
#54722=CARTESIAN_POINT('Ctrl Pts',(19.7193843468129,-0.753024059784299,
119.635844665495));
#54723=CARTESIAN_POINT('Ctrl Pts',(19.9254897572766,-0.190124415181504,
119.672212430828));
#54724=CARTESIAN_POINT('Ctrl Pts',(19.8835551265898,0.409891451814051,119.708704471057));
#54725=CARTESIAN_POINT('Ctrl Pts',(19.5992582389472,0.942231735537137,119.745319028385));
#54726=CARTESIAN_POINT('Ctrl Pts',(19.120735909551,1.31324454186643,119.782054298589));
#54727=CARTESIAN_POINT('Ctrl Pts',(18.5305348998093,1.45689202451587,119.818908350599));
#54728=CARTESIAN_POINT('Ctrl Pts',(17.9311917661294,1.34662904570844,119.855879245505));
#54729=CARTESIAN_POINT('Ctrl Pts',(17.5116220005748,1.05780154061175,119.886783901806));
#54730=CARTESIAN_POINT('Ctrl Pts',(17.2681007112558,0.738313939272634,119.911563959347));
#54731=CARTESIAN_POINT('Ctrl Pts',(17.0957154156509,0.374823924233557,119.936381231006));
#54732=CARTESIAN_POINT('Ctrl Pts',(17.0309927941948,-0.133517822775856,
119.967471718131));
#54733=CARTESIAN_POINT('Ctrl Pts',(17.2098570169801,-0.723745817563428,
120.004888433649));
#54734=CARTESIAN_POINT('Ctrl Pts',(17.6153203269838,-1.19074555891921,120.042410870425));
#54735=CARTESIAN_POINT('Ctrl Pts',(18.1777197790016,-1.45213042815002,120.080036611004));
#54736=CARTESIAN_POINT('Ctrl Pts',(18.7994854721492,-1.46102141363347,120.11776312502));
#54737=CARTESIAN_POINT('Ctrl Pts',(19.3721419323586,-1.21453953940101,120.155587847869));
#54738=CARTESIAN_POINT('Ctrl Pts',(19.7952400432308,-0.754491980125082,
120.193508128623));
#54739=CARTESIAN_POINT('Ctrl Pts',(19.9940145933377,-0.160304321379954,
120.231521263177));
#54740=CARTESIAN_POINT('Ctrl Pts',(19.9326093252334,0.464726279580436,120.269624478708));
#54741=CARTESIAN_POINT('Ctrl Pts',(19.620552160879,1.01140912119698,120.307814943475));
#54742=CARTESIAN_POINT('Ctrl Pts',(19.1112964283598,1.38377060349613,120.34608976467));
#54743=CARTESIAN_POINT('Ctrl Pts',(18.493054159353,1.51592840621915,120.384445993232));
#54744=CARTESIAN_POINT('Ctrl Pts',(17.8734911230083,1.38376736011695,120.422880625353));
#54745=CARTESIAN_POINT('Ctrl Pts',(17.3609452757673,1.00933886152342,120.461390604502));
#54746=CARTESIAN_POINT('Ctrl Pts',(17.0454493832622,0.457183766611044,120.499972821949));
#54747=CARTESIAN_POINT('Ctrl Pts',(16.9828884983602,-0.176810342706842,
120.5386241196));
#54748=CARTESIAN_POINT('Ctrl Pts',(17.1850847559295,-0.782090219748437,
120.577341292721));
#54749=CARTESIAN_POINT('Ctrl Pts',(17.617571957069,-1.25274977112251,120.616121092604));
#54750=CARTESIAN_POINT('Ctrl Pts',(18.2054777306114,-1.50609466901128,120.654960228881));
#54751=CARTESIAN_POINT('Ctrl Pts',(18.8465084682623,-1.49719808014636,120.693855368907));
#54752=CARTESIAN_POINT('Ctrl Pts',(19.4287811906121,-1.2268814515038,120.732803143256));
#54753=CARTESIAN_POINT('Ctrl Pts',(19.850388348535,-0.741698347844994,120.771800144215));
#54754=CARTESIAN_POINT('Ctrl Pts',(20.0372674102143,-0.125904739992541,
120.810842936167));
#54755=CARTESIAN_POINT('Ctrl Pts',(19.9562362814235,0.513203014455754,120.849928044874));
#54756=CARTESIAN_POINT('Ctrl Pts',(19.6208945619106,1.0640151196956,120.889051981027));
#54757=CARTESIAN_POINT('Ctrl Pts',(19.0893414896838,1.43014628984235,120.928211200816));
#54758=CARTESIAN_POINT('Ctrl Pts',(18.4540890328838,1.54731880733756,120.967402188646));
#54759=CARTESIAN_POINT('Ctrl Pts',(17.8259326540409,1.39470008780894,121.006621310676));
#54760=CARTESIAN_POINT('Ctrl Pts',(17.3145823586523,0.998555219088929,121.045865097348));
#54761=CARTESIAN_POINT('Ctrl Pts',(17.0094747415844,0.427826827738151,121.085129718059));
#54762=CARTESIAN_POINT('Ctrl Pts',(16.9640777387006,-0.218091263932203,
121.124411982227));
#54763=CARTESIAN_POINT('Ctrl Pts',(17.130918600528,-0.674247594855583,121.153883510412));
#54764=CARTESIAN_POINT('Ctrl Pts',(17.3138014149502,-0.933512874257721,
121.173534979156));
#54765=CARTESIAN_POINT('Ctrl Pts',(17.4530421733364,-1.09265995262176,121.186636051418));
#54766=CARTESIAN_POINT('Ctrl Pts',(17.7385750620485,-1.33073917465461,121.209565675458));
#54767=CARTESIAN_POINT('Ctrl Pts',(18.2401816117862,-1.53044037240608,121.242325830746));
#54768=CARTESIAN_POINT('Ctrl Pts',(18.8876846243691,-1.50314303435984,121.281640996012));
#54769=CARTESIAN_POINT('Ctrl Pts',(19.4674781468588,-1.21384361944328,121.320955204458));
#54770=CARTESIAN_POINT('Ctrl Pts',(19.8785262374103,-0.712971704074119,
121.360264930557));
#54771=CARTESIAN_POINT('Ctrl Pts',(20.0490844123739,-0.0880460210185634,
121.399566456549));
#54772=CARTESIAN_POINT('Ctrl Pts',(19.9495540137019,0.551858347376732,121.438856173297));
#54773=CARTESIAN_POINT('Ctrl Pts',(19.5974666870083,1.09507568907155,121.478130424469));
#54774=CARTESIAN_POINT('Ctrl Pts',(19.0544768654203,1.44693457162279,121.517385592229));
#54775=CARTESIAN_POINT('Ctrl Pts',(18.4154972537208,1.54625877810524,121.556618056793));
#54776=CARTESIAN_POINT('Ctrl Pts',(17.7920996522822,1.37604183951388,121.595824221844));
#54777=CARTESIAN_POINT('Ctrl Pts',(17.2929810705988,0.966354646499578,121.635000506818));
#54778=CARTESIAN_POINT('Ctrl Pts',(17.004980218725,0.389027537158531,121.674143350793));
#54779=CARTESIAN_POINT('Ctrl Pts',(16.9779354617802,-0.254970506734332,
121.713249217133));
#54780=CARTESIAN_POINT('Ctrl Pts',(17.2160457097184,-0.853225362726958,
121.752314588298));
#54781=CARTESIAN_POINT('Ctrl Pts',(17.6772270736164,-1.30153725689535,121.791335987055));
#54782=CARTESIAN_POINT('Ctrl Pts',(18.280563801658,-1.522109234509,121.830309943406));
#54783=CARTESIAN_POINT('Ctrl Pts',(18.9205345174637,-1.47706436765061,121.869233063613));
#54784=CARTESIAN_POINT('Ctrl Pts',(19.4854989461127,-1.17497713175005,121.908101903289));
#54785=CARTESIAN_POINT('Ctrl Pts',(19.877218120182,-0.669217905916773,121.946913212876));
#54786=CARTESIAN_POINT('Ctrl Pts',(20.027954611204,-0.0485663563189042,
121.985663485908));
#54787=CARTESIAN_POINT('Ctrl Pts',(19.9122221117287,0.578502033445827,122.024349735476));
#54788=CARTESIAN_POINT('Ctrl Pts',(19.5510980447147,1.10267673035263,122.062968476763));
#54789=CARTESIAN_POINT('Ctrl Pts',(19.008358735754,1.4330323440933,122.101516650726));
#54790=CARTESIAN_POINT('Ctrl Pts',(18.3792313621179,1.51273490014566,122.139991110259));
#54791=CARTESIAN_POINT('Ctrl Pts',(17.7736319859323,1.3288869614174,122.178388737758));
#54792=CARTESIAN_POINT('Ctrl Pts',(17.2969403519651,0.914578061633921,122.216706534334));
#54793=CARTESIAN_POINT('Ctrl Pts',(17.0316254152085,0.342938327687217,122.254941518211));
#54794=CARTESIAN_POINT('Ctrl Pts',(17.0229584803841,-0.285798262575817,
122.293090735968));
#54795=CARTESIAN_POINT('Ctrl Pts',(17.2712780130928,-0.861895236579561,
122.331151377767));
#54796=CARTESIAN_POINT('Ctrl Pts',(17.7321373752124,-1.28529911750752,122.369120583684));
#54797=CARTESIAN_POINT('Ctrl Pts',(18.324268585886,-1.48304302933555,122.406995648865));
#54798=CARTESIAN_POINT('Ctrl Pts',(18.943934995372,-1.42184009998327,122.444773893392));
#54799=CARTESIAN_POINT('Ctrl Pts',(19.4831319671316,-1.11368417665321,122.482452674253));
#54800=CARTESIAN_POINT('Ctrl Pts',(19.8484430472875,-0.613528621914714,
122.520029499532));
#54801=CARTESIAN_POINT('Ctrl Pts',(19.9772418314858,-0.00946603320977227,
122.55750183048));
#54802=CARTESIAN_POINT('Ctrl Pts',(19.8484484572925,0.592790433281014,122.594867332922));
#54803=CARTESIAN_POINT('Ctrl Pts',(19.4859506986768,1.08847020229008,122.632123577563));
#54804=CARTESIAN_POINT('Ctrl Pts',(18.9542199651723,1.39193826091876,122.669268450296));
#54805=CARTESIAN_POINT('Ctrl Pts',(18.3467642170425,1.45156152895867,122.706299619877));
#54806=CARTESIAN_POINT('Ctrl Pts',(17.769753863205,1.25849341836473,122.743215077924));
#54807=CARTESIAN_POINT('Ctrl Pts',(17.3233542581996,0.847860663667533,122.78001275512));
#54808=CARTESIAN_POINT('Ctrl Pts',(17.0843926590814,0.292596511201441,122.816690711866));
#54809=CARTESIAN_POINT('Ctrl Pts',(17.092085167056,-0.243030263092677,122.849185287392));
#54810=CARTESIAN_POINT('Ctrl Pts',(17.257257453301,-0.673940750281189,122.87753804838));
#54811=CARTESIAN_POINT('Ctrl Pts',(17.57311479071,-1.09519924960301,122.909867480492));
#54812=CARTESIAN_POINT('Ctrl Pts',(18.164141477298,-1.4216002905349,122.950139633626));
#54813=CARTESIAN_POINT('Ctrl Pts',(18.9696230694653,-1.37578967503559,122.998239220247));
#54814=CARTESIAN_POINT('Ctrl Pts',(19.6239280630407,-0.910798341147612,
123.046108286732));
#54815=CARTESIAN_POINT('Ctrl Pts',(19.9291530020374,-0.172616375716822,
123.09374369598));
#54816=CARTESIAN_POINT('Ctrl Pts',(19.7954441463139,0.611082382716884,123.141142539284));
#54817=CARTESIAN_POINT('Ctrl Pts',(19.3559189355603,1.10190606845524,123.180442267812));
#54818=CARTESIAN_POINT('Ctrl Pts',(18.8899307018718,1.30920832624538,123.211761321333));
#54819=CARTESIAN_POINT('Ctrl Pts',(18.5263742070194,1.36095381325754,123.234322232426));
#54820=CARTESIAN_POINT('Ctrl Pts',(18.1775435791038,1.31674673854746,123.255962213161));
#54821=CARTESIAN_POINT('Ctrl Pts',(17.7593333092916,1.15328432565283,123.283597019229));
#54822=CARTESIAN_POINT('Ctrl Pts',(17.3398307943576,0.763703083387018,123.318019536972));
#54823=CARTESIAN_POINT('Ctrl Pts',(17.1587817619038,0.223479402479618,123.352279789599));
#54824=CARTESIAN_POINT('Ctrl Pts',(17.1817179901053,-0.21965108746767,123.379590264377));
#54825=CARTESIAN_POINT('Ctrl Pts',(17.3115269973765,-0.642795882173348,
123.406835412008));
#54826=CARTESIAN_POINT('Ctrl Pts',(17.6636164923134,-1.08399859950636,123.440769257244));
#54827=CARTESIAN_POINT('Ctrl Pts',(18.2330731955017,-1.32335926805016,123.477916162675));
#54828=CARTESIAN_POINT('Ctrl Pts',(18.7844078123242,-1.30212295801351,123.511542460656));
#54829=CARTESIAN_POINT('Ctrl Pts',(19.237729586223,-1.10435198427873,123.541695259909));
#54830=CARTESIAN_POINT('Ctrl Pts',(19.5861320260864,-0.755606676065294,
123.571737216082));
#54831=CARTESIAN_POINT('Ctrl Pts',(19.7823338166623,-0.305527423581674,
123.601668369117));
#54832=CARTESIAN_POINT('Ctrl Pts',(19.8004670543637,0.183419600739397,123.631488872885));
#54833=CARTESIAN_POINT('Ctrl Pts',(19.6393061251712,0.643384293867979,123.661198852101));
#54834=CARTESIAN_POINT('Ctrl Pts',(19.3752597155567,0.950094183277476,123.685865350904));
#54835=CARTESIAN_POINT('Ctrl Pts',(19.1084833026195,1.12428378128028,123.705543516584));
#54836=CARTESIAN_POINT('Ctrl Pts',(18.7659233778752,1.2668057521504,123.728458733859));
#54837=CARTESIAN_POINT('Ctrl Pts',(18.2510086222503,1.29223736298827,123.759451911037));
#54838=CARTESIAN_POINT('Ctrl Pts',(17.7649077298888,1.05761469451992,123.791914783735));
#54839=CARTESIAN_POINT('Ctrl Pts',(17.4792767223923,0.748967846692912,123.817788794064));
#54840=CARTESIAN_POINT('Ctrl Pts',(17.329077898565,0.47291654541466,123.837146270913));
#54841=CARTESIAN_POINT('Ctrl Pts',(17.2252669564987,0.0673940502346189,
123.862892562462));
#54842=CARTESIAN_POINT('Ctrl Pts',(17.2852604391398,-0.408471018364417,
123.89174995223));
#54843=CARTESIAN_POINT('Ctrl Pts',(17.5645778305311,-0.851824873362711,
123.923676060479));
#54844=CARTESIAN_POINT('Ctrl Pts',(17.9580568083485,-1.14230514083795,123.953496928898));
#54845=CARTESIAN_POINT('Ctrl Pts',(18.4529779621923,-1.26241680311112,123.984390222781));
#54846=CARTESIAN_POINT('Ctrl Pts',(18.9708103094374,-1.16668504108039,124.01634052165));
#54847=CARTESIAN_POINT('Ctrl Pts',(19.366630228591,-0.893819587524324,124.045509327258));
#54848=CARTESIAN_POINT('Ctrl Pts',(19.5610749691126,-0.608733295788248,
124.066648060783));
#54849=CARTESIAN_POINT('Ctrl Pts',(19.6687801575205,-0.346185382792283,
124.084228340358));
#54850=CARTESIAN_POINT('Ctrl Pts',(19.7217080738956,-0.0799700980385591,
124.100898985158));
#54851=CARTESIAN_POINT('Ctrl Pts',(19.6928905271332,0.260729788345592,124.121900560401));
#54852=CARTESIAN_POINT('Ctrl Pts',(19.5712258979927,0.579308030812463,124.142846849415));
#54853=CARTESIAN_POINT('Ctrl Pts',(19.3666436814044,0.851037647129537,124.16373812114));
#54854=CARTESIAN_POINT('Ctrl Pts',(19.0955647657873,1.05496769594385,124.184575019819));
#54855=CARTESIAN_POINT('Ctrl Pts',(18.8057448596413,1.16555851345604,124.203626193165));
#54856=CARTESIAN_POINT('Ctrl Pts',(18.5276285134945,1.19871213746157,124.220906472711));
#54857=CARTESIAN_POINT('Ctrl Pts',(18.1934516179046,1.16838186372108,124.241603159253));
#54858=CARTESIAN_POINT('Ctrl Pts',(17.8030055811293,1.00012280453531,124.267400343048));
#54859=CARTESIAN_POINT('Ctrl Pts',(17.4591443613634,0.625680307947734,124.298240874512));
#54860=CARTESIAN_POINT('Ctrl Pts',(17.298780306353,0.145317478363908,124.328967538828));
#54861=CARTESIAN_POINT('Ctrl Pts',(17.3484322588003,-0.356863082032555,
124.359582443048));
#54862=CARTESIAN_POINT('Ctrl Pts',(17.5979613332727,-0.793375340327835,
124.390087870071));
#54863=CARTESIAN_POINT('Ctrl Pts',(18.0025932240276,-1.08887194841174,124.420486124645));
#54864=CARTESIAN_POINT('Ctrl Pts',(18.4909367856316,-1.19296322240431,124.450779612303));
#54865=CARTESIAN_POINT('Ctrl Pts',(18.9775569396537,-1.08887495450386,124.480970793866));
#54866=CARTESIAN_POINT('Ctrl Pts',(19.3778957756401,-0.796079646301384,
124.511062207275));
#54867=CARTESIAN_POINT('Ctrl Pts',(19.6229378177282,-0.366699000956798,
124.541056454746));
#54868=CARTESIAN_POINT('Ctrl Pts',(19.6710819454008,0.123768576792137,124.570956206973));
#54869=CARTESIAN_POINT('Ctrl Pts',(19.5151825214616,0.589690167012718,124.6007641975));
#54870=CARTESIAN_POINT('Ctrl Pts',(19.1835730252442,0.950223228101631,124.63048322199));
#54871=CARTESIAN_POINT('Ctrl Pts',(18.7349333590939,1.14331075884206,124.660116135655));
#54872=CARTESIAN_POINT('Ctrl Pts',(18.2479281964886,1.13633797140025,124.689665853396));
#54873=CARTESIAN_POINT('Ctrl Pts',(17.8074430853533,0.931620578918509,124.719135346688));
#54874=CARTESIAN_POINT('Ctrl Pts',(17.4898217356975,0.565808383480578,124.748527641549));
#54875=CARTESIAN_POINT('Ctrl Pts',(17.3496657150365,0.103341142817895,124.777845815482));
#54876=CARTESIAN_POINT('Ctrl Pts',(17.4104730137507,-0.374876916066361,
124.807092995679));
#54877=CARTESIAN_POINT('Ctrl Pts',(17.6607161319537,-0.785598124605828,
124.836272358739));
#54878=CARTESIAN_POINT('Ctrl Pts',(18.0560104898594,-1.05768804968322,124.865387127451));
#54879=CARTESIAN_POINT('Ctrl Pts',(18.526967068725,-1.14441382762597,124.894440568606));
#54880=CARTESIAN_POINT('Ctrl Pts',(18.9913431026315,-1.0314475639091,124.923435989685));
#54881=CARTESIAN_POINT('Ctrl Pts',(19.3683685002177,-0.739218678075058,
124.952376736826));
#54882=CARTESIAN_POINT('Ctrl Pts',(19.5927584790688,-0.319231596033026,
124.981266194478));
#54883=CARTESIAN_POINT('Ctrl Pts',(19.6259873268813,0.154988889320898,125.010107782232));
#54884=CARTESIAN_POINT('Ctrl Pts',(19.4628825553958,0.60073609927402,125.038904952244));
#54885=CARTESIAN_POINT('Ctrl Pts',(19.1324150236228,0.940507944126239,125.067661186012));
#54886=CARTESIAN_POINT('Ctrl Pts',(18.6925674228159,1.11544599427495,125.09637999193));
#54887=CARTESIAN_POINT('Ctrl Pts',(18.220187394042,1.09550298745015,125.125064904932));
#54888=CARTESIAN_POINT('Ctrl Pts',(17.7975969993875,0.884587280323155,125.153719483493));
#54889=CARTESIAN_POINT('Ctrl Pts',(17.498285758871,0.519807155829135,125.182347306636));
#54890=CARTESIAN_POINT('Ctrl Pts',(17.3741663376746,0.0649598517818115,
125.210951970916));
#54891=CARTESIAN_POINT('Ctrl Pts',(17.4465962994511,-0.400595566794844,
125.239537087522));
#54892=CARTESIAN_POINT('Ctrl Pts',(17.702714511609,-0.795746326978485,125.268106281994));
#54893=CARTESIAN_POINT('Ctrl Pts',(18.0977185791255,-1.0517185595441,125.296663191365));
#54894=CARTESIAN_POINT('Ctrl Pts',(18.5626804301901,-1.12401300878258,125.325211460905));
#54895=CARTESIAN_POINT('Ctrl Pts',(19.0165404416634,-1.00011889006815,125.353754741278));
#54896=CARTESIAN_POINT('Ctrl Pts',(19.3801993580427,-0.701672757556588,
125.382296685284));
#54897=CARTESIAN_POINT('Ctrl Pts',(19.5902652601078,-0.280690435726507,
125.410840947633));
#54898=CARTESIAN_POINT('Ctrl Pts',(19.6100726418786,0.189473466106149,125.439391182285));
#54899=CARTESIAN_POINT('Ctrl Pts',(19.4360640155898,0.626871185373153,125.467951038996));
#54900=CARTESIAN_POINT('Ctrl Pts',(19.0984268547706,0.955204626959225,125.496524160671));
#54901=CARTESIAN_POINT('Ctrl Pts',(18.6558720003985,1.11709745415395,125.525114179851));
#54902=CARTESIAN_POINT('Ctrl Pts',(18.1854533778308,1.08409412045259,125.553724718471));
#54903=CARTESIAN_POINT('Ctrl Pts',(17.7691894439931,0.861647559159082,125.582359385548));
#54904=CARTESIAN_POINT('Ctrl Pts',(17.4798028826353,0.488224059886903,125.611021773455));
#54905=CARTESIAN_POINT('Ctrl Pts',(17.3680505492265,0.028671246726309,125.639715455637));
#54906=CARTESIAN_POINT('Ctrl Pts',(17.4538447442219,-0.437011366440344,
125.668443982813));
#54907=CARTESIAN_POINT('Ctrl Pts',(17.7227152954249,-0.827560849480737,
125.697210882868));
#54908=CARTESIAN_POINT('Ctrl Pts',(18.1282398436561,-1.07459346383945,125.726019658635));
#54909=CARTESIAN_POINT('Ctrl Pts',(18.6000357415897,-1.13454664475889,125.754873784372));
#54910=CARTESIAN_POINT('Ctrl Pts',(19.0559420543163,-0.996340771154775,
125.783776703428));
#54911=CARTESIAN_POINT('Ctrl Pts',(19.4162896725845,-0.683416566476759,
125.81273182463));
#54912=CARTESIAN_POINT('Ctrl Pts',(19.6177879629471,-0.249774365013851,
125.841742522047));
#54913=CARTESIAN_POINT('Ctrl Pts',(19.6246130111878,0.229318651775951,125.870812133036));
#54914=CARTESIAN_POINT('Ctrl Pts',(19.4347596171185,0.670358453751199,125.899943954864));
#54915=CARTESIAN_POINT('Ctrl Pts',(19.0805337627966,0.996122063548543,125.929141242478));
#54916=CARTESIAN_POINT('Ctrl Pts',(18.6230742316303,1.14915614382532,125.958407205093));
#54917=CARTESIAN_POINT('Ctrl Pts',(18.1418280742596,1.10188574238829,125.987745005866));
#54918=CARTESIAN_POINT('Ctrl Pts',(17.7207864948947,0.861567901278113,126.0171577601));
#54919=CARTESIAN_POINT('Ctrl Pts',(17.4338601270708,0.46920267105939,126.046648532321));
#54920=CARTESIAN_POINT('Ctrl Pts',(17.3319338973738,-0.00744028244417294,
126.076220333858));
#54921=CARTESIAN_POINT('Ctrl Pts',(17.4338635816607,-0.48549799831244,126.105876120044));
#54922=CARTESIAN_POINT('Ctrl Pts',(17.7230041681992,-0.881387583071317,
126.135618789578));
#54923=CARTESIAN_POINT('Ctrl Pts',(18.1499074077235,-1.12538888170401,126.16545118304));
#54924=CARTESIAN_POINT('Ctrl Pts',(18.6407553958162,-1.17389726511166,126.195376080285));
#54925=CARTESIAN_POINT('Ctrl Pts',(19.110096255813,-1.01719771547609,126.225396198108));
#54926=CARTESIAN_POINT('Ctrl Pts',(19.4756904241207,-0.681377009093858,
126.255514187869));
#54927=CARTESIAN_POINT('Ctrl Pts',(19.6728936838703,-0.224001716190088,
126.285732634629));
#54928=CARTESIAN_POINT('Ctrl Pts',(19.6660657931652,0.275726478226854,126.316054056017));
#54929=CARTESIAN_POINT('Ctrl Pts',(19.4549941835243,0.730659016820871,126.346480900112));
#54930=CARTESIAN_POINT('Ctrl Pts',(19.0751783442302,1.0608711604977,126.37701554289));
#54931=CARTESIAN_POINT('Ctrl Pts',(18.5918798815844,1.2076802849347,126.407660287092));
#54932=CARTESIAN_POINT('Ctrl Pts',(18.088932931197,1.14405521959446,126.438417359648));
#54933=CARTESIAN_POINT('Ctrl Pts',(17.6542245236157,0.879575635245244,126.469288913932));
#54934=CARTESIAN_POINT('Ctrl Pts',(17.3643636459841,0.459028112591109,126.5002770223));
#54935=CARTESIAN_POINT('Ctrl Pts',(17.2711939938056,-0.0451525818812408,
126.531383684238));
#54936=CARTESIAN_POINT('Ctrl Pts',(17.3925496972517,-0.545347189477102,
126.562610806295));
#54937=CARTESIAN_POINT('Ctrl Pts',(17.7088476742613,-0.953940800655802,
126.593960235512));
#54938=CARTESIAN_POINT('Ctrl Pts',(18.1662621639506,-1.19868197962896,126.625433694777));
#54939=CARTESIAN_POINT('Ctrl Pts',(18.6857870320997,-1.23538347152007,126.657032901379));
#54940=CARTESIAN_POINT('Ctrl Pts',(19.1770109198137,-1.05599536532106,126.688759339219));
#54941=CARTESIAN_POINT('Ctrl Pts',(19.4907918421248,-0.751068679762662,
126.715305466298));
#54942=CARTESIAN_POINT('Ctrl Pts',(19.6511793003569,-0.445245949338393,
126.73660731796));
#54943=CARTESIAN_POINT('Ctrl Pts',(19.7449908411919,-0.112183045382465,
126.757952973406));
#54944=CARTESIAN_POINT('Ctrl Pts',(19.7266891552073,0.328560035877289,126.784717043322));
#54945=CARTESIAN_POINT('Ctrl Pts',(19.4895319957358,0.804308800674381,126.816966807474));
#54946=CARTESIAN_POINT('Ctrl Pts',(19.077093245759,1.14310156338576,126.84935038456));
#54947=CARTESIAN_POINT('Ctrl Pts',(18.5600737160613,1.28447435350301,126.881868928107));
#54948=CARTESIAN_POINT('Ctrl Pts',(18.0282062679645,1.20200111344108,126.914523338728));
#54949=CARTESIAN_POINT('Ctrl Pts',(17.5745116558757,0.908257909117066,126.947314510873));
#54950=CARTESIAN_POINT('Ctrl Pts',(17.2791351203368,0.45292366127595,126.980243200589));
#54951=CARTESIAN_POINT('Ctrl Pts',(17.1951454991029,-0.0855934603369406,
127.013310094763));
#54952=CARTESIAN_POINT('Ctrl Pts',(17.3390382074035,-0.613655007911289,
127.046515773498));
#54953=CARTESIAN_POINT('Ctrl Pts',(17.6875198362081,-1.0386636260325,127.079860729247));
#54954=CARTESIAN_POINT('Ctrl Pts',(18.181260402214,-1.28529745768021,127.113345357394));
#54955=CARTESIAN_POINT('Ctrl Pts',(18.7349795771802,-1.30885272449037,127.146969959054));
#54956=CARTESIAN_POINT('Ctrl Pts',(19.2521732788533,-1.10333621731152,127.180734741782));
#54957=CARTESIAN_POINT('Ctrl Pts',(19.6419290401089,-0.702841603331218,
127.214639813623));
#54958=CARTESIAN_POINT('Ctrl Pts',(19.8349060622305,-0.175911321282134,
127.248685196296));
#54959=CARTESIAN_POINT('Ctrl Pts',(19.7956686304382,0.386187668303325,127.282870799533));
#54960=CARTESIAN_POINT('Ctrl Pts',(19.5291784681672,0.885271812874289,127.317196470363));
#54961=CARTESIAN_POINT('Ctrl Pts',(19.0802611718389,1.23339149582639,127.351661899081));
#54962=CARTESIAN_POINT('Ctrl Pts',(18.5260767506703,1.3683341345413,127.386266797367));
#54963=CARTESIAN_POINT('Ctrl Pts',(17.9628555970782,1.26473704354384,127.421010556494));
#54964=CARTESIAN_POINT('Ctrl Pts',(17.4891965904045,0.938837633413158,127.455892935242));
#54965=CARTESIAN_POINT('Ctrl Pts',(17.1887742378464,0.445956210839747,127.490912627166));
#54966=CARTESIAN_POINT('Ctrl Pts',(17.1155871988033,-0.128878759482379,
127.526070226388));
#54967=CARTESIAN_POINT('Ctrl Pts',(17.2842442567953,-0.6856327348833,127.561362414191));
#54968=CARTESIAN_POINT('Ctrl Pts',(17.6669802913474,-1.12658965503124,127.596792558688));
#54969=CARTESIAN_POINT('Ctrl Pts',(18.1986315984172,-1.37375997079926,127.632352264871));
#54970=CARTESIAN_POINT('Ctrl Pts',(18.7867735556596,-1.38213293233228,127.668054104116));
#54971=CARTESIAN_POINT('Ctrl Pts',(19.3292837483826,-1.1488895601724,127.7038701522));
#54972=CARTESIAN_POINT('Ctrl Pts',(19.7308757076997,-0.712514467722855,
127.739846925354));
#54973=CARTESIAN_POINT('Ctrl Pts',(19.918472262676,-0.148383127901019,127.775918194433));
#54974=CARTESIAN_POINT('Ctrl Pts',(19.8719539849658,0.345937981508172,127.806087591881));
#54975=CARTESIAN_POINT('Ctrl Pts',(19.7127708262951,0.70607801146938,127.830337982654));
#54976=CARTESIAN_POINT('Ctrl Pts',(19.5386023042488,0.945577081476424,127.848504632835));
#54977=CARTESIAN_POINT('Ctrl Pts',(19.3198906328131,1.14364161409795,127.866689814571));
#54978=CARTESIAN_POINT('Ctrl Pts',(19.0678313013017,1.2914197254424,127.884957912083));
#54979=CARTESIAN_POINT('Ctrl Pts',(18.7904620761009,1.38257654608712,127.903291001622));
#54980=CARTESIAN_POINT('Ctrl Pts',(18.5922400986655,1.40380723379247,127.915441694516));
#54981=CARTESIAN_POINT('Ctrl Pts',(18.4903128297246,1.40466511306502,127.92147546947));
#54982=CARTESIAN_POINT('Ctrl Pts',(18.4897811044666,1.46372061123931,112.750652102996));
#54983=CARTESIAN_POINT('Ctrl Pts',(18.3305659168598,1.46238056347085,112.760077143174));
#54984=CARTESIAN_POINT('Ctrl Pts',(18.125793406092,1.42986577729673,112.772844964474));
#54985=CARTESIAN_POINT('Ctrl Pts',(17.8412845056959,1.31915463921368,112.792067023561));
#54986=CARTESIAN_POINT('Ctrl Pts',(17.6209713973646,1.1900784659798,112.80803570717));
#54987=CARTESIAN_POINT('Ctrl Pts',(17.3911882883068,0.981968016985861,112.827140907135));
#54988=CARTESIAN_POINT('Ctrl Pts',(17.2073171982579,0.729393018088631,112.846306361443));
#54989=CARTESIAN_POINT('Ctrl Pts',(17.0384351507011,0.347283122277831,112.872036780446));
#54990=CARTESIAN_POINT('Ctrl Pts',(16.9886748804566,-0.178292311259029,
112.904115521818));
#54991=CARTESIAN_POINT('Ctrl Pts',(17.1889316142324,-0.781749189448536,
112.942692992335));
#54992=CARTESIAN_POINT('Ctrl Pts',(17.6209789196198,-1.25188558375487,112.981429235051));
#54993=CARTESIAN_POINT('Ctrl Pts',(18.2079353711238,-1.5045708835093,113.020185323627));
#54994=CARTESIAN_POINT('Ctrl Pts',(18.8482829043636,-1.49590845051623,113.05905837792));
#54995=CARTESIAN_POINT('Ctrl Pts',(19.4304958659054,-1.22560756348276,113.097987904393));
#54996=CARTESIAN_POINT('Ctrl Pts',(19.8522306332794,-0.740339244651456,
113.137001694574));
#54997=CARTESIAN_POINT('Ctrl Pts',(20.0393256416704,-0.123981173335954,
113.176077472417));
#54998=CARTESIAN_POINT('Ctrl Pts',(19.9582169960145,0.516105276266115,113.215223894842));
#54999=CARTESIAN_POINT('Ctrl Pts',(19.6221913410372,1.06810878123685,113.254429998878));
#55000=CARTESIAN_POINT('Ctrl Pts',(19.0892198662845,1.43526754494134,113.293696217054));
#55001=CARTESIAN_POINT('Ctrl Pts',(18.4518647573978,1.55287245970027,113.333016998286));
#55002=CARTESIAN_POINT('Ctrl Pts',(17.8212439746614,1.39968964394208,113.372389563759));
#55003=CARTESIAN_POINT('Ctrl Pts',(17.3075692374066,1.00180608691406,113.411809801272));
#55004=CARTESIAN_POINT('Ctrl Pts',(17.000873284185,0.42817270456625,113.451274197287));
#55005=CARTESIAN_POINT('Ctrl Pts',(16.9551821048933,-0.22136165817646,113.49077889699));
#55006=CARTESIAN_POINT('Ctrl Pts',(17.1789901136725,-0.833471727017209,
113.530320136614));
#55007=CARTESIAN_POINT('Ctrl Pts',(17.6336675842817,-1.30116454392376,113.569894150434));
#55008=CARTESIAN_POINT('Ctrl Pts',(18.2401696678772,-1.54252645140642,113.60949699668));
#55009=CARTESIAN_POINT('Ctrl Pts',(18.8927538416101,-1.51509157179902,113.64912505003));
#55010=CARTESIAN_POINT('Ctrl Pts',(19.4775429231303,-1.22333733766362,113.68877409611));
#55011=CARTESIAN_POINT('Ctrl Pts',(19.8923283686142,-0.717952641965618,
113.728440607448));
#55012=CARTESIAN_POINT('Ctrl Pts',(20.0645752690355,-0.0870289267892908,
113.768120453468));
#55013=CARTESIAN_POINT('Ctrl Pts',(19.9640685005371,0.559400324613147,113.807809828465));
#55014=CARTESIAN_POINT('Ctrl Pts',(19.6082418329362,1.10844386956989,113.847504852794));
#55015=CARTESIAN_POINT('Ctrl Pts',(19.0591636449125,1.46432165094386,113.887201491434));
#55016=CARTESIAN_POINT('Ctrl Pts',(18.5204080967549,1.54803402763228,113.920280307134));
#55017=CARTESIAN_POINT('Ctrl Pts',(18.0971213830127,1.47872672380361,113.946740145263));
#55018=CARTESIAN_POINT('Ctrl Pts',(17.6973555935897,1.32336298729138,113.973197285216));
#55019=CARTESIAN_POINT('Ctrl Pts',(17.2760459903937,0.977663903758167,114.006262645077));
#55020=CARTESIAN_POINT('Ctrl Pts',(16.9841963480954,0.392626824069597,114.045926931518));
#55021=CARTESIAN_POINT('Ctrl Pts',(16.9567342727123,-0.260253158742564,
114.085573459637));
#55022=CARTESIAN_POINT('Ctrl Pts',(17.1982278925264,-0.867095767455903,
114.125198265763));
#55023=CARTESIAN_POINT('Ctrl Pts',(17.6662113538874,-1.32206355425537,114.164797473269));
#55024=CARTESIAN_POINT('Ctrl Pts',(18.2787609337407,-1.54603968390748,114.20436727098));
#55025=CARTESIAN_POINT('Ctrl Pts',(18.9288172222856,-1.50031607897088,114.243903822103));
#55026=CARTESIAN_POINT('Ctrl Pts',(19.5029618017992,-1.19335509858773,114.283403282528));
#55027=CARTESIAN_POINT('Ctrl Pts',(19.901237024244,-0.679182233478761,114.322861954074));
#55028=CARTESIAN_POINT('Ctrl Pts',(20.0545852373889,-0.047903393129132,
114.362275981028));
#55029=CARTESIAN_POINT('Ctrl Pts',(19.9368537301759,0.590185965224506,114.40164173171));
#55030=CARTESIAN_POINT('Ctrl Pts',(19.5692562741686,1.12380691439424,114.440955473318));
#55031=CARTESIAN_POINT('Ctrl Pts',(19.0165331060083,1.46027294727139,114.480213553625));
#55032=CARTESIAN_POINT('Ctrl Pts',(18.375563704988,1.54150263789562,114.519412367348));
#55033=CARTESIAN_POINT('Ctrl Pts',(17.7583100289019,1.35414393426942,114.5585483306));
#55034=CARTESIAN_POINT('Ctrl Pts',(17.2722472743633,0.931726226959488,114.597617913046));
#55035=CARTESIAN_POINT('Ctrl Pts',(17.001603535348,0.348658869884238,114.636617630877));
#55036=CARTESIAN_POINT('Ctrl Pts',(16.9927335372165,-0.292881472094132,
114.675544031198));
#55037=CARTESIAN_POINT('Ctrl Pts',(17.2461846841767,-0.880944809491311,
114.714393746167));
#55038=CARTESIAN_POINT('Ctrl Pts',(17.7167374067633,-1.31327003087369,114.753163390647));
#55039=CARTESIAN_POINT('Ctrl Pts',(18.3215624607069,-1.51531409642752,114.791849768283));
#55040=CARTESIAN_POINT('Ctrl Pts',(18.8491562346418,-1.46314533152096,114.824016194578));
#55041=CARTESIAN_POINT('Ctrl Pts',(19.2302731192541,-1.29534293564721,114.849704556036));
#55042=CARTESIAN_POINT('Ctrl Pts',(19.5680201993842,-1.05257590633892,114.87536252632));
#55043=CARTESIAN_POINT('Ctrl Pts',(19.8793194019256,-0.626525224187843,
114.907376795667));
#55044=CARTESIAN_POINT('Ctrl Pts',(20.0110263896328,-0.00874579380907211,
114.945698209434));
#55045=CARTESIAN_POINT('Ctrl Pts',(19.8793086186887,0.607314790118817,114.983920680183));
#55046=CARTESIAN_POINT('Ctrl Pts',(19.5084111324286,1.11450997297525,115.022041429527));
#55047=CARTESIAN_POINT('Ctrl Pts',(18.964206619524,1.42510388242354,115.060057532941));
#55048=CARTESIAN_POINT('Ctrl Pts',(18.3423681279344,1.48616747636079,115.09796627472));
#55049=CARTESIAN_POINT('Ctrl Pts',(17.751531483489,1.28847084357424,115.135764893611));
#55050=CARTESIAN_POINT('Ctrl Pts',(17.2943774305468,0.86797834662618,115.173450851635));
#55051=CARTESIAN_POINT('Ctrl Pts',(17.0495318909918,0.299122922775257,115.211021448735));
#55052=CARTESIAN_POINT('Ctrl Pts',(17.0575062136741,-0.249489879927474,
115.244313053249));
#55053=CARTESIAN_POINT('Ctrl Pts',(17.2265723807848,-0.691296868335461,
115.273365038483));
#55054=CARTESIAN_POINT('Ctrl Pts',(17.4088824641546,-0.933730795312457,
115.292001216897));
#55055=CARTESIAN_POINT('Ctrl Pts',(17.5553960293834,-1.07013569528572,115.304407717233));
#55056=CARTESIAN_POINT('Ctrl Pts',(17.6331027617258,-1.1330673537071,115.310607741085));
#55057=CARTESIAN_POINT('Ctrl Pts',(17.7150593184202,-1.19031116283603,115.31680421033));
#55058=CARTESIAN_POINT('Ctrl Pts',(17.8863953605569,-1.29308480412215,115.329190651479));
#55059=CARTESIAN_POINT('Ctrl Pts',(18.1686370240243,-1.40074582057259,115.347743492983));
#55060=CARTESIAN_POINT('Ctrl Pts',(18.5690163480438,-1.43447133078092,115.372425439255));
#55061=CARTESIAN_POINT('Ctrl Pts',(18.9622857850623,-1.356175093929,115.397050104753));
#55062=CARTESIAN_POINT('Ctrl Pts',(19.3174893024164,-1.17255993098256,115.421618022958));
#55063=CARTESIAN_POINT('Ctrl Pts',(19.6076271996196,-0.898329980683078,
115.446127643009));
#55064=CARTESIAN_POINT('Ctrl Pts',(19.8094258000695,-0.55549666470966,115.470579183103));
#55065=CARTESIAN_POINT('Ctrl Pts',(19.9426156970628,-0.0425558216700198,
115.503102315118));
#55066=CARTESIAN_POINT('Ctrl Pts',(19.8514135668701,0.492534124086972,115.535506467039));
#55067=CARTESIAN_POINT('Ctrl Pts',(19.5947255019288,0.874650732212783,115.563754295808));
#55068=CARTESIAN_POINT('Ctrl Pts',(19.4083996970038,1.05617431733856,115.579865220324));
#55069=CARTESIAN_POINT('Ctrl Pts',(19.1982429433524,1.2096203916672,115.595955885261));
#55070=CARTESIAN_POINT('Ctrl Pts',(18.989589114405,1.30306979403804,115.610008424767));
#55071=CARTESIAN_POINT('Ctrl Pts',(18.8013128243347,1.3501360194407,115.622033854083));
#55072=CARTESIAN_POINT('Ctrl Pts',(18.7059043584766,1.3670507590569,115.628042775347));
#55073=CARTESIAN_POINT('Ctrl Pts',(18.6256141605857,1.37555385934589,115.633046937773));
#55074=CARTESIAN_POINT('Ctrl Pts',(18.561178149311,1.37888388996972,115.637048396594));
#55075=CARTESIAN_POINT('Ctrl Pts',(18.2997000866567,1.38388444692226,115.65327107495));
#55076=CARTESIAN_POINT('Ctrl Pts',(17.8263490130143,1.2627382748751,115.682643583081));
#55077=CARTESIAN_POINT('Ctrl Pts',(17.424914370665,0.890032416107338,115.715592608078));
#55078=CARTESIAN_POINT('Ctrl Pts',(17.2467539250202,0.554805958801192,115.739053158468));
#55079=CARTESIAN_POINT('Ctrl Pts',(17.1861924514361,0.375353183495959,115.750764696338));
#55080=CARTESIAN_POINT('Ctrl Pts',(17.1564555797285,0.227296192343728,115.760122604584));
#55081=CARTESIAN_POINT('Ctrl Pts',(17.120967866444,-0.0723899313699495,
115.778823626985));
#55082=CARTESIAN_POINT('Ctrl Pts',(17.2088578800484,-0.568527186055847,
115.809127002241));
#55083=CARTESIAN_POINT('Ctrl Pts',(17.6421591341182,-1.11134999926644,115.850880748309));
#55084=CARTESIAN_POINT('Ctrl Pts',(18.2259638545534,-1.35677182815753,115.888965856558));
#55085=CARTESIAN_POINT('Ctrl Pts',(18.7911845995156,-1.3349800129774,115.923437330073));
#55086=CARTESIAN_POINT('Ctrl Pts',(19.255812563341,-1.13226888716917,115.954344416483));
#55087=CARTESIAN_POINT('Ctrl Pts',(19.6129288887079,-0.774826552610854,
115.985133850421));
#55088=CARTESIAN_POINT('Ctrl Pts',(19.7803871051415,-0.390503239648824,
116.010693444063));
#55089=CARTESIAN_POINT('Ctrl Pts',(19.8232900466592,-0.0631136113716338,
116.031081930678));
#55090=CARTESIAN_POINT('Ctrl Pts',(19.8094753804474,0.18357055636264,116.046343784384));
#55091=CARTESIAN_POINT('Ctrl Pts',(19.759963513967,0.383089889208843,116.059037249292));
#55092=CARTESIAN_POINT('Ctrl Pts',(19.6987167583072,0.534822847653917,116.069177221446));
#55093=CARTESIAN_POINT('Ctrl Pts',(19.5862796684731,0.752779622550448,116.084372388956));
#55094=CARTESIAN_POINT('Ctrl Pts',(19.3428646912038,1.03541739212991,116.107109487966));
#55095=CARTESIAN_POINT('Ctrl Pts',(18.9047700381786,1.26675694584353,116.137306977485));
#55096=CARTESIAN_POINT('Ctrl Pts',(18.4143705145873,1.32182474021267,116.167385713619));
#55097=CARTESIAN_POINT('Ctrl Pts',(18.0583443434444,1.22628304283745,116.189855803588));
#55098=CARTESIAN_POINT('Ctrl Pts',(17.8462515090041,1.11147637938476,116.204798779312));
#55099=CARTESIAN_POINT('Ctrl Pts',(17.7127049673212,1.02227301661988,116.214750887188));
#55100=CARTESIAN_POINT('Ctrl Pts',(17.5026882046262,0.834640398251948,116.232141219153));
#55101=CARTESIAN_POINT('Ctrl Pts',(17.3621175549714,0.611099620430629,116.248241208803));
#55102=CARTESIAN_POINT('Ctrl Pts',(17.2938429805976,0.423855467682653,116.260598155883));
#55103=CARTESIAN_POINT('Ctrl Pts',(17.2759262214136,0.366868133270414,116.264303404854));
#55104=CARTESIAN_POINT('Ctrl Pts',(17.2607570337696,0.309096675662953,116.268006801496));
#55105=CARTESIAN_POINT('Ctrl Pts',(17.248292579062,0.250729697737948,116.271708356085));
#55106=CARTESIAN_POINT('Ctrl Pts',(17.2385564436958,0.191862855691203,116.275408062101));
#55107=CARTESIAN_POINT('Ctrl Pts',(17.2293276540802,0.112898847873108,116.280338540313));
#55108=CARTESIAN_POINT('Ctrl Pts',(17.2189539465842,-0.105526562397861,
116.293887185899));
#55109=CARTESIAN_POINT('Ctrl Pts',(17.2865569346428,-0.46198587121534,116.316002575039));
#55110=CARTESIAN_POINT('Ctrl Pts',(17.5430611832942,-0.869881342426196,
116.345372133543));
#55111=CARTESIAN_POINT('Ctrl Pts',(17.9292997327579,-1.15471831367284,116.374624691353));
#55112=CARTESIAN_POINT('Ctrl Pts',(18.3910824032975,-1.27825989559717,116.403760596127));
#55113=CARTESIAN_POINT('Ctrl Pts',(18.8641367580531,-1.22478453810117,116.432780512622));
#55114=CARTESIAN_POINT('Ctrl Pts',(19.2833643020942,-1.00303724998616,116.461684909985));
#55115=CARTESIAN_POINT('Ctrl Pts',(19.5227871655153,-0.724505149715909,
116.484076990982));
#55116=CARTESIAN_POINT('Ctrl Pts',(19.6374182547927,-0.493683341710843,
116.500028892448));
#55117=CARTESIAN_POINT('Ctrl Pts',(19.7052765909381,-0.299410071500717,
116.512773803769));
#55118=CARTESIAN_POINT('Ctrl Pts',(19.7596827729301,0.0582630911084101,
116.535032914344));
#55119=CARTESIAN_POINT('Ctrl Pts',(19.6422842103624,0.571651584928872,116.566706373337));
#55120=CARTESIAN_POINT('Ctrl Pts',(19.2257653211103,1.04290863492653,116.604515658408));
#55121=CARTESIAN_POINT('Ctrl Pts',(18.6378872911912,1.25645660057682,116.642128600935));
#55122=CARTESIAN_POINT('Ctrl Pts',(18.0225041260444,1.16333115570126,116.679547542631));
#55123=CARTESIAN_POINT('Ctrl Pts',(17.601202923633,0.843680448939181,116.71134621701));
#55124=CARTESIAN_POINT('Ctrl Pts',(17.3846691880087,0.474999085705099,116.737611476145));
#55125=CARTESIAN_POINT('Ctrl Pts',(17.2710407476065,0.0379276543343812,
116.765343094364));
#55126=CARTESIAN_POINT('Ctrl Pts',(17.3682734853946,-0.532588354634737,
116.799861144831));
#55127=CARTESIAN_POINT('Ctrl Pts',(17.8290624618527,-1.0473695001524,116.841053271886));
#55128=CARTESIAN_POINT('Ctrl Pts',(18.4893639542835,-1.23701137347387,116.88202069821));
#55129=CARTESIAN_POINT('Ctrl Pts',(19.1457977829931,-1.04739610347266,116.922768533721));
#55130=CARTESIAN_POINT('Ctrl Pts',(19.5985173054551,-0.540139679709388,
116.96330233943));
#55131=CARTESIAN_POINT('Ctrl Pts',(19.6922387328967,0.0153796368980274,
116.996906606869));
#55132=CARTESIAN_POINT('Ctrl Pts',(19.5824301046536,0.437440499685657,117.02368902324));
#55133=CARTESIAN_POINT('Ctrl Pts',(19.4170516191088,0.71855847802177,117.043725662408));
#55134=CARTESIAN_POINT('Ctrl Pts',(19.1802672799888,0.941766571567522,117.063713592448));
#55135=CARTESIAN_POINT('Ctrl Pts',(18.7959731089366,1.14115562743497,117.090299363394));
#55136=CARTESIAN_POINT('Ctrl Pts',(18.2416584714609,1.17212298152654,117.123413149607));
#55137=CARTESIAN_POINT('Ctrl Pts',(17.6612476425556,0.85078765321395,117.16296619688));
#55138=CARTESIAN_POINT('Ctrl Pts',(17.3422279633976,0.272702222384503,117.202342864818));
#55139=CARTESIAN_POINT('Ctrl Pts',(17.3794635084803,-0.383772473351894,
117.241550095212));
#55140=CARTESIAN_POINT('Ctrl Pts',(17.7586839982553,-0.91755328435359,117.280595232539));
#55141=CARTESIAN_POINT('Ctrl Pts',(18.3613572107628,-1.16681408332463,117.319485706597));
#55142=CARTESIAN_POINT('Ctrl Pts',(19.0018467679279,-1.05764318469179,117.358229192413));
#55143=CARTESIAN_POINT('Ctrl Pts',(19.4843526169941,-0.62602185554045,117.396833518546));
#55144=CARTESIAN_POINT('Ctrl Pts',(19.6626760875841,-0.00596355109428755,
117.435306690535));
#55145=CARTESIAN_POINT('Ctrl Pts',(19.4843653350139,0.611949745664865,117.473656858281));
#55146=CARTESIAN_POINT('Ctrl Pts',(19.006082836089,1.03901891538125,117.511892338249));
#55147=CARTESIAN_POINT('Ctrl Pts',(18.3756555473465,1.14588845941846,117.550021578917));
#55148=CARTESIAN_POINT('Ctrl Pts',(17.7865034506633,0.901614741639774,117.588053147374));
#55149=CARTESIAN_POINT('Ctrl Pts',(17.4184650221663,0.38256549210635,117.625995735236));
#55150=CARTESIAN_POINT('Ctrl Pts',(17.3830379091306,-0.251394920777476,
117.663858153122));
#55151=CARTESIAN_POINT('Ctrl Pts',(17.6897416212228,-0.805988837816665,
117.701649288551));
#55152=CARTESIAN_POINT('Ctrl Pts',(18.2435530961125,-1.11192915841498,117.739378125066));
#55153=CARTESIAN_POINT('Ctrl Pts',(18.8743941085538,-1.07637392924317,117.777053713013));
#55154=CARTESIAN_POINT('Ctrl Pts',(19.3889681580371,-0.711139819413866,
117.814685205125));
#55155=CARTESIAN_POINT('Ctrl Pts',(19.6302776223641,-0.128565949173179,
117.852281715748));
#55156=CARTESIAN_POINT('Ctrl Pts',(19.5421188945232,0.388966926266299,117.883590757787));
#55157=CARTESIAN_POINT('Ctrl Pts',(19.3148713652829,0.727405617431935,117.908629650839));
#55158=CARTESIAN_POINT('Ctrl Pts',(19.0040420734761,0.991073319636765,117.933664807893));
#55159=CARTESIAN_POINT('Ctrl Pts',(18.4999415631754,1.13648535076679,117.964953921654));
#55160=CARTESIAN_POINT('Ctrl Pts',(17.8947899695678,0.96208712009206,118.002503188243));
#55161=CARTESIAN_POINT('Ctrl Pts',(17.4750732454252,0.492492667183828,118.040063661805));
#55162=CARTESIAN_POINT('Ctrl Pts',(17.3694300523301,-0.128850031555598,
118.077644813751));
#55163=CARTESIAN_POINT('Ctrl Pts',(17.6107331136891,-0.711582450772628,
118.115255756409));
#55164=CARTESIAN_POINT('Ctrl Pts',(18.125603119214,-1.07704534040567,118.152905757722));
#55165=CARTESIAN_POINT('Ctrl Pts',(18.7567934833813,-1.1125997163517,118.190603932222));
#55166=CARTESIAN_POINT('Ctrl Pts',(19.3110204717537,-0.806486790888208,
118.228359414069));
#55167=CARTESIAN_POINT('Ctrl Pts',(19.6179609922649,-0.25139504372414,118.266181161867));
#55168=CARTESIAN_POINT('Ctrl Pts',(19.5825391926542,0.383053875326996,118.304078231522));
#55169=CARTESIAN_POINT('Ctrl Pts',(19.2140816405097,0.902802898927527,118.342059291419));
#55170=CARTESIAN_POINT('Ctrl Pts',(18.7226880201779,1.10634814765537,118.373787735995));
#55171=CARTESIAN_POINT('Ctrl Pts',(18.3086085930042,1.09397848195709,118.39922099189));
#55172=CARTESIAN_POINT('Ctrl Pts',(18.0123540634614,0.999893884623254,118.418322678652));
#55173=CARTESIAN_POINT('Ctrl Pts',(17.7533626515011,0.82671918127196,118.437451496774));
#55174=CARTESIAN_POINT('Ctrl Pts',(17.5521199768519,0.588537547192838,118.456609257602));
#55175=CARTESIAN_POINT('Ctrl Pts',(17.4244911269899,0.303352454653029,118.475796244556));
#55176=CARTESIAN_POINT('Ctrl Pts',(17.3807273267954,-0.00639979916192339,
118.495014194405));
#55177=CARTESIAN_POINT('Ctrl Pts',(17.4244813580664,-0.316785015260581,
118.514263485987));
#55178=CARTESIAN_POINT('Ctrl Pts',(17.5313433203722,-0.555495775472718,
118.530332161233));
#55179=CARTESIAN_POINT('Ctrl Pts',(17.6540773517199,-0.723534213278567,
118.543203421388));
#55180=CARTESIAN_POINT('Ctrl Pts',(17.7992754119155,-0.872605010499798,
118.556086803096));
#55181=CARTESIAN_POINT('Ctrl Pts',(18.1045650757977,-1.07757525544991,118.578662058107));
#55182=CARTESIAN_POINT('Ctrl Pts',(18.6388883319623,-1.16886260969525,118.611002224315));
#55183=CARTESIAN_POINT('Ctrl Pts',(19.2429199720252,-0.91905243268689,118.649960624054));
#55184=CARTESIAN_POINT('Ctrl Pts',(19.5591656207873,-0.47353880214557,118.682557494984));
#55185=CARTESIAN_POINT('Ctrl Pts',(19.6312341819153,-0.107637891392649,
118.705448035791));
#55186=CARTESIAN_POINT('Ctrl Pts',(19.6284150057505,0.103886268314961,118.718548975396));
#55187=CARTESIAN_POINT('Ctrl Pts',(19.5958932860597,0.313538506666422,118.731664743549));
#55188=CARTESIAN_POINT('Ctrl Pts',(19.5004242033217,0.563000832640334,118.748085947437));
#55189=CARTESIAN_POINT('Ctrl Pts',(19.2432455304437,0.90628492536278,118.774418879784));
#55190=CARTESIAN_POINT('Ctrl Pts',(18.7589006628383,1.17453438898742,118.807447049227));
#55191=CARTESIAN_POINT('Ctrl Pts',(18.0920378754068,1.13752775310542,118.847267321706));
#55192=CARTESIAN_POINT('Ctrl Pts',(17.5444894219634,0.749580520515216,118.887280294004));
#55193=CARTESIAN_POINT('Ctrl Pts',(17.3292362808046,0.230633636407774,118.920790576476));
#55194=CARTESIAN_POINT('Ctrl Pts',(17.3423520957121,-0.207489759410931,
118.94770109744));
#55195=CARTESIAN_POINT('Ctrl Pts',(17.4252619681566,-0.469003909932179,
118.96456394793));
#55196=CARTESIAN_POINT('Ctrl Pts',(17.5203149088613,-0.634993651085502,
118.976390606938));
#55197=CARTESIAN_POINT('Ctrl Pts',(17.583983658906,-0.723534404469764,118.983155440389));
#55198=CARTESIAN_POINT('Ctrl Pts',(17.6538927305433,-0.807470935982133,
118.98992472633));
#55199=CARTESIAN_POINT('Ctrl Pts',(17.7520083028492,-0.902883777274666,
118.998394938564));
#55200=CARTESIAN_POINT('Ctrl Pts',(17.9290489907581,-1.0323314088204,119.01196453638));
#55201=CARTESIAN_POINT('Ctrl Pts',(18.1815801842383,-1.14541285633602,119.028960890958));
#55202=CARTESIAN_POINT('Ctrl Pts',(18.5112600172864,-1.19201555623084,119.049410990679));
#55203=CARTESIAN_POINT('Ctrl Pts',(18.8418328477004,-1.14540690441618,119.06991680109));
#55204=CARTESIAN_POINT('Ctrl Pts',(19.1474267825692,-1.00874033585996,119.090478520413));
#55205=CARTESIAN_POINT('Ctrl Pts',(19.4039443073445,-0.79220717736026,119.111097145673));
#55206=CARTESIAN_POINT('Ctrl Pts',(19.5910119718638,-0.51236647902462,119.131772830806));
#55207=CARTESIAN_POINT('Ctrl Pts',(19.6935905299409,-0.190752836459021,
119.152506800925));
#55208=CARTESIAN_POINT('Ctrl Pts',(19.7031388477895,0.147604935192541,119.173298766399));
#55209=CARTESIAN_POINT('Ctrl Pts',(19.6325566841645,0.421577620165869,119.190675097676));
#55210=CARTESIAN_POINT('Ctrl Pts',(19.5319409006659,0.622959778725234,119.204605562775));
#55211=CARTESIAN_POINT('Ctrl Pts',(19.3723111918508,0.855222362722365,119.22204381589));
#55212=CARTESIAN_POINT('Ctrl Pts',(19.0605236648718,1.11137648097883,119.24652741901));
#55213=CARTESIAN_POINT('Ctrl Pts',(18.557841901936,1.24883064038303,119.278143157038));
#55214=CARTESIAN_POINT('Ctrl Pts',(18.0406440600076,1.16864301673205,119.309897324764));
#55215=CARTESIAN_POINT('Ctrl Pts',(17.5993534519754,0.882949483972891,119.341791378035));
#55216=CARTESIAN_POINT('Ctrl Pts',(17.3119750925068,0.439968778678807,119.373826695856));
#55217=CARTESIAN_POINT('Ctrl Pts',(17.2302408898466,-0.0840529947305273,
119.406004587621));
#55218=CARTESIAN_POINT('Ctrl Pts',(17.3702629976844,-0.598088729393078,
119.438326182762));
#55219=CARTESIAN_POINT('Ctrl Pts',(17.6530460544461,-0.942889577582773,
119.465381607609));
#55220=CARTESIAN_POINT('Ctrl Pts',(17.9499828766226,-1.13203718581272,119.487098771073));
#55221=CARTESIAN_POINT('Ctrl Pts',(18.2803607508843,-1.25590365191542,119.508864774012));
#55222=CARTESIAN_POINT('Ctrl Pts',(18.729892524166,-1.27510737942024,119.536163929142));
#55223=CARTESIAN_POINT('Ctrl Pts',(19.2339592933469,-1.07479600420633,119.569070444908));
#55224=CARTESIAN_POINT('Ctrl Pts',(19.6139473273938,-0.684379105992577,
119.602125158036));
#55225=CARTESIAN_POINT('Ctrl Pts',(19.8021770921533,-0.170476841564033,
119.635328673285));
#55226=CARTESIAN_POINT('Ctrl Pts',(19.7639134649815,0.377926935064038,119.668681477351));
#55227=CARTESIAN_POINT('Ctrl Pts',(19.503839851328,0.865051934686931,119.70218396231));
#55228=CARTESIAN_POINT('Ctrl Pts',(19.0655180465322,1.20498508477827,119.735836419624));
#55229=CARTESIAN_POINT('Ctrl Pts',(18.524202098875,1.33680965848674,119.76963902964));
#55230=CARTESIAN_POINT('Ctrl Pts',(17.973771139484,1.23562343421845,119.803591891955));
#55231=CARTESIAN_POINT('Ctrl Pts',(17.5879069760352,0.970077900984119,119.832011116879));
#55232=CARTESIAN_POINT('Ctrl Pts',(17.3637280416863,0.675990163767077,119.85482156895));
#55233=CARTESIAN_POINT('Ctrl Pts',(17.2049255398143,0.341169720857323,119.877682007301));
#55234=CARTESIAN_POINT('Ctrl Pts',(17.1451722184405,-0.127573629778547,
119.906351243673));
#55235=CARTESIAN_POINT('Ctrl Pts',(17.310261401612,-0.672648178521142,119.940903882702));
#55236=CARTESIAN_POINT('Ctrl Pts',(17.6851761255204,-1.10460181805881,119.975605671829));
#55237=CARTESIAN_POINT('Ctrl Pts',(18.2060526856434,-1.34679126014451,120.0104560752));
#55238=CARTESIAN_POINT('Ctrl Pts',(18.7828550078472,-1.35513556170808,120.045454472915));
#55239=CARTESIAN_POINT('Ctrl Pts',(19.3149902028912,-1.12620240023457,120.08060013599));
#55240=CARTESIAN_POINT('Ctrl Pts',(19.7088387709082,-0.69810855233221,120.115892239948));
#55241=CARTESIAN_POINT('Ctrl Pts',(19.8942441582493,-0.144212137261873,
120.151329858863));
#55242=CARTESIAN_POINT('Ctrl Pts',(19.8370075803674,0.439473461448282,120.186911969597));
#55243=CARTESIAN_POINT('Ctrl Pts',(19.5451864564148,0.950924687748161,120.22263744994));
#55244=CARTESIAN_POINT('Ctrl Pts',(19.0680246080906,1.29995703510414,120.258505080578));
#55245=CARTESIAN_POINT('Ctrl Pts',(18.4876484020761,1.42413625094397,120.294513545472));
#55246=CARTESIAN_POINT('Ctrl Pts',(17.9049235301147,1.29995128236404,120.330661433598));
#55247=CARTESIAN_POINT('Ctrl Pts',(17.4219109382343,0.94724316719828,120.36694723955));
#55248=CARTESIAN_POINT('Ctrl Pts',(17.1239748622548,0.42606089295562,120.40336936399));
#55249=CARTESIAN_POINT('Ctrl Pts',(17.0646832076731,-0.173564467661854,
120.43992611466));
#55250=CARTESIAN_POINT('Ctrl Pts',(17.2561734622077,-0.747185474824163,
120.476615708097));
#55251=CARTESIAN_POINT('Ctrl Pts',(17.6667181243669,-1.19415105882015,120.513436271009));
#55252=CARTESIAN_POINT('Ctrl Pts',(18.2259712361402,-1.43528718231683,120.55038584204));
#55253=CARTESIAN_POINT('Ctrl Pts',(18.8370311234314,-1.4269354433336,120.587462370911));
#55254=CARTESIAN_POINT('Ctrl Pts',(19.3932495447825,-1.16885830485679,120.62466372221));
#55255=CARTESIAN_POINT('Ctrl Pts',(19.7968685982965,-0.70457726902139,120.661987673534));
#55256=CARTESIAN_POINT('Ctrl Pts',(19.9762240695575,-0.11403519053951,120.699431923752));
#55257=CARTESIAN_POINT('Ctrl Pts',(19.8984843651625,0.500186680137618,120.736994083826));
#55258=CARTESIAN_POINT('Ctrl Pts',(19.575656077446,1.03070741260493,120.774671696405));
#55259=CARTESIAN_POINT('Ctrl Pts',(19.0627604327755,1.38415482585726,120.812462202125));
#55260=CARTESIAN_POINT('Ctrl Pts',(18.4484458920318,1.49760672327847,120.850363008698));
#55261=CARTESIAN_POINT('Ctrl Pts',(17.8396489580402,1.34983590931418,120.888371367717));
#55262=CARTESIAN_POINT('Ctrl Pts',(17.3429428706895,0.96521497337526,120.926484611833));
#55263=CARTESIAN_POINT('Ctrl Pts',(17.045865677827,0.409809093734156,120.964699713595));
#55264=CARTESIAN_POINT('Ctrl Pts',(17.0014431624987,-0.220184717467978,
121.003014125745));
#55265=CARTESIAN_POINT('Ctrl Pts',(17.164424612689,-0.666099995461193,121.031821615483));
#55266=CARTESIAN_POINT('Ctrl Pts',(17.3434257995041,-0.919871476980275,
121.05105622202));
#55267=CARTESIAN_POINT('Ctrl Pts',(17.4797859795515,-1.07572928897003,121.063886410082));
#55268=CARTESIAN_POINT('Ctrl Pts',(17.7596234065678,-1.30908834442737,121.086360066906));
#55269=CARTESIAN_POINT('Ctrl Pts',(18.2520106540773,-1.50524820617466,121.118521093473));
#55270=CARTESIAN_POINT('Ctrl Pts',(18.8890624165871,-1.47853930079608,121.157201286479));
#55271=CARTESIAN_POINT('Ctrl Pts',(19.4608024223474,-1.19342203771302,121.19596496386));
#55272=CARTESIAN_POINT('Ctrl Pts',(19.8670946705987,-0.698578328455279,
121.234808961374));
#55273=CARTESIAN_POINT('Ctrl Pts',(20.0361439976898,-0.0797433644516521,
121.273729883387));
#55274=CARTESIAN_POINT('Ctrl Pts',(19.9375081708051,0.555375415482859,121.312724375624));
#55275=CARTESIAN_POINT('Ctrl Pts',(19.5874251537738,1.09577408462559,121.351788983929));
#55276=CARTESIAN_POINT('Ctrl Pts',(19.0462304801139,1.44664725684484,121.390920231817));
#55277=CARTESIAN_POINT('Ctrl Pts',(18.4078945414795,1.54602243253516,121.430114584083));
#55278=CARTESIAN_POINT('Ctrl Pts',(17.7836988323502,1.37574232630369,121.46936846982));
#55279=CARTESIAN_POINT('Ctrl Pts',(17.282784413028,0.964774261392473,121.508678276351));
#55280=CARTESIAN_POINT('Ctrl Pts',(16.9930369427572,0.384280279752719,121.548040351931));
#55281=CARTESIAN_POINT('Ctrl Pts',(16.965632387849,-0.264730861667821,121.587451011704));
#55282=CARTESIAN_POINT('Ctrl Pts',(17.2059822704094,-0.869015615574065,
121.62690653034));
#55283=CARTESIAN_POINT('Ctrl Pts',(17.6726767135541,-1.32289404488312,121.666403167446));
#55284=CARTESIAN_POINT('Ctrl Pts',(18.2846316707479,-1.54677468466741,121.705937127496));
#55285=CARTESIAN_POINT('Ctrl Pts',(18.9352078852143,-1.50113156051487,121.745504642789));
#55286=CARTESIAN_POINT('Ctrl Pts',(19.5108283377225,-1.19351370721864,121.785101820707));
#55287=CARTESIAN_POINT('Ctrl Pts',(19.9108571524216,-0.677265469818324,
121.824724937988));
#55288=CARTESIAN_POINT('Ctrl Pts',(20.0652157840296,-0.0423184316138819,
121.864369898394));
#55289=CARTESIAN_POINT('Ctrl Pts',(19.9467037274954,0.600613015659342,121.904033165255));
#55290=CARTESIAN_POINT('Ctrl Pts',(19.5757992709283,1.13923860750134,121.94371053936));
#55291=CARTESIAN_POINT('Ctrl Pts',(19.0170903691283,1.47948299020874,121.98339826705));
#55292=CARTESIAN_POINT('Ctrl Pts',(18.3680365032212,1.56185385513211,122.023092428396));
#55293=CARTESIAN_POINT('Ctrl Pts',(17.7419081841277,1.37192185757288,122.062789067507));
#55294=CARTESIAN_POINT('Ctrl Pts',(17.2479880852714,0.942825489960859,122.102484313511));
#55295=CARTESIAN_POINT('Ctrl Pts',(16.9724506261291,0.349491856500285,122.142174250389));
#55296=CARTESIAN_POINT('Ctrl Pts',(16.9632975544238,-0.304482856222713,
122.181854925629));
#55297=CARTESIAN_POINT('Ctrl Pts',(17.2219756104425,-0.90495722201614,122.221522510184));
#55298=CARTESIAN_POINT('Ctrl Pts',(17.703150736639,-1.34720967711664,122.261173032983));
#55299=CARTESIAN_POINT('Ctrl Pts',(18.32267005537,-1.55424124071767,122.300802661018));
#55300=CARTESIAN_POINT('Ctrl Pts',(18.9723111111196,-1.49021086379301,122.340407526305));
#55301=CARTESIAN_POINT('Ctrl Pts',(19.5387259317724,-1.16665041070326,122.379983728909));
#55302=CARTESIAN_POINT('Ctrl Pts',(19.9232635108214,-0.640390240190918,
122.41952751821));
#55303=CARTESIAN_POINT('Ctrl Pts',(20.0591820384592,-0.00354720571782957,
122.459034985586));
#55304=CARTESIAN_POINT('Ctrl Pts',(19.9232660830292,0.632615020340979,122.498502456349));
#55305=CARTESIAN_POINT('Ctrl Pts',(19.5397804872933,1.15720317221413,122.537926016389));
#55306=CARTESIAN_POINT('Ctrl Pts',(18.976169061755,1.47900616711341,122.57730217062));
#55307=CARTESIAN_POINT('Ctrl Pts',(18.3311000990434,1.54244114772495,122.616626980227));
#55308=CARTESIAN_POINT('Ctrl Pts',(17.7172503357923,1.33717049420449,122.65589694091));
#55309=CARTESIAN_POINT('Ctrl Pts',(17.2414907601859,0.899686660583994,122.695108360465));
#55310=CARTESIAN_POINT('Ctrl Pts',(16.9863250205813,0.307053962090209,122.734257662629));
#55311=CARTESIAN_POINT('Ctrl Pts',(16.9944497248883,-0.265604990902867,
122.768998723032));
#55312=CARTESIAN_POINT('Ctrl Pts',(17.1712479141773,-0.726942161622184,
122.799352272066));
#55313=CARTESIAN_POINT('Ctrl Pts',(17.5097094866836,-1.1784234221635,122.833999798576));
#55314=CARTESIAN_POINT('Ctrl Pts',(18.1440046231468,-1.52895577946613,122.877227151694));
#55315=CARTESIAN_POINT('Ctrl Pts',(19.0103596682388,-1.47993008996887,122.928960969768));
#55316=CARTESIAN_POINT('Ctrl Pts',(19.7156188499506,-0.979014184639401,
122.980547803872));
#55317=CARTESIAN_POINT('Ctrl Pts',(20.0453801510908,-0.182081354440587,
123.03198007533));
#55318=CARTESIAN_POINT('Ctrl Pts',(19.9009658784246,0.665665387675089,123.083250264192));
#55319=CARTESIAN_POINT('Ctrl Pts',(19.4248338794238,1.19762189380074,123.125834318843));
#55320=CARTESIAN_POINT('Ctrl Pts',(18.9192728107669,1.42256593967437,123.159813367155));
#55321=CARTESIAN_POINT('Ctrl Pts',(18.5245231164848,1.4787721179211,123.184310457398));
#55322=CARTESIAN_POINT('Ctrl Pts',(18.1454638254786,1.43075212555668,123.207825338745));
#55323=CARTESIAN_POINT('Ctrl Pts',(17.6907015228179,1.25302600903987,123.237875289869));
#55324=CARTESIAN_POINT('Ctrl Pts',(17.2340011183052,0.829040578783695,123.275344392595));
#55325=CARTESIAN_POINT('Ctrl Pts',(17.036580919693,0.240275284929825,123.3126849899));
#55326=CARTESIAN_POINT('Ctrl Pts',(17.0615849896374,-0.243150591543408,
123.342478462658));
#55327=CARTESIAN_POINT('Ctrl Pts',(17.2032609087076,-0.705038732123995,
123.372218231113));
#55328=CARTESIAN_POINT('Ctrl Pts',(17.5878551543339,-1.18711482918302,123.409291524378));
#55329=CARTESIAN_POINT('Ctrl Pts',(18.2106400712898,-1.44898576843933,123.44991921019));
#55330=CARTESIAN_POINT('Ctrl Pts',(18.8141776698684,-1.42578153316616,123.486729147975));
#55331=CARTESIAN_POINT('Ctrl Pts',(19.3107890371302,-1.20916212882085,123.519760499083));
#55332=CARTESIAN_POINT('Ctrl Pts',(19.6927353972249,-0.826888177330121,
123.552692753465));
#55333=CARTESIAN_POINT('Ctrl Pts',(19.9079783510014,-0.333205350440447,
123.58552446981));
#55334=CARTESIAN_POINT('Ctrl Pts',(19.927910114824,0.203440614612126,123.618254093443));
#55335=CARTESIAN_POINT('Ctrl Pts',(19.7509532260585,0.708563531543187,123.650880447743));
#55336=CARTESIAN_POINT('Ctrl Pts',(19.4608602251756,1.04556155423777,123.677981648566));
#55337=CARTESIAN_POINT('Ctrl Pts',(19.1676482101075,1.23701496091332,123.699609780472));
#55338=CARTESIAN_POINT('Ctrl Pts',(18.7910679570069,1.39369644218677,123.724801049022));
#55339=CARTESIAN_POINT('Ctrl Pts',(18.2247967647374,1.42170073442178,123.758885465202));
#55340=CARTESIAN_POINT('Ctrl Pts',(17.6899503199116,1.1635842287656,123.794602768893));
#55341=CARTESIAN_POINT('Ctrl Pts',(17.3755915425233,0.823902495683255,123.823078658873));
#55342=CARTESIAN_POINT('Ctrl Pts',(17.2102573337398,0.520040275543171,123.844386427488));
#55343=CARTESIAN_POINT('Ctrl Pts',(17.095967357383,0.0736009166210867,123.872730605635));
#55344=CARTESIAN_POINT('Ctrl Pts',(17.1620133383056,-0.450381505464488,
123.904505832421));
#55345=CARTESIAN_POINT('Ctrl Pts',(17.4696117223982,-0.938632889638676,
123.939664796233));
#55346=CARTESIAN_POINT('Ctrl Pts',(17.9029622950757,-1.25855076196019,123.972507589326));
#55347=CARTESIAN_POINT('Ctrl Pts',(18.4480459034613,-1.39083552515014,124.006531983721));
#55348=CARTESIAN_POINT('Ctrl Pts',(19.0183329635533,-1.28540085920782,124.041718831028));
#55349=CARTESIAN_POINT('Ctrl Pts',(19.4541943928961,-0.984922969711832,
124.073838648615));
#55350=CARTESIAN_POINT('Ctrl Pts',(19.6682715737307,-0.67104133868322,124.097112291097));
#55351=CARTESIAN_POINT('Ctrl Pts',(19.7868416138341,-0.382011184973219,
124.116465835797));
#55352=CARTESIAN_POINT('Ctrl Pts',(19.845095426036,-0.0889792271213038,
124.134815712575));
#55353=CARTESIAN_POINT('Ctrl Pts',(19.8133776059636,0.285969865030816,124.157928489657));
#55354=CARTESIAN_POINT('Ctrl Pts',(19.6795064045911,0.636485482650236,124.180974858546));
#55355=CARTESIAN_POINT('Ctrl Pts',(19.4544658023414,0.935380714529392,124.203954899115));
#55356=CARTESIAN_POINT('Ctrl Pts',(19.1563653681889,1.15962510660347,124.226868327498));
#55357=CARTESIAN_POINT('Ctrl Pts',(18.8377643876985,1.28119223747043,124.247811293649));
#55358=CARTESIAN_POINT('Ctrl Pts',(18.5321242045092,1.31762067856076,124.266801681851));
#55359=CARTESIAN_POINT('Ctrl Pts',(18.1649796321115,1.28429399639958,124.289540148812));
#55360=CARTESIAN_POINT('Ctrl Pts',(17.7362231944242,1.09949023306847,124.317869313244));
#55361=CARTESIAN_POINT('Ctrl Pts',(17.3588965090123,0.688544810591405,124.351714091216));
#55362=CARTESIAN_POINT('Ctrl Pts',(17.1830862730632,0.161768183835377,124.385408663042));
#55363=CARTESIAN_POINT('Ctrl Pts',(17.2375391699697,-0.388462801364577,
124.418953209553));
#55364=CARTESIAN_POINT('Ctrl Pts',(17.510749604725,-0.866293220470127,124.452347979479));
#55365=CARTESIAN_POINT('Ctrl Pts',(17.953313706052,-1.18941945391201,124.485593341375));
#55366=CARTESIAN_POINT('Ctrl Pts',(18.4868547743004,-1.30308143479277,124.51868975568));
#55367=CARTESIAN_POINT('Ctrl Pts',(19.0178962204122,-1.18942424606218,124.551637788857));
#55368=CARTESIAN_POINT('Ctrl Pts',(19.4542337078503,-0.8702144890527,124.584438104991));
#55369=CARTESIAN_POINT('Ctrl Pts',(19.7209361731848,-0.402730819941738,
124.617091470052));
#55370=CARTESIAN_POINT('Ctrl Pts',(19.7732021435748,0.130517736745286,124.649598749166));
#55371=CARTESIAN_POINT('Ctrl Pts',(19.6038673633271,0.636337480625157,124.681960907071));
#55372=CARTESIAN_POINT('Ctrl Pts',(19.244310467946,1.0271307853851,124.714179006478));
#55373=CARTESIAN_POINT('Ctrl Pts',(18.7586597506273,1.23605144177733,124.746254207572));
#55374=CARTESIAN_POINT('Ctrl Pts',(18.2323678346202,1.22842456764535,124.778187767811));
#55375=CARTESIAN_POINT('Ctrl Pts',(17.7571886611326,1.00747814552238,124.809981041022));
#55376=CARTESIAN_POINT('Ctrl Pts',(17.4151961591713,0.613446990910202,124.841635476325));
#55377=CARTESIAN_POINT('Ctrl Pts',(17.2646251988404,0.11626338066299,124.873152616656));
#55378=CARTESIAN_POINT('Ctrl Pts',(17.3299739672999,-0.396839428590113,
124.904534097586));
#55379=CARTESIAN_POINT('Ctrl Pts',(17.5980462947708,-0.836615880994796,
124.935781647363));
#55380=CARTESIAN_POINT('Ctrl Pts',(18.0205671134112,-1.12731152415149,124.966897085264));
#55381=CARTESIAN_POINT('Ctrl Pts',(18.5228589289931,-1.21969167859972,124.997882320446));
#55382=CARTESIAN_POINT('Ctrl Pts',(19.0170220921567,-1.09935899300576,125.028739349874));
#55383=CARTESIAN_POINT('Ctrl Pts',(19.4172956623671,-0.788959348815974,
125.059470256914));
#55384=CARTESIAN_POINT('Ctrl Pts',(19.6549180267179,-0.343945996706955,
125.090077211201));
#55385=CARTESIAN_POINT('Ctrl Pts',(19.6899160842551,0.157308971986261,125.120562466777));
#55386=CARTESIAN_POINT('Ctrl Pts',(19.5178066612108,0.627294647194249,125.150928360418));
#55387=CARTESIAN_POINT('Ctrl Pts',(19.1700918544773,0.984613592532787,125.181177309389));
#55388=CARTESIAN_POINT('Ctrl Pts',(18.7085131498763,1.16805288175899,125.211311809549));
#55389=CARTESIAN_POINT('Ctrl Pts',(18.2141093210495,1.14704615240416,125.241334435139));
#55390=CARTESIAN_POINT('Ctrl Pts',(17.7730146416868,0.926743182603541,125.271247836795));
#55391=CARTESIAN_POINT('Ctrl Pts',(17.4614821276217,0.546851681684302,125.301054739329));
#55392=CARTESIAN_POINT('Ctrl Pts',(17.3327303667907,0.0744996228417085,
125.330757939393));
#55393=CARTESIAN_POINT('Ctrl Pts',(17.4078770669085,-0.407601769713727,
125.360360303038));
#55394=CARTESIAN_POINT('Ctrl Pts',(17.6724992810162,-0.815611229448775,
125.389864765497));
#55395=CARTESIAN_POINT('Ctrl Pts',(18.0793755906884,-1.0791058017612,125.419274329063));
#55396=CARTESIAN_POINT('Ctrl Pts',(18.5568918796206,-1.15320571445106,125.448592060433));
#55397=CARTESIAN_POINT('Ctrl Pts',(19.0216174451001,-1.02619433748491,125.47782108828));
#55398=CARTESIAN_POINT('Ctrl Pts',(19.3928480017872,-0.721344483540626,
125.506964600284));
#55399=CARTESIAN_POINT('Ctrl Pts',(19.6065865223145,-0.29267161003856,125.536025842907));
#55400=CARTESIAN_POINT('Ctrl Pts',(19.6265455959889,0.184613405993531,125.565008119228));
#55401=CARTESIAN_POINT('Ctrl Pts',(19.4502857848642,0.627267625324512,125.593914785862));
#55402=CARTESIAN_POINT('Ctrl Pts',(19.1094565344714,0.958497326481144,125.622749250498));
#55403=CARTESIAN_POINT('Ctrl Pts',(18.6641306988289,1.12124490215563,125.65151496845));
#55404=CARTESIAN_POINT('Ctrl Pts',(18.1922438001048,1.08798886479353,125.680215442352));
#55405=CARTESIAN_POINT('Ctrl Pts',(17.7759904730407,0.865378727907893,125.70885422014));
#55406=CARTESIAN_POINT('Ctrl Pts',(17.4875467958782,0.492928571561681,125.737434891433));
#55407=CARTESIAN_POINT('Ctrl Pts',(17.3765912962239,0.0360231116649436,
125.765961085237));
#55408=CARTESIAN_POINT('Ctrl Pts',(17.4617752953106,-0.425529155060106,
125.794436465925));
#55409=CARTESIAN_POINT('Ctrl Pts',(17.7276023914822,-0.811397469264803,
125.822864733026));
#55410=CARTESIAN_POINT('Ctrl Pts',(18.1272364572306,-1.05466977543198,125.851249619116));
#55411=CARTESIAN_POINT('Ctrl Pts',(18.5907303019158,-1.11342078422065,125.879594886123));
#55412=CARTESIAN_POINT('Ctrl Pts',(19.0372330501214,-0.977914032009643,
125.9079043228));
#55413=CARTESIAN_POINT('Ctrl Pts',(19.3890522206571,-0.672205338262385,
125.93618174058));
#55414=CARTESIAN_POINT('Ctrl Pts',(19.5851322651224,-0.249885254342319,
125.964430973193));
#55415=CARTESIAN_POINT('Ctrl Pts',(19.5916177912335,0.215288095109658,125.992655874655));
#55416=CARTESIAN_POINT('Ctrl Pts',(19.4076799277922,0.642232516558101,126.02086031546));
#55417=CARTESIAN_POINT('Ctrl Pts',(19.0656071912909,0.956631975295786,126.049048179947));
#55418=CARTESIAN_POINT('Ctrl Pts',(18.6251546527486,1.1038329828714,126.07722336208));
#55419=CARTESIAN_POINT('Ctrl Pts',(18.1631369444732,1.05831622648696,126.105389764899));
#55420=CARTESIAN_POINT('Ctrl Pts',(17.7600722808915,0.828106591669271,126.133551298519));
#55421=CARTESIAN_POINT('Ctrl Pts',(17.4861931301989,0.453362374694559,126.161711876545));
#55422=CARTESIAN_POINT('Ctrl Pts',(17.3892461185869,-0.000608579703322207,
126.189875413034));
#55423=CARTESIAN_POINT('Ctrl Pts',(17.4861934126935,-0.45469525474382,126.218045818642));
#55424=CARTESIAN_POINT('Ctrl Pts',(17.7602536761873,-0.829727747487646,
126.246226999653));
#55425=CARTESIAN_POINT('Ctrl Pts',(18.1637977951782,-1.06023867129499,126.274422856165));
#55426=CARTESIAN_POINT('Ctrl Pts',(18.6266008887622,-1.10585668977637,126.302637278628));
#55427=CARTESIAN_POINT('Ctrl Pts',(19.0680252619495,-0.958355862859884,
126.33087414464));
#55428=CARTESIAN_POINT('Ctrl Pts',(19.4110278768796,-0.643133784314882,
126.359137315337));
#55429=CARTESIAN_POINT('Ctrl Pts',(19.5955669183692,-0.214853191351468,
126.387430634005));
#55430=CARTESIAN_POINT('Ctrl Pts',(19.5890811732739,0.252008008583668,126.415757924456));
#55431=CARTESIAN_POINT('Ctrl Pts',(19.3922180527628,0.676069561741979,126.444122988192));
#55432=CARTESIAN_POINT('Ctrl Pts',(19.038806518154,0.983192293191261,126.47252960012));
#55433=CARTESIAN_POINT('Ctrl Pts',(18.5900631360178,1.11940281866746,126.50098150721));
#55434=CARTESIAN_POINT('Ctrl Pts',(18.1240214367007,1.06035134340115,126.529482422973));
#55435=CARTESIAN_POINT('Ctrl Pts',(17.7219999728875,0.815652189115242,126.558036033249));
#55436=CARTESIAN_POINT('Ctrl Pts',(17.4544565122385,0.42732974030796,126.586645980413));
#55437=CARTESIAN_POINT('Ctrl Pts',(17.3686682099376,-0.0373706799791392,
126.615315883455));
#55438=CARTESIAN_POINT('Ctrl Pts',(17.4804111341263,-0.497601968494626,
126.644049291652));
#55439=CARTESIAN_POINT('Ctrl Pts',(17.7710524624981,-0.872926042665041,
126.672849763267));
#55440=CARTESIAN_POINT('Ctrl Pts',(18.1906784128292,-1.09736508436974,126.701720713779));
#55441=CARTESIAN_POINT('Ctrl Pts',(18.6665693810468,-1.13091363907518,126.73066569576));
#55442=CARTESIAN_POINT('Ctrl Pts',(19.115900304304,-0.966754134360276,126.759687863605));
#55443=CARTESIAN_POINT('Ctrl Pts',(19.4025342696002,-0.688135191455954,
126.783940470337));
#55444=CARTESIAN_POINT('Ctrl Pts',(19.548921654941,-0.40898722136763,126.803384174727));
#55445=CARTESIAN_POINT('Ctrl Pts',(19.634493180543,-0.10514408540288,126.822856841586));
#55446=CARTESIAN_POINT('Ctrl Pts',(19.6177649185308,0.296581417751861,126.847251669214));
#55447=CARTESIAN_POINT('Ctrl Pts',(19.4017808130667,0.729742583298161,126.876616113372));
#55448=CARTESIAN_POINT('Ctrl Pts',(19.0265757427209,1.03788810065477,126.906073797672));
#55449=CARTESIAN_POINT('Ctrl Pts',(18.5566758014723,1.16633154684977,126.935628014866));
#55450=CARTESIAN_POINT('Ctrl Pts',(18.0736913341831,1.09139777528755,126.965281594702));
#55451=CARTESIAN_POINT('Ctrl Pts',(17.6620120612613,0.824814395466043,126.995037511174));
#55452=CARTESIAN_POINT('Ctrl Pts',(17.3941799549046,0.411881837949739,127.024898556795));
#55453=CARTESIAN_POINT('Ctrl Pts',(17.3180870575981,-0.076187288283962,
127.05486751266));
#55454=CARTESIAN_POINT('Ctrl Pts',(17.4484565420247,-0.554528037140921,
127.084947054201));
#55455=CARTESIAN_POINT('Ctrl Pts',(17.764010774281,-0.939345893009087,127.115139797876));
#55456=CARTESIAN_POINT('Ctrl Pts',(18.2109253092811,-1.16257046672283,127.145448275684));
#55457=CARTESIAN_POINT('Ctrl Pts',(18.7119822511381,-1.18387264939932,127.175874945546));
#55458=CARTESIAN_POINT('Ctrl Pts',(19.1798875199966,-0.997932182564281,
127.206422183755));
#55459=CARTESIAN_POINT('Ctrl Pts',(19.5324518600497,-0.635646414421749,
127.237092283841));
#55460=CARTESIAN_POINT('Ctrl Pts',(19.7070045821325,-0.15902031214536,127.267887456223));
#55461=CARTESIAN_POINT('Ctrl Pts',(19.6715152795569,0.349422683108497,127.298809830743));
#55462=CARTESIAN_POINT('Ctrl Pts',(19.4304489650515,0.800905801272552,127.329861432512));
#55463=CARTESIAN_POINT('Ctrl Pts',(19.0242953873212,1.11587711326151,127.361044250206));
#55464=CARTESIAN_POINT('Ctrl Pts',(18.5227859928513,1.23800718975454,127.392360076625));
#55465=CARTESIAN_POINT('Ctrl Pts',(18.0129472939614,1.14424745798179,127.423810814418));
#55466=CARTESIAN_POINT('Ctrl Pts',(17.5840172876535,0.849149894711047,127.455397873974));
#55467=CARTESIAN_POINT('Ctrl Pts',(17.3118406201315,0.402652849536599,127.487123453883));
#55468=CARTESIAN_POINT('Ctrl Pts',(17.2454720166539,-0.118349922486156,
127.518987753904));
#55469=CARTESIAN_POINT('Ctrl Pts',(17.3984032330202,-0.623252153014087,
127.550994556485));
#55470=CARTESIAN_POINT('Ctrl Pts',(17.7456488662068,-1.02342067777811,127.58314143777));
#55471=CARTESIAN_POINT('Ctrl Pts',(18.2284245791308,-1.2478499399624,127.615434837012));
#55472=CARTESIAN_POINT('Ctrl Pts',(18.7627797364581,-1.25558862553399,127.647868301601));
#55473=CARTESIAN_POINT('Ctrl Pts',(19.2563109695001,-1.04333545914346,127.680455449859));
#55474=CARTESIAN_POINT('Ctrl Pts',(19.6216681619718,-0.646528379290638,
127.713175673656));
#55475=CARTESIAN_POINT('Ctrl Pts',(19.7927328538191,-0.132281528567945,
127.746058739306));
#55476=CARTESIAN_POINT('Ctrl Pts',(19.7503141195651,0.318711829041913,127.773584129304));
#55477=CARTESIAN_POINT('Ctrl Pts',(19.6053572776214,0.646435247116302,127.795653000386));
#55478=CARTESIAN_POINT('Ctrl Pts',(19.4462354220477,0.865492620926237,127.812264237419));
#55479=CARTESIAN_POINT('Ctrl Pts',(19.2457948002735,1.04692682939879,127.828924915749));
#55480=CARTESIAN_POINT('Ctrl Pts',(19.0155264002248,1.18188573320303,127.845613783594));
#55481=CARTESIAN_POINT('Ctrl Pts',(18.7628986552341,1.26490607478793,127.862310718442));
#55482=CARTESIAN_POINT('Ctrl Pts',(18.5810921207593,1.28450653733517,127.873458175477));
#55483=CARTESIAN_POINT('Ctrl Pts',(18.4867961500699,1.28530018715607,127.879040201486));
#55484=CARTESIAN_POINT('Ctrl Pts',(18.4876785229654,1.35973827479612,112.700349483895));
#55485=CARTESIAN_POINT('Ctrl Pts',(18.338278791091,1.35848083962102,112.709193479852));
#55486=CARTESIAN_POINT('Ctrl Pts',(18.1480053653849,1.32809629852819,112.721061171528));
#55487=CARTESIAN_POINT('Ctrl Pts',(17.8839969407007,1.22542744763376,112.73889627186));
#55488=CARTESIAN_POINT('Ctrl Pts',(17.6791187447654,1.10539854696858,112.753746837641));
#55489=CARTESIAN_POINT('Ctrl Pts',(17.4646853083375,0.911300230451853,112.771570316604));
#55490=CARTESIAN_POINT('Ctrl Pts',(17.2932741920643,0.675669450544188,112.789446398643));
#55491=CARTESIAN_POINT('Ctrl Pts',(17.1360309787953,0.320121093800881,112.813390160947));
#55492=CARTESIAN_POINT('Ctrl Pts',(17.0894953340232,-0.170507827027364,
112.843336784654));
#55493=CARTESIAN_POINT('Ctrl Pts',(17.2766257739384,-0.734670630418044,
112.879400942648));
#55494=CARTESIAN_POINT('Ctrl Pts',(17.6806702631371,-1.17437363669764,112.915626922413));
#55495=CARTESIAN_POINT('Ctrl Pts',(18.2307083272979,-1.41134855642679,112.951951982645));
#55496=CARTESIAN_POINT('Ctrl Pts',(18.8314790313439,-1.40324601833503,112.988419852557));
#55497=CARTESIAN_POINT('Ctrl Pts',(19.3786171248065,-1.14937703929912,113.025002743964));
#55498=CARTESIAN_POINT('Ctrl Pts',(19.7755321622389,-0.69277837996112,113.06171356028));
#55499=CARTESIAN_POINT('Ctrl Pts',(19.9519587360096,-0.111935044059312,
113.098541071133));
#55500=CARTESIAN_POINT('Ctrl Pts',(19.8754964114079,0.492238686716583,113.135489585637));
#55501=CARTESIAN_POINT('Ctrl Pts',(19.5579256638734,1.01412235273271,113.172553147416));
#55502=CARTESIAN_POINT('Ctrl Pts',(19.0533449396798,1.36184827886875,113.209731746827));
#55503=CARTESIAN_POINT('Ctrl Pts',(18.4489214934587,1.47348302587511,113.247022170108));
#55504=CARTESIAN_POINT('Ctrl Pts',(17.8498617671385,1.328077180479,113.284422590151));
#55505=CARTESIAN_POINT('Ctrl Pts',(17.3610409118715,0.949582216371434,113.32193043636));
#55506=CARTESIAN_POINT('Ctrl Pts',(17.0686356732366,0.402912605142576,113.359543389231));
#55507=CARTESIAN_POINT('Ctrl Pts',(17.0249018837744,-0.217196012200376,
113.397258901394));
#55508=CARTESIAN_POINT('Ctrl Pts',(17.2388349234317,-0.802630231903418,
113.435074404672));
#55509=CARTESIAN_POINT('Ctrl Pts',(17.6743443357727,-1.25077220769488,113.47298729979));
#55510=CARTESIAN_POINT('Ctrl Pts',(18.2563708833245,-1.48251999814763,113.510994797665));
#55511=CARTESIAN_POINT('Ctrl Pts',(18.883788180464,-1.45626180229461,113.54909429881));
#55512=CARTESIAN_POINT('Ctrl Pts',(19.4470878187195,-1.17536327214856,113.587282715003));
#55513=CARTESIAN_POINT('Ctrl Pts',(19.8474132957324,-0.687788270612358,
113.625557419335));
#55514=CARTESIAN_POINT('Ctrl Pts',(20.0140399050535,-0.0779171052049972,
113.663915285566));
#55515=CARTESIAN_POINT('Ctrl Pts',(19.9168245873902,0.548151296346475,113.702353379261));
#55516=CARTESIAN_POINT('Ctrl Pts',(19.5716780905909,1.08094531644977,113.740868668601));
#55517=CARTESIAN_POINT('Ctrl Pts',(19.0379862034942,1.42700170662234,113.779457936887));
#55518=CARTESIAN_POINT('Ctrl Pts',(18.5132840325881,1.5086380779085,113.811674845049));
#55519=CARTESIAN_POINT('Ctrl Pts',(18.1004282686362,1.44105976086287,113.837482080291));
#55520=CARTESIAN_POINT('Ctrl Pts',(17.7101473882012,1.28940494040579,113.863311335357));
#55521=CARTESIAN_POINT('Ctrl Pts',(17.2981783514831,0.951509020667204,113.895638332265));
#55522=CARTESIAN_POINT('Ctrl Pts',(17.0121782076903,0.378491346568276,113.934491682164));
#55523=CARTESIAN_POINT('Ctrl Pts',(16.9850947717721,-0.262273826574141,
113.973402866311));
#55524=CARTESIAN_POINT('Ctrl Pts',(17.2224477564689,-0.859069243423921,
114.012368441823));
#55525=CARTESIAN_POINT('Ctrl Pts',(17.6834527470367,-1.30743766470174,114.051384974311));
#55526=CARTESIAN_POINT('Ctrl Pts',(18.2881276456927,-1.52867649004814,114.090449046825));
#55527=CARTESIAN_POINT('Ctrl Pts',(18.9311491263506,-1.48358202333768,114.129557166494));
#55528=CARTESIAN_POINT('Ctrl Pts',(19.5002573154791,-1.17946619024642,114.168705781698));
#55529=CARTESIAN_POINT('Ctrl Pts',(19.895883518136,-0.668933671693989,114.207891428952));
#55530=CARTESIAN_POINT('Ctrl Pts',(20.0486043834432,-0.0408103026870864,
114.247110440653));
#55531=CARTESIAN_POINT('Ctrl Pts',(19.9313560547634,0.595409226935658,114.286359317187));
#55532=CARTESIAN_POINT('Ctrl Pts',(19.5642318343119,1.12858247956978,114.325634401683));
#55533=CARTESIAN_POINT('Ctrl Pts',(19.0110221780777,1.46550417236436,114.364932073146));
#55534=CARTESIAN_POINT('Ctrl Pts',(18.3681434811919,1.54711317103822,114.404248695611));
#55535=CARTESIAN_POINT('Ctrl Pts',(17.7477597391124,1.35894684363908,114.443580607611));
#55536=CARTESIAN_POINT('Ctrl Pts',(17.2581993100081,0.93367008885888,114.482924143866));
#55537=CARTESIAN_POINT('Ctrl Pts',(16.9849907759577,0.345400833559539,114.522275637151));
#55538=CARTESIAN_POINT('Ctrl Pts',(16.9758869025945,-0.303213715649527,
114.561631392287));
#55539=CARTESIAN_POINT('Ctrl Pts',(17.2325184431462,-0.899000003070434,
114.600987756475));
#55540=CARTESIAN_POINT('Ctrl Pts',(17.7100628186082,-1.3379326372978,114.640340988896));
#55541=CARTESIAN_POINT('Ctrl Pts',(18.3251652493023,-1.54355290685385,114.679687519473));
#55542=CARTESIAN_POINT('Ctrl Pts',(18.8628342525488,-1.49050064839209,114.712467468208));
#55543=CARTESIAN_POINT('Ctrl Pts',(19.2518081213493,-1.319262658196,114.738684473466));
#55544=CARTESIAN_POINT('Ctrl Pts',(19.5968527931672,-1.07127762690712,114.764896190921));
#55545=CARTESIAN_POINT('Ctrl Pts',(19.9154275427713,-0.63545754250494,114.797649532843));
#55546=CARTESIAN_POINT('Ctrl Pts',(20.0505695810008,-0.00220756764337195,
114.836932305889));
#55547=CARTESIAN_POINT('Ctrl Pts',(19.9154136835604,0.630564901895597,114.876189922281));
#55548=CARTESIAN_POINT('Ctrl Pts',(19.5338400364215,1.15258304952519,114.91541892072));
#55549=CARTESIAN_POINT('Ctrl Pts',(18.9727998510443,1.47293614770067,114.954615610741));
#55550=CARTESIAN_POINT('Ctrl Pts',(18.3304348019443,1.53614587402187,114.99377648997));
#55551=CARTESIAN_POINT('Ctrl Pts',(17.7188795785189,1.33165301578999,115.032897926425));
#55552=CARTESIAN_POINT('Ctrl Pts',(17.2447460413749,0.895715527281768,115.071976520637));
#55553=CARTESIAN_POINT('Ctrl Pts',(16.9902588839041,0.304783064849235,115.111008561568));
#55554=CARTESIAN_POINT('Ctrl Pts',(16.998448612415,-0.266235065591532,115.145659623941));
#55555=CARTESIAN_POINT('Ctrl Pts',(17.1746492311271,-0.726807957150069,
115.175944304194));
#55556=CARTESIAN_POINT('Ctrl Pts',(17.3649071445344,-0.979853975065223,
115.195395177983));
#55557=CARTESIAN_POINT('Ctrl Pts',(17.5179391530716,-1.12232983850705,115.208353638872));
#55558=CARTESIAN_POINT('Ctrl Pts',(17.5991280987468,-1.18808194474613,115.214831558541));
#55559=CARTESIAN_POINT('Ctrl Pts',(17.6847833163635,-1.2479102131603,115.221307669249));
#55560=CARTESIAN_POINT('Ctrl Pts',(17.8639071380312,-1.35535581298678,115.234257210543));
#55561=CARTESIAN_POINT('Ctrl Pts',(18.1591868534977,-1.4680197646283,115.253667690937));
#55562=CARTESIAN_POINT('Ctrl Pts',(18.5785806683425,-1.50338131849235,115.27952203358));
#55563=CARTESIAN_POINT('Ctrl Pts',(18.9910229601307,-1.42130509597836,115.305346731328));
#55564=CARTESIAN_POINT('Ctrl Pts',(19.3639961781648,-1.22854103830715,115.331142672617));
#55565=CARTESIAN_POINT('Ctrl Pts',(19.6690154415896,-0.940296747232436,
115.356907307457));
#55566=CARTESIAN_POINT('Ctrl Pts',(19.8814233359884,-0.579498862185678,
115.382641004355));
#55567=CARTESIAN_POINT('Ctrl Pts',(20.0218052305324,-0.039065010395108,
115.416908850278));
#55568=CARTESIAN_POINT('Ctrl Pts',(19.9257175915022,0.525726425592309,115.45110998076));
#55569=CARTESIAN_POINT('Ctrl Pts',(19.6543672323539,0.929749490353506,115.480974606343));
#55570=CARTESIAN_POINT('Ctrl Pts',(19.4572181758747,1.12181982433915,115.498021674344));
#55571=CARTESIAN_POINT('Ctrl Pts',(19.2347288283088,1.28428049014307,115.515056878813));
#55572=CARTESIAN_POINT('Ctrl Pts',(19.013651074864,1.3833118822926,115.529946665983));
#55573=CARTESIAN_POINT('Ctrl Pts',(18.8140247733603,1.43321755407129,115.542697012047));
#55574=CARTESIAN_POINT('Ctrl Pts',(18.7128363519114,1.45115700732122,115.54906996985));
#55575=CARTESIAN_POINT('Ctrl Pts',(18.6276598573334,1.46017834311691,115.554378697797));
#55576=CARTESIAN_POINT('Ctrl Pts',(18.5592862695786,1.46371178414657,115.558624633332));
#55577=CARTESIAN_POINT('Ctrl Pts',(18.281804518493,1.46901920455917,115.575840541739));
#55578=CARTESIAN_POINT('Ctrl Pts',(17.7789208622668,1.34044114145594,115.607043467896));
#55579=CARTESIAN_POINT('Ctrl Pts',(17.3515825252313,0.943867467580674,115.642111302339));
#55580=CARTESIAN_POINT('Ctrl Pts',(17.161718430748,0.586643344943619,115.667111195049));
#55581=CARTESIAN_POINT('Ctrl Pts',(17.0971415218615,0.395305592897811,115.679598666197));
#55582=CARTESIAN_POINT('Ctrl Pts',(17.0654186859172,0.237367172497665,115.689581011609));
#55583=CARTESIAN_POINT('Ctrl Pts',(17.0275491270296,-0.0824119897447905,
115.709536206168));
#55584=CARTESIAN_POINT('Ctrl Pts',(17.1213154380764,-0.612393720202946,
115.741905478085));
#55585=CARTESIAN_POINT('Ctrl Pts',(17.5848400159856,-1.19334019842358,115.786583882468));
#55586=CARTESIAN_POINT('Ctrl Pts',(18.2105492300219,-1.45653032695076,115.827406065294));
#55587=CARTESIAN_POINT('Ctrl Pts',(18.8172754847527,-1.43320988743828,115.864408413174));
#55588=CARTESIAN_POINT('Ctrl Pts',(19.3166435273073,-1.21540635448681,115.897624944836));
#55589=CARTESIAN_POINT('Ctrl Pts',(19.7009419977361,-0.830844298663376,
115.930754148081));
#55590=CARTESIAN_POINT('Ctrl Pts',(19.8813782039901,-0.416853424760839,
115.958288014972));
#55591=CARTESIAN_POINT('Ctrl Pts',(19.9276431736338,-0.0638821576866821,
115.980269583929));
#55592=CARTESIAN_POINT('Ctrl Pts',(19.9127472486195,0.20223062639115,115.996733473868));
#55593=CARTESIAN_POINT('Ctrl Pts',(19.8593136020091,0.41757635134816,116.010433712158));
#55594=CARTESIAN_POINT('Ctrl Pts',(19.7931822001391,0.581413531785223,116.021382537624));
#55595=CARTESIAN_POINT('Ctrl Pts',(19.6717448900476,0.81682145173997,116.037794354297));
#55596=CARTESIAN_POINT('Ctrl Pts',(19.4086990851244,1.12231198394179,116.06236784433));
#55597=CARTESIAN_POINT('Ctrl Pts',(18.9347537982859,1.37264233511827,116.095038203222));
#55598=CARTESIAN_POINT('Ctrl Pts',(18.4036743708657,1.43232551015976,116.12761233323));
#55599=CARTESIAN_POINT('Ctrl Pts',(18.017732623987,1.32879363369123,116.15196992527));
#55600=CARTESIAN_POINT('Ctrl Pts',(17.7876887319677,1.20427083424148,116.168177533439));
#55601=CARTESIAN_POINT('Ctrl Pts',(17.6428048499461,1.1074956958902,116.178974506447));
#55602=CARTESIAN_POINT('Ctrl Pts',(17.4148844793436,0.903876845597534,116.197846985979));
#55603=CARTESIAN_POINT('Ctrl Pts',(17.2622074736554,0.661128460586399,116.215331339299));
#55604=CARTESIAN_POINT('Ctrl Pts',(17.188027229338,0.457688297602254,116.228757052948));
#55605=CARTESIAN_POINT('Ctrl Pts',(17.168559043819,0.395766595906644,116.23278314266));
#55606=CARTESIAN_POINT('Ctrl Pts',(17.1520743242299,0.332985467597782,116.236807679468));
#55607=CARTESIAN_POINT('Ctrl Pts',(17.138527639409,0.26955084397591,116.240830617286));
#55608=CARTESIAN_POINT('Ctrl Pts',(17.1279448550524,0.205565981972609,116.244851992867));
#55609=CARTESIAN_POINT('Ctrl Pts',(17.1179125927233,0.119727148367452,116.250211712015));
#55610=CARTESIAN_POINT('Ctrl Pts',(17.10663249924,-0.117752725314212,116.264942373433));
#55611=CARTESIAN_POINT('Ctrl Pts',(17.1801410722104,-0.505505163832453,
116.288998851246));
#55612=CARTESIAN_POINT('Ctrl Pts',(17.4593468605389,-0.949572639259783,
116.320971494261));
#55613=CARTESIAN_POINT('Ctrl Pts',(17.8801051002652,-1.2599094895317,116.352839941182));
#55614=CARTESIAN_POINT('Ctrl Pts',(18.3835262236398,-1.39462467271549,116.384603580865));
#55615=CARTESIAN_POINT('Ctrl Pts',(18.8995848502807,-1.33631990116552,116.416261382716));
#55616=CARTESIAN_POINT('Ctrl Pts',(19.3572158707464,-1.09429062186641,116.447812674778));
#55617=CARTESIAN_POINT('Ctrl Pts',(19.6187260169908,-0.790095912733049,
116.472268975216));
#55618=CARTESIAN_POINT('Ctrl Pts',(19.7439727930601,-0.537901365985853,
116.489697925247));
#55619=CARTESIAN_POINT('Ctrl Pts',(19.8181256978155,-0.325610218012137,
116.503624869793));
#55620=CARTESIAN_POINT('Ctrl Pts',(19.8776026319941,0.0653392500041546,
116.527955084156));
#55621=CARTESIAN_POINT('Ctrl Pts',(19.7492623583921,0.626762380276667,116.562591461326));
#55622=CARTESIAN_POINT('Ctrl Pts',(19.2935621397076,1.14241638930198,116.603960385172));
#55623=CARTESIAN_POINT('Ctrl Pts',(18.6500528451987,1.37621044955443,116.64513338571));
#55624=CARTESIAN_POINT('Ctrl Pts',(17.9761635526829,1.2742602408342,116.686109582385));
#55625=CARTESIAN_POINT('Ctrl Pts',(17.5146651224903,0.924134010931,116.720941344535));
#55626=CARTESIAN_POINT('Ctrl Pts',(17.2774362791059,0.520220428704234,116.749716614797));
#55627=CARTESIAN_POINT('Ctrl Pts',(17.1529354063379,0.0413427657848591,
116.780100883198));
#55628=CARTESIAN_POINT('Ctrl Pts',(17.2594728905108,-0.583805099635299,
116.817924242688));
#55629=CARTESIAN_POINT('Ctrl Pts',(17.7643920189576,-1.14787815539454,116.863060893889));
#55630=CARTESIAN_POINT('Ctrl Pts',(18.4878485549571,-1.355639848724,116.907946311528));
#55631=CARTESIAN_POINT('Ctrl Pts',(19.2068886828874,-1.1479083033055,116.952580891862));
#55632=CARTESIAN_POINT('Ctrl Pts',(19.7025859315818,-0.59243259627754,116.996965410243));
#55633=CARTESIAN_POINT('Ctrl Pts',(19.805116781009,0.0155843273252081,117.033744906381));
#55634=CARTESIAN_POINT('Ctrl Pts',(19.6849763257637,0.477310867630742,117.063044708738));
#55635=CARTESIAN_POINT('Ctrl Pts',(19.5041028285569,0.784752423535641,117.084957745122));
#55636=CARTESIAN_POINT('Ctrl Pts',(19.2452349298756,1.02876411530207,117.106809363928));
#55637=CARTESIAN_POINT('Ctrl Pts',(18.8252583549806,1.24665288186946,117.135863022342));
#55638=CARTESIAN_POINT('Ctrl Pts',(18.2198687746404,1.28039646177613,117.172027569721));
#55639=CARTESIAN_POINT('Ctrl Pts',(17.5866457772006,0.929702296368013,117.21518301736));
#55640=CARTESIAN_POINT('Ctrl Pts',(17.2390532742044,0.299598173471757,117.258099043471));
#55641=CARTESIAN_POINT('Ctrl Pts',(17.2797153311823,-0.415006662101263,
117.3007784115));
#55642=CARTESIAN_POINT('Ctrl Pts',(17.6920802994576,-0.995196786608285,
117.343224228662));
#55643=CARTESIAN_POINT('Ctrl Pts',(18.3463415258393,-1.26562861592044,117.385439850698));
#55644=CARTESIAN_POINT('Ctrl Pts',(19.0404591281284,-1.14715003431039,117.427428928389));
#55645=CARTESIAN_POINT('Ctrl Pts',(19.5623711434035,-0.680042513891968,
117.469195380227));
#55646=CARTESIAN_POINT('Ctrl Pts',(19.7547673292631,-0.0103754829418355,
117.510743394758));
#55647=CARTESIAN_POINT('Ctrl Pts',(19.5623929190238,0.655560976653802,117.552077418062));
#55648=CARTESIAN_POINT('Ctrl Pts',(19.0478297506675,1.11474704186936,117.593202163305));
#55649=CARTESIAN_POINT('Ctrl Pts',(18.3712156490552,1.22922475979801,117.63412259366));
#55650=CARTESIAN_POINT('Ctrl Pts',(17.7404829013797,0.967463930769031,117.674843912414));
#55651=CARTESIAN_POINT('Ctrl Pts',(17.3475629596244,0.412913264252416,117.715371566815));
#55652=CARTESIAN_POINT('Ctrl Pts',(17.310064375504,-0.262540500826519,117.755711245779));
#55653=CARTESIAN_POINT('Ctrl Pts',(17.636197520999,-0.85173985968551,117.795868851832));
#55654=CARTESIAN_POINT('Ctrl Pts',(18.2232061575254,-1.17571779828974,117.83585051381));
#55655=CARTESIAN_POINT('Ctrl Pts',(18.8898049415706,-1.13787460741934,117.875662566524));
#55656=CARTESIAN_POINT('Ctrl Pts',(19.4318065563587,-0.752832224962471,
117.915311577176));
#55657=CARTESIAN_POINT('Ctrl Pts',(19.6850206338496,-0.140764865189098,
117.954804243761));
#55658=CARTESIAN_POINT('Ctrl Pts',(19.5924643948714,0.401139914316672,117.987590349654));
#55659=CARTESIAN_POINT('Ctrl Pts',(19.3550318497187,0.754660044567889,118.01374802109));
#55660=CARTESIAN_POINT('Ctrl Pts',(19.0307937520553,1.02963893852138,118.039859642854));
#55661=CARTESIAN_POINT('Ctrl Pts',(18.50622690624,1.18069309462962,118.072414545105));
#55662=CARTESIAN_POINT('Ctrl Pts',(17.8787720595626,0.999543022593704,118.111353082998));
#55663=CARTESIAN_POINT('Ctrl Pts',(17.4452307248378,0.514012685374898,118.15017156465));
#55664=CARTESIAN_POINT('Ctrl Pts',(17.3367378446691,-0.125987357398448,
118.188877898695));
#55665=CARTESIAN_POINT('Ctrl Pts',(17.5846953995656,-0.723951514978575,
118.227479865732));
#55666=CARTESIAN_POINT('Ctrl Pts',(18.1114543571691,-1.0974563568826,118.265985524989));
#55667=CARTESIAN_POINT('Ctrl Pts',(18.7547058180995,-1.13336389519741,118.304402965018));
#55668=CARTESIAN_POINT('Ctrl Pts',(19.3173182988927,-0.822244782737743,
118.342740449353));
#55669=CARTESIAN_POINT('Ctrl Pts',(19.6275738333935,-0.26047787608183,118.381006236972));
#55670=CARTESIAN_POINT('Ctrl Pts',(19.5915390368011,0.379069408536245,118.419208846237));
#55671=CARTESIAN_POINT('Ctrl Pts',(19.2211927231264,0.900906054925335,118.45735657839));
#55672=CARTESIAN_POINT('Ctrl Pts',(18.7293427115169,1.10434931242854,118.489108025697));
#55673=CARTESIAN_POINT('Ctrl Pts',(18.3161133166046,1.09194722489886,118.514490132623));
#55674=CARTESIAN_POINT('Ctrl Pts',(18.0209984782359,0.998187264691806,118.533518695961));
#55675=CARTESIAN_POINT('Ctrl Pts',(17.7634928966558,0.82595466122776,118.552539656177));
#55676=CARTESIAN_POINT('Ctrl Pts',(17.563775870497,0.589521138450256,118.571554845456));
#55677=CARTESIAN_POINT('Ctrl Pts',(17.437363222974,0.306953574752756,118.590564605243));
#55678=CARTESIAN_POINT('Ctrl Pts',(17.3941193006543,0.000610802263239836,
118.609570707512));
#55679=CARTESIAN_POINT('Ctrl Pts',(17.4373534640508,-0.305796483992987,
118.628573614322));
#55680=CARTESIAN_POINT('Ctrl Pts',(17.5426862832814,-0.541016627132415,
118.644408242671));
#55681=CARTESIAN_POINT('Ctrl Pts',(17.6634779226648,-0.706381682981929,
118.657075049229));
#55682=CARTESIAN_POINT('Ctrl Pts',(17.806243697093,-0.852950163395337,118.66974258048));
#55683=CARTESIAN_POINT('Ctrl Pts',(18.106057194281,-1.05418422554283,118.691910013046));
#55684=CARTESIAN_POINT('Ctrl Pts',(18.6293906886623,-1.14333393643523,118.72358214913));
#55685=CARTESIAN_POINT('Ctrl Pts',(19.2187652101556,-0.899240835761239,
118.761603122514));
#55686=CARTESIAN_POINT('Ctrl Pts',(19.5261380986293,-0.46579781924761,118.793306539549));
#55687=CARTESIAN_POINT('Ctrl Pts',(19.5960047419514,-0.110829187609168,
118.815513403398));
#55688=CARTESIAN_POINT('Ctrl Pts',(19.5932711946567,0.0941203340922264,
118.828206979085));
#55689=CARTESIAN_POINT('Ctrl Pts',(19.561775887923,0.297086240693117,118.840904501667));
#55690=CARTESIAN_POINT('Ctrl Pts',(19.4694460545618,0.538278919044113,118.856782163855));
#55691=CARTESIAN_POINT('Ctrl Pts',(19.2211350815969,0.869636695096682,118.882201823917));
#55692=CARTESIAN_POINT('Ctrl Pts',(18.7546109285557,1.12774604749691,118.914006897353));
#55693=CARTESIAN_POINT('Ctrl Pts',(18.1144942029186,1.09193664690372,118.952230982635));
#55694=CARTESIAN_POINT('Ctrl Pts',(17.5906842728557,0.720468306166889,118.990521107805));
#55695=CARTESIAN_POINT('Ctrl Pts',(17.3855246482535,0.225277058832011,119.022491989366));
#55696=CARTESIAN_POINT('Ctrl Pts',(17.3980555839542,-0.191783272636398,
119.048109713078));
#55697=CARTESIAN_POINT('Ctrl Pts',(17.4768927747722,-0.44037660910954,119.06413951312));
#55698=CARTESIAN_POINT('Ctrl Pts',(17.5671568068215,-0.597988874584677,
119.075369732831));
#55699=CARTESIAN_POINT('Ctrl Pts',(17.627583349682,-0.682021820729704,119.08179007171));
#55700=CARTESIAN_POINT('Ctrl Pts',(17.6939097716351,-0.761655148296046,
119.088212380741));
#55701=CARTESIAN_POINT('Ctrl Pts',(17.7869510861829,-0.852129061282766,
119.096244363201));
#55702=CARTESIAN_POINT('Ctrl Pts',(17.9547144167929,-0.974787629722701,
119.109102616347));
#55703=CARTESIAN_POINT('Ctrl Pts',(18.1937763612775,-1.0818094293345,119.125191738617));
#55704=CARTESIAN_POINT('Ctrl Pts',(18.5054383431021,-1.1258363795764,119.144523919164));
#55705=CARTESIAN_POINT('Ctrl Pts',(18.8175251592586,-1.08180363622223,119.163883306933));
#55706=CARTESIAN_POINT('Ctrl Pts',(19.1056462869439,-0.952921422339809,
119.183270109433));
#55707=CARTESIAN_POINT('Ctrl Pts',(19.3471812503215,-0.748996843631803,
119.202685994533));
#55708=CARTESIAN_POINT('Ctrl Pts',(19.5230935936411,-0.485797243267148,
119.222131101893));
#55709=CARTESIAN_POINT('Ctrl Pts',(19.6194235398893,-0.183681159155142,
119.241607538908));
#55710=CARTESIAN_POINT('Ctrl Pts',(19.6283568615701,0.133769359585175,119.261114722082));
#55711=CARTESIAN_POINT('Ctrl Pts',(19.5621898852985,0.39051406225891,119.277398730761));
#55712=CARTESIAN_POINT('Ctrl Pts',(19.467979719698,0.579067452723987,119.290441977098));
#55713=CARTESIAN_POINT('Ctrl Pts',(19.3185921773537,0.796417004314266,119.306760645479));
#55714=CARTESIAN_POINT('Ctrl Pts',(19.0271066040016,1.03580841985484,119.329646794098));
#55715=CARTESIAN_POINT('Ctrl Pts',(18.5579560526582,1.16400930978687,119.359152271126));
#55716=CARTESIAN_POINT('Ctrl Pts',(18.0760367110303,1.08921289338611,119.388741208946));
#55717=CARTESIAN_POINT('Ctrl Pts',(17.6654854616247,0.823330943755025,119.418416546625));
#55718=CARTESIAN_POINT('Ctrl Pts',(17.3985369873615,0.411710794457526,119.448181135551));
#55719=CARTESIAN_POINT('Ctrl Pts',(17.3227666115826,-0.0745209629554153,
119.478037892946));
#55720=CARTESIAN_POINT('Ctrl Pts',(17.4525835817918,-0.550846602669221,
119.507989394093));
#55721=CARTESIAN_POINT('Ctrl Pts',(17.7143528381942,-0.869942542802271,
119.533030493605));
#55722=CARTESIAN_POINT('Ctrl Pts',(17.9889445791141,-1.04484589484823,119.553113195196));
#55723=CARTESIAN_POINT('Ctrl Pts',(18.2942955374926,-1.15931837182444,119.573229991214));
#55724=CARTESIAN_POINT('Ctrl Pts',(18.7094283500856,-1.17700658256433,119.598440038838));
#55725=CARTESIAN_POINT('Ctrl Pts',(19.1744277236937,-0.992164148776086,
119.628797431618));
#55726=CARTESIAN_POINT('Ctrl Pts',(19.5246105085742,-0.632300664711906,
119.659262467001));
#55727=CARTESIAN_POINT('Ctrl Pts',(19.6978971318757,-0.159064142767438,
119.689837552661));
#55728=CARTESIAN_POINT('Ctrl Pts',(19.6626494698746,0.345510270040854,119.720524932272));
#55729=CARTESIAN_POINT('Ctrl Pts',(19.4235062092649,0.793350318368254,119.751326824166));
#55730=CARTESIAN_POINT('Ctrl Pts',(19.0207724226401,1.10563928405634,119.782245336604));
#55731=CARTESIAN_POINT('Ctrl Pts',(18.5237348992026,1.22664815333434,119.813282525917));
#55732=CARTESIAN_POINT('Ctrl Pts',(18.0186212112409,1.13376405338814,119.844440332931));
#55733=CARTESIAN_POINT('Ctrl Pts',(17.6647078195633,0.890180692604903,119.870507283873));
#55734=CARTESIAN_POINT('Ctrl Pts',(17.459152794792,0.620520297905578,119.891422999201));
#55735=CARTESIAN_POINT('Ctrl Pts',(17.3135738426375,0.313569874486673,119.912380371528));
#55736=CARTESIAN_POINT('Ctrl Pts',(17.2588234924652,-0.116038476650668,
119.938655950413));
#55737=CARTESIAN_POINT('Ctrl Pts',(17.4100983478659,-0.615449946450397,
119.970314243228));
#55738=CARTESIAN_POINT('Ctrl Pts',(17.7535352748928,-1.01112010205256,120.002101741838));
#55739=CARTESIAN_POINT('Ctrl Pts',(18.2305891354705,-1.23292472309362,120.034019862503));
#55740=CARTESIAN_POINT('Ctrl Pts',(18.7588013590758,-1.24056168734763,120.066069997976));
#55741=CARTESIAN_POINT('Ctrl Pts',(19.2460849895487,-1.03092328241255,120.098253406646));
#55742=CARTESIAN_POINT('Ctrl Pts',(19.6067436569891,-0.638908623644245,
120.130571281471));
#55743=CARTESIAN_POINT('Ctrl Pts',(19.7765414423687,-0.131657613778088,
120.16302471018));
#55744=CARTESIAN_POINT('Ctrl Pts',(19.7241268936388,0.402946109902079,120.195614696143));
#55745=CARTESIAN_POINT('Ctrl Pts',(19.4568058001641,0.871483019948602,120.228342146454));
#55746=CARTESIAN_POINT('Ctrl Pts',(19.0195888769497,1.19131601339264,120.261207876936));
#55747=CARTESIAN_POINT('Ctrl Pts',(18.4876303130866,1.30515498304331,120.29421260826));
#55748=CARTESIAN_POINT('Ctrl Pts',(17.9533196433611,1.19131025373105,120.327356967205));
#55749=CARTESIAN_POINT('Ctrl Pts',(17.5102434085246,0.867796104159015,120.360641485681));
#55750=CARTESIAN_POINT('Ctrl Pts',(17.2367984070158,0.389513905763427,120.394066601003));
#55751=CARTESIAN_POINT('Ctrl Pts',(17.1823257731603,-0.161052944534343,
120.427632654705));
#55752=CARTESIAN_POINT('Ctrl Pts',(17.3582173349526,-0.688057393908344,
120.461339892745));
#55753=CARTESIAN_POINT('Ctrl Pts',(17.7355965521711,-1.09897149996487,120.495188465041));
#55754=CARTESIAN_POINT('Ctrl Pts',(18.2500378061209,-1.32083060054573,120.529178426105));
#55755=CARTESIAN_POINT('Ctrl Pts',(18.8125577781375,-1.31318644286814,120.563309734203));
#55756=CARTESIAN_POINT('Ctrl Pts',(19.3250052395169,-1.07547039577926,120.597582252196));
#55757=CARTESIAN_POINT('Ctrl Pts',(19.697188512651,-0.647426242261582,120.631995745907));
#55758=CARTESIAN_POINT('Ctrl Pts',(19.8627512839161,-0.102480320396054,
120.666549887297));
#55759=CARTESIAN_POINT('Ctrl Pts',(19.7910024142767,0.464853743541633,120.70124425028));
#55760=CARTESIAN_POINT('Ctrl Pts',(19.4925884258856,0.955366343499383,120.73607831879));
#55761=CARTESIAN_POINT('Ctrl Pts',(19.017965346801,1.28251422077536,120.771051472002));
#55762=CARTESIAN_POINT('Ctrl Pts',(18.448872236062,1.38768021419735,120.806163012952));
#55763=CARTESIAN_POINT('Ctrl Pts',(17.8842561866098,1.25070220238676,120.841412116456));
#55764=CARTESIAN_POINT('Ctrl Pts',(17.4230517533873,0.893660617828872,120.876797928954));
#55765=CARTESIAN_POINT('Ctrl Pts',(17.1468515279311,0.377437762693973,120.912319382562));
#55766=CARTESIAN_POINT('Ctrl Pts',(17.1054347892236,-0.208842011271403,
120.947975548869));
#55767=CARTESIAN_POINT('Ctrl Pts',(17.257242942961,-0.624353404722209,120.974817587713));
#55768=CARTESIAN_POINT('Ctrl Pts',(17.4241596596904,-0.860998050927015,
120.992753814121));
#55769=CARTESIAN_POINT('Ctrl Pts',(17.5513580669707,-1.00638554422223,121.004722033497));
#55770=CARTESIAN_POINT('Ctrl Pts',(17.8125062676019,-1.22417547142694,121.025695549015));
#55771=CARTESIAN_POINT('Ctrl Pts',(18.2724517094306,-1.40748417284606,121.055739282651));
#55772=CARTESIAN_POINT('Ctrl Pts',(18.8683616599553,-1.38258592298105,121.091921232995));
#55773=CARTESIAN_POINT('Ctrl Pts',(19.4039469371452,-1.11559596226272,121.128230999328));
#55774=CARTESIAN_POINT('Ctrl Pts',(19.7851220860264,-0.651485254357956,
121.164667024263));
#55775=CARTESIAN_POINT('Ctrl Pts',(19.9440082322412,-0.0702040346042679,
121.201227575976));
#55776=CARTESIAN_POINT('Ctrl Pts',(19.8513116568888,0.527285905129969,121.237910885291));
#55777=CARTESIAN_POINT('Ctrl Pts',(19.5215667915217,1.03646753264763,121.274715074731));
#55778=CARTESIAN_POINT('Ctrl Pts',(19.0109647654682,1.3676240556558,121.31163819733));
#55779=CARTESIAN_POINT('Ctrl Pts',(18.4077307987017,1.46163653233743,121.348678218649));
#55780=CARTESIAN_POINT('Ctrl Pts',(17.8168866182968,1.30056114436624,121.385833028301));
#55781=CARTESIAN_POINT('Ctrl Pts',(17.3419316367841,0.911026491110346,121.42310043786));
#55782=CARTESIAN_POINT('Ctrl Pts',(17.0666957019877,0.359844238279606,121.460478181363));
#55783=CARTESIAN_POINT('Ctrl Pts',(17.0405213308045,-0.257462790858785,
121.49796392011));
#55784=CARTESIAN_POINT('Ctrl Pts',(17.2694126324673,-0.833236802289572,
121.535555236205));
#55785=CARTESIAN_POINT('Ctrl Pts',(17.7147338114203,-1.26648509350842,121.57324965169));
#55786=CARTESIAN_POINT('Ctrl Pts',(18.2997310041706,-1.48062436312049,121.611044598073));
#55787=CARTESIAN_POINT('Ctrl Pts',(18.9227806176326,-1.43702806539659,121.648937478815));
#55788=CARTESIAN_POINT('Ctrl Pts',(19.475064541157,-1.14201388349045,121.686925554159));
#55789=CARTESIAN_POINT('Ctrl Pts',(19.8596141628965,-0.645935586892937,
121.725006162078));
#55790=CARTESIAN_POINT('Ctrl Pts',(20.008346706193,-0.0346372378620192,
121.763176310523));
#55791=CARTESIAN_POINT('Ctrl Pts',(19.8941556704044,0.585521991047194,121.80143337875));
#55792=CARTESIAN_POINT('Ctrl Pts',(19.5358462733169,1.10607313572164,121.839774198206));
#55793=CARTESIAN_POINT('Ctrl Pts',(18.995024727083,1.43556935990143,121.878195884757));
#55794=CARTESIAN_POINT('Ctrl Pts',(18.3655210390793,1.51558521854799,121.916695382839));
#55795=CARTESIAN_POINT('Ctrl Pts',(17.7570606450874,1.33114453962665,121.95526955489));
#55796=CARTESIAN_POINT('Ctrl Pts',(17.2761160603867,0.913489361496773,121.993915283113));
#55797=CARTESIAN_POINT('Ctrl Pts',(17.0072368483796,0.334798105910418,122.032629365255));
#55798=CARTESIAN_POINT('Ctrl Pts',(16.9981624241316,-0.304316767733318,
122.071408517403));
#55799=CARTESIAN_POINT('Ctrl Pts',(17.251330532035,-0.892329965491541,122.11024951087));
#55800=CARTESIAN_POINT('Ctrl Pts',(17.7233021624858,-1.3263014609352,122.149148947241));
#55801=CARTESIAN_POINT('Ctrl Pts',(18.3322262968092,-1.5299313411392,122.188103494914));
#55802=CARTESIAN_POINT('Ctrl Pts',(18.9720612013498,-1.46700073882079,122.227109746095));
#55803=CARTESIAN_POINT('Ctrl Pts',(19.5310749635394,-1.14782155829681,122.266164210345));
#55804=CARTESIAN_POINT('Ctrl Pts',(19.9113979815986,-0.627556137759355,
122.305263484811));
#55805=CARTESIAN_POINT('Ctrl Pts',(20.0461854224048,0.00334322599405469,
122.344403969626));
#55806=CARTESIAN_POINT('Ctrl Pts',(19.9113972671777,0.63487192224289,122.383582231813));
#55807=CARTESIAN_POINT('Ctrl Pts',(19.5300757175112,1.15672922617075,122.422794562142));
#55808=CARTESIAN_POINT('Ctrl Pts',(18.9684369249769,1.47756196833367,122.462037597625));
#55809=CARTESIAN_POINT('Ctrl Pts',(18.3242818697673,1.54104364912502,122.501307500968));
#55810=CARTESIAN_POINT('Ctrl Pts',(17.7100244133753,1.33578019286523,122.540600797604));
#55811=CARTESIAN_POINT('Ctrl Pts',(17.2329398048057,0.897263318486983,122.579913783485));
#55812=CARTESIAN_POINT('Ctrl Pts',(16.9764784072532,0.301964176637347,122.619242811121));
#55813=CARTESIAN_POINT('Ctrl Pts',(16.9845337828457,-0.274473648200087,
122.654212995416));
#55814=CARTESIAN_POINT('Ctrl Pts',(17.1627555053455,-0.739648570522611,
122.684817494633));
#55815=CARTESIAN_POINT('Ctrl Pts',(17.5044140404774,-1.19548846578833,122.719797873699));
#55816=CARTESIAN_POINT('Ctrl Pts',(18.1459455530736,-1.55032796429415,122.763527455907));
#55817=CARTESIAN_POINT('Ctrl Pts',(19.0247080539113,-1.50093222138397,122.81600109576));
#55818=CARTESIAN_POINT('Ctrl Pts',(19.7421346852786,-0.991773946961065,
122.868463997585));
#55819=CARTESIAN_POINT('Ctrl Pts',(20.078678890067,-0.179297852006348,122.920907533627));
#55820=CARTESIAN_POINT('Ctrl Pts',(19.931361285469,0.687441108918969,122.97332295464));
#55821=CARTESIAN_POINT('Ctrl Pts',(19.4435177864377,1.2328776932785,123.016971870743));
#55822=CARTESIAN_POINT('Ctrl Pts',(18.9243150922261,1.46395147514551,123.051868326394));
#55823=CARTESIAN_POINT('Ctrl Pts',(18.5183951569639,1.52178329193078,123.077059337171));
#55824=CARTESIAN_POINT('Ctrl Pts',(18.1281145921538,1.47237094917012,123.101269725337));
#55825=CARTESIAN_POINT('Ctrl Pts',(17.6593637564239,1.28921713675561,123.132243778228));
#55826=CARTESIAN_POINT('Ctrl Pts',(17.1876918207849,0.851581019041659,123.170931091307));
#55827=CARTESIAN_POINT('Ctrl Pts',(16.9832215152354,0.242357233593553,123.209572770744));
#55828=CARTESIAN_POINT('Ctrl Pts',(17.0091058149915,-0.258767597083051,
123.240456182328));
#55829=CARTESIAN_POINT('Ctrl Pts',(17.1560922813407,-0.738084296272097,
123.271318228827));
#55830=CARTESIAN_POINT('Ctrl Pts',(17.5557244048119,-1.23929750545205,123.309854723166));
#55831=CARTESIAN_POINT('Ctrl Pts',(18.2044422297094,-1.51227958537405,123.352178753354));
#55832=CARTESIAN_POINT('Ctrl Pts',(18.8343869808506,-1.48815787538939,123.390598660515));
#55833=CARTESIAN_POINT('Ctrl Pts',(19.353588737119,-1.2617754559261,123.425130511472));
#55834=CARTESIAN_POINT('Ctrl Pts',(19.7535878185842,-0.861555544152392,
123.459613986599));
#55835=CARTESIAN_POINT('Ctrl Pts',(19.9794032819064,-0.343829749696201,
123.494046857608));
#55836=CARTESIAN_POINT('Ctrl Pts',(20.000423736225,0.219869657394578,123.528426618707));
#55837=CARTESIAN_POINT('Ctrl Pts',(19.8143309546131,0.751313711751814,123.562751365816));
#55838=CARTESIAN_POINT('Ctrl Pts',(19.5087207298247,1.10644312189301,123.591307129293));
#55839=CARTESIAN_POINT('Ctrl Pts',(19.1994192267151,1.30841669722232,123.614122206283));
#55840=CARTESIAN_POINT('Ctrl Pts',(18.8018880211566,1.47383184469139,123.640715972828));
#55841=CARTESIAN_POINT('Ctrl Pts',(18.203271795634,1.50358610427353,123.676747659749));
#55842=CARTESIAN_POINT('Ctrl Pts',(17.636687751151,1.23032070130387,123.714579983589));
#55843=CARTESIAN_POINT('Ctrl Pts',(17.30320303094,0.870020035335568,123.744785773105));
#55844=CARTESIAN_POINT('Ctrl Pts',(17.1276403635631,0.547396546141828,123.767409714068));
#55845=CARTESIAN_POINT('Ctrl Pts',(17.0061453562421,0.0729490378705759,
123.79753311268));
#55846=CARTESIAN_POINT('Ctrl Pts',(17.076311597054,-0.484727721015513,123.831350608742));
#55847=CARTESIAN_POINT('Ctrl Pts',(17.4041389802875,-1.00524236044422,123.868829379186));
#55848=CARTESIAN_POINT('Ctrl Pts',(17.8666645324534,-1.34678546980139,123.903886582043));
#55849=CARTESIAN_POINT('Ctrl Pts',(18.4492984685224,-1.48828068205571,123.940256330297));
#55850=CARTESIAN_POINT('Ctrl Pts',(19.0598066985192,-1.37550604828877,123.977923741201));
#55851=CARTESIAN_POINT('Ctrl Pts',(19.5271103794071,-1.05345495711953,124.012357050828));
#55852=CARTESIAN_POINT('Ctrl Pts',(19.7569163431838,-0.716570316510549,
124.037337521724));
#55853=CARTESIAN_POINT('Ctrl Pts',(19.8842721919957,-0.406132863032926,
124.058124610392));
#55854=CARTESIAN_POINT('Ctrl Pts',(19.9468983857731,-0.0912051795872804,
124.077845882252));
#55855=CARTESIAN_POINT('Ctrl Pts',(19.9128060685492,0.312131110791157,124.102708347526));
#55856=CARTESIAN_POINT('Ctrl Pts',(19.7686968044805,0.689516156019462,124.12752086565));
#55857=CARTESIAN_POINT('Ctrl Pts',(19.5262222384832,1.01161051681084,124.152283309869));
#55858=CARTESIAN_POINT('Ctrl Pts',(19.2047436092611,1.25346719763061,124.176994654029));
#55859=CARTESIAN_POINT('Ctrl Pts',(18.8608700518071,1.38470264636897,124.199599471414));
#55860=CARTESIAN_POINT('Ctrl Pts',(18.5307429560582,1.42405810218505,124.220111266288));
#55861=CARTESIAN_POINT('Ctrl Pts',(18.1339511090329,1.38805442878169,124.244685991001));
#55862=CARTESIAN_POINT('Ctrl Pts',(17.6701428523837,1.1882073001127,124.275329590867));
#55863=CARTESIAN_POINT('Ctrl Pts',(17.2614772001437,0.743236175006286,124.311980647433));
#55864=CARTESIAN_POINT('Ctrl Pts',(17.0708207279897,0.172186327797883,124.348508410227));
#55865=CARTESIAN_POINT('Ctrl Pts',(17.1298493738262,-0.424934717672883,
124.384911209635));
#55866=CARTESIAN_POINT('Ctrl Pts',(17.4265801116394,-0.944023464590011,
124.421187316989));
#55867=CARTESIAN_POINT('Ctrl Pts',(17.9077483098367,-1.29540685305693,124.457335165658));
#55868=CARTESIAN_POINT('Ctrl Pts',(18.4883777457567,-1.41915590235369,124.493353235692));
#55869=CARTESIAN_POINT('Ctrl Pts',(19.0667970754498,-1.29541084050984,124.529240117323));
#55870=CARTESIAN_POINT('Ctrl Pts',(19.5424601631271,-0.947491030561093,
124.564994478041));
#55871=CARTESIAN_POINT('Ctrl Pts',(19.8334367279826,-0.437548507507534,
124.600615080923));
#55872=CARTESIAN_POINT('Ctrl Pts',(19.890532162967,0.144554159051283,124.636100776618));
#55873=CARTESIAN_POINT('Ctrl Pts',(19.7056002759952,0.697081689981892,124.671450509215));
#55874=CARTESIAN_POINT('Ctrl Pts',(19.31264694973,1.1242227099732,124.706663314447));
#55875=CARTESIAN_POINT('Ctrl Pts',(18.7815879028084,1.35271038509035,124.741738321289));
#55876=CARTESIAN_POINT('Ctrl Pts',(18.2058055231885,1.34439292496962,124.776674751525));
#55877=CARTESIAN_POINT('Ctrl Pts',(17.6857205110023,1.10259169434594,124.81147192126));
#55878=CARTESIAN_POINT('Ctrl Pts',(17.3112703623074,0.671193369840806,124.84612924114));
#55879=CARTESIAN_POINT('Ctrl Pts',(17.1463529681068,0.126691569128493,124.880646216948));
#55880=CARTESIAN_POINT('Ctrl Pts',(17.2179263446672,-0.435378650074446,
124.915022449439));
#55881=CARTESIAN_POINT('Ctrl Pts',(17.51162287668,-0.917207316201509,124.949257634716));
#55882=CARTESIAN_POINT('Ctrl Pts',(17.9745869037968,-1.23573305878125,124.983351564605));
#55883=CARTESIAN_POINT('Ctrl Pts',(18.5249812919712,-1.33696044526901,125.017304127033));
#55884=CARTESIAN_POINT('Ctrl Pts',(19.0664533911177,-1.20510407231254,125.05111530585));
#55885=CARTESIAN_POINT('Ctrl Pts',(19.5050030607281,-0.865013250071704,
125.08478518061));
#55886=CARTESIAN_POINT('Ctrl Pts',(19.7652995061654,-0.377512664504211,
125.118313926678));
#55887=CARTESIAN_POINT('Ctrl Pts',(19.8036148445623,0.171470264339861,125.151701815308));
#55888=CARTESIAN_POINT('Ctrl Pts',(19.6151555861472,0.68604789282707,125.184949213517));
#55889=CARTESIAN_POINT('Ctrl Pts',(19.2345664267479,1.0771164944424,125.218056583602));
#55890=CARTESIAN_POINT('Ctrl Pts',(18.7295776788037,1.2777789898754,125.251024482545));
#55891=CARTESIAN_POINT('Ctrl Pts',(18.1889590277654,1.25477807637706,125.283853562006));
#55892=CARTESIAN_POINT('Ctrl Pts',(17.7069217162722,1.01398801261303,125.316544568073));
#55893=CARTESIAN_POINT('Ctrl Pts',(17.3667091947938,0.599062987557933,125.349098340655));
#55894=CARTESIAN_POINT('Ctrl Pts',(17.2262326256709,0.0835362323822979,
125.381515812706));
#55895=CARTESIAN_POINT('Ctrl Pts',(17.3082274780863,-0.442201849037498,
125.413798009192));
#55896=CARTESIAN_POINT('Ctrl Pts',(17.5966013589314,-0.886741847862278,
125.445946047028));
#55897=CARTESIAN_POINT('Ctrl Pts',(18.0395538508959,-1.17353593875436,125.477961134467));
#55898=CARTESIAN_POINT('Ctrl Pts',(18.5588683493257,-1.25406427559042,125.509844570104));
#55899=CARTESIAN_POINT('Ctrl Pts',(19.0637106321298,-1.11602592841314,125.541597741769));
#55900=CARTESIAN_POINT('Ctrl Pts',(19.4665019523936,-0.785175599263413,
125.573222125044));
#55901=CARTESIAN_POINT('Ctrl Pts',(19.6980954335397,-0.320540839004115,
125.604719283131));
#55902=CARTESIAN_POINT('Ctrl Pts',(19.7196286151713,0.196094904948042,125.636090865987));
#55903=CARTESIAN_POINT('Ctrl Pts',(19.5290243381413,0.674571056739599,125.667338608869));
#55904=CARTESIAN_POINT('Ctrl Pts',(19.161057269751,1.03206511272243,125.698464330996));
#55905=CARTESIAN_POINT('Ctrl Pts',(18.6810272845914,1.20740872383971,125.729469933572));
#55906=CARTESIAN_POINT('Ctrl Pts',(18.1731880784998,1.17153389999086,125.760357399525));
#55907=CARTESIAN_POINT('Ctrl Pts',(17.7259793640479,0.932269103252213,125.791128792605));
#55908=CARTESIAN_POINT('Ctrl Pts',(17.4166481460682,0.532699142812196,125.821786255271));
#55909=CARTESIAN_POINT('Ctrl Pts',(17.2979289089794,0.0434238889981436,
125.852332007358));
#55910=CARTESIAN_POINT('Ctrl Pts',(17.3890747127762,-0.449895700330302,
125.882768343437));
#55911=CARTESIAN_POINT('Ctrl Pts',(17.6727604197615,-0.861510746724262,
125.913097632608));
#55912=CARTESIAN_POINT('Ctrl Pts',(18.0983508923542,-1.12046324618725,125.943322317335));
#55913=CARTESIAN_POINT('Ctrl Pts',(18.5909205460674,-1.18279337377893,125.973444911086));
#55914=CARTESIAN_POINT('Ctrl Pts',(19.064420089077,-1.03898045127023,126.003467996632));
#55915=CARTESIAN_POINT('Ctrl Pts',(19.4366807791309,-0.715362751697529,
126.033394223096));
#55916=CARTESIAN_POINT('Ctrl Pts',(19.6436450174629,-0.269331625013446,
126.063226305569));
#55917=CARTESIAN_POINT('Ctrl Pts',(19.6503634796231,0.220825607772631,126.092967023883));
#55918=CARTESIAN_POINT('Ctrl Pts',(19.4568759059551,0.669639021035746,126.122619219901));
#55919=CARTESIAN_POINT('Ctrl Pts',(19.0979908142443,0.999328230901447,126.152185795611));
#55920=CARTESIAN_POINT('Ctrl Pts',(18.6370406771027,1.15325141249116,126.181669709829));
#55921=CARTESIAN_POINT('Ctrl Pts',(18.1547300638473,1.10561141161178,126.211073977686));
#55922=CARTESIAN_POINT('Ctrl Pts',(17.7350366382869,0.865760124565423,126.240401669216));
#55923=CARTESIAN_POINT('Ctrl Pts',(17.4506232868768,0.476387237297481,126.269655906651));
#55924=CARTESIAN_POINT('Ctrl Pts',(17.3502891400616,0.00594117354873083,
126.298839861967));
#55925=CARTESIAN_POINT('Ctrl Pts',(17.4506205281827,-0.463375181533064,
126.327956753676));
#55926=CARTESIAN_POINT('Ctrl Pts',(17.7332657943092,-0.849933821163535,
126.3570098459));
#55927=CARTESIAN_POINT('Ctrl Pts',(18.1482785980622,-1.08684381320572,126.386002446982));
#55928=CARTESIAN_POINT('Ctrl Pts',(18.6229220125094,-1.13349526950984,126.414937906657));
#55929=CARTESIAN_POINT('Ctrl Pts',(19.0743847326823,-0.982499015596272,
126.4438196133));
#55930=CARTESIAN_POINT('Ctrl Pts',(19.424192069326,-0.660840549056361,126.472650990649));
#55931=CARTESIAN_POINT('Ctrl Pts',(19.6118106557014,-0.225071250741804,
126.501435496495));
#55932=CARTESIAN_POINT('Ctrl Pts',(19.6050944907734,0.248608474895961,126.530176621242));
#55933=CARTESIAN_POINT('Ctrl Pts',(19.4057746373271,0.677638998879331,126.558877885567));
#55934=CARTESIAN_POINT('Ctrl Pts',(19.0490596952358,0.987451960857726,126.587542836246));
#55935=CARTESIAN_POINT('Ctrl Pts',(18.597433005056,1.12439519713685,126.616175045175));
#55936=CARTESIAN_POINT('Ctrl Pts',(18.1297382366635,1.06499687702138,126.644778103328));
#55937=CARTESIAN_POINT('Ctrl Pts',(17.7274508894903,0.819976494804396,126.673355627513));
#55938=CARTESIAN_POINT('Ctrl Pts',(17.46052738614,0.432314452937021,126.701911243189));
#55939=CARTESIAN_POINT('Ctrl Pts',(17.3752688798186,-0.0302622593028861,
126.730448607546));
#55940=CARTESIAN_POINT('Ctrl Pts',(17.4863236298534,-0.4870874654627,126.758971357521));
#55941=CARTESIAN_POINT('Ctrl Pts',(17.7741583266334,-0.858567970464191,
126.787483198642));
#55942=CARTESIAN_POINT('Ctrl Pts',(18.1885215296499,-1.08004071358368,126.815987733931));
#55943=CARTESIAN_POINT('Ctrl Pts',(18.6571227528184,-1.11294273911574,126.84448878));
#55944=CARTESIAN_POINT('Ctrl Pts',(19.0983396321036,-0.951607216982945,
126.87298976346));
#55945=CARTESIAN_POINT('Ctrl Pts',(19.3790073574672,-0.678636495961043,
126.896744018428));
#55946=CARTESIAN_POINT('Ctrl Pts',(19.5220836903997,-0.405756943585032,
126.915750760586));
#55947=CARTESIAN_POINT('Ctrl Pts',(19.6056047918582,-0.109116596200933,
126.934761112833));
#55948=CARTESIAN_POINT('Ctrl Pts',(19.5891990596196,0.282305480414591,126.958530471191));
#55949=CARTESIAN_POINT('Ctrl Pts',(19.3791775936598,0.703224821732214,126.987068898185));
#55950=CARTESIAN_POINT('Ctrl Pts',(19.0153693298559,1.00184926778107,127.015625598023));
#55951=CARTESIAN_POINT('Ctrl Pts',(18.5609439856181,1.12593517559301,127.044204512567));
#55952=CARTESIAN_POINT('Ctrl Pts',(18.0950635602875,1.05353232660813,127.072809113128));
#55953=CARTESIAN_POINT('Ctrl Pts',(17.6989714968607,0.796900190380831,127.101443096007));
#55954=CARTESIAN_POINT('Ctrl Pts',(17.4419485246998,0.400416874555999,127.13011000932));
#55955=CARTESIAN_POINT('Ctrl Pts',(17.3691828511564,-0.0670598713129301,
127.158813447632));
#55956=CARTESIAN_POINT('Ctrl Pts',(17.4938709051282,-0.524124201025331,
127.18755694342));
#55957=CARTESIAN_POINT('Ctrl Pts',(17.7948197733865,-0.890955803526526,
127.216344020369));
#55958=CARTESIAN_POINT('Ctrl Pts',(18.2200428622329,-1.10322448511446,127.245178163347));
#55959=CARTESIAN_POINT('Ctrl Pts',(18.6957109311462,-1.12334093168554,127.274062831572));
#55960=CARTESIAN_POINT('Ctrl Pts',(19.1389377379455,-0.947095772661866,
127.303001446521));
#55961=CARTESIAN_POINT('Ctrl Pts',(19.4721844503801,-0.604515201648737,
127.331997395638));
#55962=CARTESIAN_POINT('Ctrl Pts',(19.6367900836946,-0.154763370218899,
127.361054019705));
#55963=CARTESIAN_POINT('Ctrl Pts',(19.6032731046921,0.324047256434558,127.390174640306));
#55964=CARTESIAN_POINT('Ctrl Pts',(19.3765936226467,0.748387713713813,127.419362477709));
#55965=CARTESIAN_POINT('Ctrl Pts',(18.99545138893,1.04384901099861,127.448620841323));
#55966=CARTESIAN_POINT('Ctrl Pts',(18.5256921328986,1.15815663876935,127.477952723227));
#55967=CARTESIAN_POINT('Ctrl Pts',(18.0489718439953,1.07040199940171,127.507361577771));
#55968=CARTESIAN_POINT('Ctrl Pts',(17.6485849520916,0.794842800013771,127.536849772547));
#55969=CARTESIAN_POINT('Ctrl Pts',(17.3949567046523,0.378620118062738,127.566421855019));
#55970=CARTESIAN_POINT('Ctrl Pts',(17.3332559961865,-0.106295560388526,
127.596077582544));
#55971=CARTESIAN_POINT('Ctrl Pts',(17.4754687696325,-0.575519789631179,
127.6258257653));
#55972=CARTESIAN_POINT('Ctrl Pts',(17.7977855400058,-0.9468941024104,127.655659616253));
#55973=CARTESIAN_POINT('Ctrl Pts',(18.2453408438712,-1.15482413737233,127.685596661067));
#55974=CARTESIAN_POINT('Ctrl Pts',(18.7399637910724,-1.16200183707374,127.715615510269));
#55975=CARTESIAN_POINT('Ctrl Pts',(19.1964401094813,-0.965517772876336,
127.745762596965));
#55976=CARTESIAN_POINT('Ctrl Pts',(19.5336962630831,-0.599252394510159,
127.775963740483));
#55977=CARTESIAN_POINT('Ctrl Pts',(19.6915929912239,-0.124428463739348,
127.806325164134));
#55978=CARTESIAN_POINT('Ctrl Pts',(19.6524076589129,0.291505836798268,127.831711772845));
#55979=CARTESIAN_POINT('Ctrl Pts',(19.5191279816085,0.592593656833114,127.851988567495));
#55980=CARTESIAN_POINT('Ctrl Pts',(19.3724951349617,0.794645357387739,127.867306889191));
#55981=CARTESIAN_POINT('Ctrl Pts',(19.1874613302448,0.962053453799274,127.882681906434));
#55982=CARTESIAN_POINT('Ctrl Pts',(18.9757369246924,1.08607203149486,127.89802598822));
#55983=CARTESIAN_POINT('Ctrl Pts',(18.7443752728392,1.16211632557479,127.913317040423));
#55984=CARTESIAN_POINT('Ctrl Pts',(18.5765564222551,1.18031848976882,127.923609419278));
#55985=CARTESIAN_POINT('Ctrl Pts',(18.4888644293293,1.18105655666575,127.928800510495));
#55986=CARTESIAN_POINT('Ctrl Pts',(18.488182152249,1.29990053410893,112.700349483895));
#55987=CARTESIAN_POINT('Ctrl Pts',(18.3444976430382,1.29869120157713,112.70885515658));
#55988=CARTESIAN_POINT('Ctrl Pts',(18.1626414086569,1.26954424100949,112.72020028386));
#55989=CARTESIAN_POINT('Ctrl Pts',(17.9105741471188,1.1715572059241,112.7372275449));
#55990=CARTESIAN_POINT('Ctrl Pts',(17.7147016928909,1.05680544825268,112.75142581384));
#55991=CARTESIAN_POINT('Ctrl Pts',(17.5092914781924,0.870936460786282,112.768496063499));
#55992=CARTESIAN_POINT('Ctrl Pts',(17.3452643787265,0.645338607702756,112.785608543142));
#55993=CARTESIAN_POINT('Ctrl Pts',(17.1949694671818,0.305633664533222,112.808486356608));
#55994=CARTESIAN_POINT('Ctrl Pts',(17.1504041586296,-0.163958059400556,
112.8371493128));
#55995=CARTESIAN_POINT('Ctrl Pts',(17.3295581344551,-0.704127606930189,
112.871679546659));
#55996=CARTESIAN_POINT('Ctrl Pts',(17.7163063911852,-1.12497913550319,112.906352649458));
#55997=CARTESIAN_POINT('Ctrl Pts',(18.2431925961433,-1.35205912276461,112.941152109412));
#55998=CARTESIAN_POINT('Ctrl Pts',(18.8187741112765,-1.34427642838518,112.976089285723));
#55999=CARTESIAN_POINT('Ctrl Pts',(19.3432395618757,-1.10098396627254,113.011156346434));
#56000=CARTESIAN_POINT('Ctrl Pts',(19.7238494382154,-0.663159822701633,
113.046357078694));
#56001=CARTESIAN_POINT('Ctrl Pts',(19.8931314314799,-0.105956319615994,
113.08168722595));
#56002=CARTESIAN_POINT('Ctrl Pts',(19.8197719071333,0.473908286429459,113.117148366555));
#56003=CARTESIAN_POINT('Ctrl Pts',(19.514861434432,0.975046989864885,113.152737815001));
#56004=CARTESIAN_POINT('Ctrl Pts',(19.0301258646803,1.30913564752012,113.188455340763));
#56005=CARTESIAN_POINT('Ctrl Pts',(18.4491549165285,1.416472562517,113.224299311997));
#56006=CARTESIAN_POINT('Ctrl Pts',(17.8730091730699,1.27666467315962,113.260268611474));
#56007=CARTESIAN_POINT('Ctrl Pts',(17.4026034483492,0.912474225359778,113.296361769111));
#56008=CARTESIAN_POINT('Ctrl Pts',(17.1210280345443,0.386131812194797,113.332577359437));
#56009=CARTESIAN_POINT('Ctrl Pts',(17.0788544181136,-0.211299879373549,
113.368913814958));
#56010=CARTESIAN_POINT('Ctrl Pts',(17.2850565553758,-0.775695991436841,
113.405369493798));
#56011=CARTESIAN_POINT('Ctrl Pts',(17.705146965038,-1.20803167965084,113.441942712263));
#56012=CARTESIAN_POINT('Ctrl Pts',(18.2669652505624,-1.43177932086286,113.478631613973));
#56013=CARTESIAN_POINT('Ctrl Pts',(18.8730309513044,-1.40645905314605,113.51543444437));
#56014=CARTESIAN_POINT('Ctrl Pts',(19.4175618056869,-1.13497091574588,113.55234907248));
#56015=CARTESIAN_POINT('Ctrl Pts',(19.8048480383929,-0.663350581086933,
113.589373656825));
#56016=CARTESIAN_POINT('Ctrl Pts',(19.966197057422,-0.0729778537808475,
113.626505971993));
#56017=CARTESIAN_POINT('Ctrl Pts',(19.8720657245217,0.533549954628291,113.663743893195));
#56018=CARTESIAN_POINT('Ctrl Pts',(19.5374817640394,1.0501311842453,113.701085198819));
#56019=CARTESIAN_POINT('Ctrl Pts',(19.0196808505253,1.38594482959087,113.738527490934));
#56020=CARTESIAN_POINT('Ctrl Pts',(18.5101754020758,1.46526119175664,113.769811704289));
#56021=CARTESIAN_POINT('Ctrl Pts',(18.1090240872925,1.39960741569811,113.794887075397));
#56022=CARTESIAN_POINT('Ctrl Pts',(17.729655069815,1.25220225914757,113.819994103033));
#56023=CARTESIAN_POINT('Ctrl Pts',(17.3289300722954,0.923586877948104,113.851436567131));
#56024=CARTESIAN_POINT('Ctrl Pts',(17.0504721252432,0.365805609893722,113.889258509496));
#56025=CARTESIAN_POINT('Ctrl Pts',(17.0240290762783,-0.258477757917008,
113.927168961164));
#56026=CARTESIAN_POINT('Ctrl Pts',(17.2554238425403,-0.840447617959809,
113.965165177094));
#56027=CARTESIAN_POINT('Ctrl Pts',(17.7053131011304,-1.27808626113464,114.003244380208));
#56028=CARTESIAN_POINT('Ctrl Pts',(18.2959641544648,-1.49425702735341,114.041403784502));
#56029=CARTESIAN_POINT('Ctrl Pts',(18.9246622805112,-1.4502272181577,114.079640512388));
#56030=CARTESIAN_POINT('Ctrl Pts',(19.4816239236303,-1.15267110135651,114.117951609114));
#56031=CARTESIAN_POINT('Ctrl Pts',(19.8691907107327,-0.652639427392253,
114.156334167846));
#56032=CARTESIAN_POINT('Ctrl Pts',(20.0189810591327,-0.03683256961316,114.194785080069));
#56033=CARTESIAN_POINT('Ctrl Pts',(19.9039833865991,0.587522999416328,114.2333013558));
#56034=CARTESIAN_POINT('Ctrl Pts',(19.5434230734537,1.11127572106957,114.271879839515));
#56035=CARTESIAN_POINT('Ctrl Pts',(18.9995399107886,1.44259279852258,114.310517384521));
#56036=CARTESIAN_POINT('Ctrl Pts',(18.3668596633944,1.52297273199859,114.349210799966));
#56037=CARTESIAN_POINT('Ctrl Pts',(17.7556977562459,1.33767203016567,114.387956849117));
#56038=CARTESIAN_POINT('Ctrl Pts',(17.272914349715,0.918370107647551,114.426752263094));
#56039=CARTESIAN_POINT('Ctrl Pts',(17.0031861863323,0.337753138207008,114.46559374694));
#56040=CARTESIAN_POINT('Ctrl Pts',(16.9941242219495,-0.303088855509916,
114.504477951706));
#56041=CARTESIAN_POINT('Ctrl Pts',(17.2478715429229,-0.892350566926149,
114.543401543985));
#56042=CARTESIAN_POINT('Ctrl Pts',(17.720592505509,-1.32694200600498,114.582361077963));
#56043=CARTESIAN_POINT('Ctrl Pts',(18.3301332049521,-1.53077558802408,114.621353247865));
#56044=CARTESIAN_POINT('Ctrl Pts',(18.8635057740616,-1.47820468577621,114.653870882415));
#56045=CARTESIAN_POINT('Ctrl Pts',(19.2496685905278,-1.30821665552171,114.679897931973));
#56046=CARTESIAN_POINT('Ctrl Pts',(19.5923918636366,-1.06191387672613,114.705932982827));
#56047=CARTESIAN_POINT('Ctrl Pts',(19.9091081456583,-0.628734129737697,
114.738490494062));
#56048=CARTESIAN_POINT('Ctrl Pts',(20.0436482399265,0.00136013336455928,
114.777578396996));
#56049=CARTESIAN_POINT('Ctrl Pts',(19.9090928165798,0.631655323772199,114.816681421648));
#56050=CARTESIAN_POINT('Ctrl Pts',(19.5286868815429,1.1521949790643,114.855796201813));
#56051=CARTESIAN_POINT('Ctrl Pts',(18.9687372623033,1.47200625927751,114.894919129408));
#56052=CARTESIAN_POINT('Ctrl Pts',(18.3269247722238,1.53523233022917,114.934046750203));
#56053=CARTESIAN_POINT('Ctrl Pts',(17.7152334288248,1.33076841613399,114.973175454517));
#56054=CARTESIAN_POINT('Ctrl Pts',(17.2404725580255,0.894349558877001,115.012301840373));
#56055=CARTESIAN_POINT('Ctrl Pts',(16.9853446354984,0.302108848816737,115.051422158546));
#56056=CARTESIAN_POINT('Ctrl Pts',(16.9934993376988,-0.27079628228924,115.086187634404));
#56057=CARTESIAN_POINT('Ctrl Pts',(17.1704122775008,-0.733300276011371,
115.116598560424));
#56058=CARTESIAN_POINT('Ctrl Pts',(17.3615831320585,-0.98758491633179,115.136144037193));
#56059=CARTESIAN_POINT('Ctrl Pts',(17.5154254407977,-1.13081668225498,115.149171118788));
#56060=CARTESIAN_POINT('Ctrl Pts',(17.5970581795022,-1.19692836165928,115.155684477762));
#56061=CARTESIAN_POINT('Ctrl Pts',(17.6831967780099,-1.25709479715135,115.162197134421));
#56062=CARTESIAN_POINT('Ctrl Pts',(17.8633620834074,-1.36516570458449,115.175222025971));
#56063=CARTESIAN_POINT('Ctrl Pts',(18.1604819038664,-1.47854845945174,115.194753812955));
#56064=CARTESIAN_POINT('Ctrl Pts',(18.582786890695,-1.51417568969967,115.220787745291));
#56065=CARTESIAN_POINT('Ctrl Pts',(18.9983836416472,-1.43149328105734,115.246809679889));
#56066=CARTESIAN_POINT('Ctrl Pts',(19.374473528925,-1.23714016652633,115.27282057109));
#56067=CARTESIAN_POINT('Ctrl Pts',(19.6822598946567,-0.946311359030486,
115.298817689622));
#56068=CARTESIAN_POINT('Ctrl Pts',(19.8967480474023,-0.582015055171165,
115.324801432878));
#56069=CARTESIAN_POINT('Ctrl Pts',(20.0386193688326,-0.0359715504243672,
115.359425895719));
#56070=CARTESIAN_POINT('Ctrl Pts',(19.941536265269,0.535299448860012,115.394018366274));
#56071=CARTESIAN_POINT('Ctrl Pts',(19.6668198938765,0.944384240575756,115.424255526598));
#56072=CARTESIAN_POINT('Ctrl Pts',(19.4671125145751,1.13894829771433,115.44152396901));
#56073=CARTESIAN_POINT('Ctrl Pts',(19.2416596715355,1.3035791132569,115.458786271138));
#56074=CARTESIAN_POINT('Ctrl Pts',(19.0175256336374,1.40399060754221,115.473882214218));
#56075=CARTESIAN_POINT('Ctrl Pts',(18.8150509122225,1.45460978349152,115.486814484407));
#56076=CARTESIAN_POINT('Ctrl Pts',(18.7124011810244,1.4728082953005,115.493279478184));
#56077=CARTESIAN_POINT('Ctrl Pts',(18.6259805295674,1.48196183269604,115.498665769091));
#56078=CARTESIAN_POINT('Ctrl Pts',(18.5565983881251,1.48554743331276,115.502974301951));
#56079=CARTESIAN_POINT('Ctrl Pts',(18.275006635137,1.49093350233563,115.520445423601));
#56080=CARTESIAN_POINT('Ctrl Pts',(17.7643189677256,1.36044159259875,115.552131188091));
#56081=CARTESIAN_POINT('Ctrl Pts',(17.3297966145357,0.957318076594017,115.587783846009));
#56082=CARTESIAN_POINT('Ctrl Pts',(17.1366050542202,0.593850002954031,115.613220643608));
#56083=CARTESIAN_POINT('Ctrl Pts',(17.0708721336454,0.399095376421441,115.625931295202));
#56084=CARTESIAN_POINT('Ctrl Pts',(17.0385717481457,0.238286256682236,115.636095006768));
#56085=CARTESIAN_POINT('Ctrl Pts',(17.0000053948983,-0.0873641069959773,
115.656416799589));
#56086=CARTESIAN_POINT('Ctrl Pts',(17.0954817402936,-0.627463061463085,
115.689403138097));
#56087=CARTESIAN_POINT('Ctrl Pts',(17.5683032047114,-1.2202390337612,115.734986014693));
#56088=CARTESIAN_POINT('Ctrl Pts',(18.2073749791171,-1.48915585063008,115.776682365231));
#56089=CARTESIAN_POINT('Ctrl Pts',(18.827714255502,-1.46536270236631,115.81451460932));
#56090=CARTESIAN_POINT('Ctrl Pts',(19.3387291215206,-1.24252555435953,115.848504801486));
#56091=CARTESIAN_POINT('Ctrl Pts',(19.7323390465761,-0.84870905484788,115.882433969696));
#56092=CARTESIAN_POINT('Ctrl Pts',(19.917317868452,-0.424382854990528,115.910656120296));
#56093=CARTESIAN_POINT('Ctrl Pts',(19.9647758151583,-0.0623666971425709,
115.933200950891));
#56094=CARTESIAN_POINT('Ctrl Pts',(19.9494967945027,0.210678396553568,115.950093741532));
#56095=CARTESIAN_POINT('Ctrl Pts',(19.8946537689314,0.431722595099945,115.964156440341));
#56096=CARTESIAN_POINT('Ctrl Pts',(19.8267524040723,0.599946781165768,115.975398400255));
#56097=CARTESIAN_POINT('Ctrl Pts',(19.7020401592803,0.841706463647344,115.992253058882));
#56098=CARTESIAN_POINT('Ctrl Pts',(19.4317853790293,1.15561589179994,116.017502153899));
#56099=CARTESIAN_POINT('Ctrl Pts',(18.9444409086331,1.41307035879397,116.051097502054));
#56100=CARTESIAN_POINT('Ctrl Pts',(18.3979015457458,1.47453073660614,116.084620132269));
#56101=CARTESIAN_POINT('Ctrl Pts',(18.0004069582635,1.36793073631313,116.1097063674));
#56102=CARTESIAN_POINT('Ctrl Pts',(17.763366663899,1.23962198295239,116.126406802779));
#56103=CARTESIAN_POINT('Ctrl Pts',(17.6140480708204,1.1398854968943,116.137534246267));
#56104=CARTESIAN_POINT('Ctrl Pts',(17.3790836560323,0.929981622126309,116.156989690435));
#56105=CARTESIAN_POINT('Ctrl Pts',(17.2215832331742,0.679602546844773,116.175024509631));
#56106=CARTESIAN_POINT('Ctrl Pts',(17.1450352066694,0.469669982396278,116.188878617737));
#56107=CARTESIAN_POINT('Ctrl Pts',(17.1249441446997,0.405767087289566,116.193033537477));
#56108=CARTESIAN_POINT('Ctrl Pts',(17.1079301441042,0.340970796669862,116.197187251518));
#56109=CARTESIAN_POINT('Ctrl Pts',(17.0939473695056,0.275494153967272,116.201339691278));
#56110=CARTESIAN_POINT('Ctrl Pts',(17.0830227708597,0.209443458520346,116.205490910608));
#56111=CARTESIAN_POINT('Ctrl Pts',(17.0726655652121,0.120824547382831,116.211024197657));
#56112=CARTESIAN_POINT('Ctrl Pts',(17.0610173800014,-0.124379540531134,
116.226234061721));
#56113=CARTESIAN_POINT('Ctrl Pts',(17.1369245229291,-0.5249310381429,116.251084258337));
#56114=CARTESIAN_POINT('Ctrl Pts',(17.4255200195769,-0.984001270082908,
116.284135719174));
#56115=CARTESIAN_POINT('Ctrl Pts',(17.8607605682645,-1.30506353431624,116.317102617813));
#56116=CARTESIAN_POINT('Ctrl Pts',(18.3818866043649,-1.44455243472689,116.349983938512));
#56117=CARTESIAN_POINT('Ctrl Pts',(18.916470350186,-1.38418902476214,116.382777928971));
#56118=CARTESIAN_POINT('Ctrl Pts',(19.3908578736671,-1.13333494037052,116.415483428707));
#56119=CARTESIAN_POINT('Ctrl Pts',(19.662129258784,-0.817824110576332,116.440850810503));
#56120=CARTESIAN_POINT('Ctrl Pts',(19.7921004518703,-0.556121431420674,
116.458936888485));
#56121=CARTESIAN_POINT('Ctrl Pts',(19.8690655500124,-0.335782443963777,
116.473391787428));
#56122=CARTESIAN_POINT('Ctrl Pts',(19.9308282800101,0.0701141608640084,
116.498652513443));
#56123=CARTESIAN_POINT('Ctrl Pts',(19.7975561020439,0.653379656102897,116.534635638022));
#56124=CARTESIAN_POINT('Ctrl Pts',(19.3238121146665,1.18955843336623,116.577647401962));
#56125=CARTESIAN_POINT('Ctrl Pts',(18.6542573597491,1.43288587092525,116.620488268205));
#56126=CARTESIAN_POINT('Ctrl Pts',(17.9525424324882,1.32679118729713,116.663155847902));
#56127=CARTESIAN_POINT('Ctrl Pts',(17.4716228570456,0.961996366384522,116.699450989897));
#56128=CARTESIAN_POINT('Ctrl Pts',(17.2242845453766,0.540894020126181,116.729451046567));
#56129=CARTESIAN_POINT('Ctrl Pts',(17.0944240343639,0.041457592091441,116.761140226464));
#56130=CARTESIAN_POINT('Ctrl Pts',(17.2055334687691,-0.610901669378824,
116.8006093271));
#56131=CARTESIAN_POINT('Ctrl Pts',(17.7327235525077,-1.19996474577183,116.847741724244));
#56132=CARTESIAN_POINT('Ctrl Pts',(18.4886274023919,-1.41711476065944,116.894641370113));
#56133=CARTESIAN_POINT('Ctrl Pts',(19.2403913761961,-1.19999329817096,116.941306241231));
#56134=CARTESIAN_POINT('Ctrl Pts',(19.7589583230562,-0.618976305235332,
116.987734609023));
#56135=CARTESIAN_POINT('Ctrl Pts',(19.866303857657,0.0173456111094613,117.026226666982));
#56136=CARTESIAN_POINT('Ctrl Pts',(19.7405351404932,0.500732911611066,117.05690073817));
#56137=CARTESIAN_POINT('Ctrl Pts',(19.5511427517233,0.822664799957136,117.079846452937));
#56138=CARTESIAN_POINT('Ctrl Pts',(19.2800271222083,1.07822752115069,117.102732140544));
#56139=CARTESIAN_POINT('Ctrl Pts',(18.840099008821,1.30647550082486,117.13316636068));
#56140=CARTESIAN_POINT('Ctrl Pts',(18.2057864265544,1.34185814168128,117.171058787474));
#56141=CARTESIAN_POINT('Ctrl Pts',(17.5421074842011,0.974328602971076,117.216288928054));
#56142=CARTESIAN_POINT('Ctrl Pts',(17.1777038347398,0.313792671011465,117.261278280207));
#56143=CARTESIAN_POINT('Ctrl Pts',(17.2203225463522,-0.435464225919962,
117.306027156934));
#56144=CARTESIAN_POINT('Ctrl Pts',(17.652724667813,-1.04386133116569,117.350536141848));
#56145=CARTESIAN_POINT('Ctrl Pts',(18.3388239098277,-1.32745573236693,117.39480611765));
#56146=CARTESIAN_POINT('Ctrl Pts',(19.0667149711576,-1.20320856043253,117.438838249758));
#56147=CARTESIAN_POINT('Ctrl Pts',(19.6139786084161,-0.713397943859653,
117.482633994782));
#56148=CARTESIAN_POINT('Ctrl Pts',(19.8156811381899,-0.0112791664943189,
117.526195091984));
#56149=CARTESIAN_POINT('Ctrl Pts',(19.6140022601783,0.686784214414896,117.569523562413));
#56150=CARTESIAN_POINT('Ctrl Pts',(19.0747275941947,1.16798331893147,117.612621710931));
#56151=CARTESIAN_POINT('Ctrl Pts',(18.3658643708616,1.28788138840837,117.655492120034));
#56152=CARTESIAN_POINT('Ctrl Pts',(17.7053431257873,1.01371279747136,117.69813764302));
#56153=CARTESIAN_POINT('Ctrl Pts',(17.2940790801678,0.433188982502828,117.740561406275));
#56154=CARTESIAN_POINT('Ctrl Pts',(17.2549003691858,-0.273508324804743,
117.782766808914));
#56155=CARTESIAN_POINT('Ctrl Pts',(17.5959737510632,-0.889574255288579,
117.824757505323));
#56156=CARTESIAN_POINT('Ctrl Pts',(18.2094168755739,-1.22806570874149,117.866537413039));
#56157=CARTESIAN_POINT('Ctrl Pts',(18.9055013390443,-1.18847566627298,117.908110699435));
#56158=CARTESIAN_POINT('Ctrl Pts',(19.4709991235593,-0.786645501256251,
117.949481800211));
#56159=CARTESIAN_POINT('Ctrl Pts',(19.7349121554302,-0.148494032303403,
117.990655350317));
#56160=CARTESIAN_POINT('Ctrl Pts',(19.6384296844279,0.41595364745626,118.024806143826));
#56161=CARTESIAN_POINT('Ctrl Pts',(19.3912822005401,0.783910465160815,118.052032979065));
#56162=CARTESIAN_POINT('Ctrl Pts',(19.0539455301924,1.06997780245999,118.079198326187));
#56163=CARTESIAN_POINT('Ctrl Pts',(18.5086041618223,1.22692728472169,118.113040992046));
#56164=CARTESIAN_POINT('Ctrl Pts',(17.8570681242743,1.03871258992206,118.153475788182));
#56165=CARTESIAN_POINT('Ctrl Pts',(17.4074661243136,0.535028360348281,118.193739748399));
#56166=CARTESIAN_POINT('Ctrl Pts',(17.295184410072,-0.12802353903353,118.233838994046));
#56167=CARTESIAN_POINT('Ctrl Pts',(17.5518536435643,-0.746678185841251,
118.273779650817));
#56168=CARTESIAN_POINT('Ctrl Pts',(18.09623557474,-1.13252353284961,118.313568149567));
#56169=CARTESIAN_POINT('Ctrl Pts',(18.7600131800788,-1.16944565236424,118.353211038631));
#56170=CARTESIAN_POINT('Ctrl Pts',(19.3396804878931,-0.848740522078599,
118.392715097256));
#56171=CARTESIAN_POINT('Ctrl Pts',(19.6587833880623,-0.270665095166121,
118.432087186673));
#56172=CARTESIAN_POINT('Ctrl Pts',(19.6216208701028,0.386364157140476,118.471334476116));
#56173=CARTESIAN_POINT('Ctrl Pts',(19.2416211971827,0.921545428620454,118.510464030869));
#56174=CARTESIAN_POINT('Ctrl Pts',(18.7378784200697,1.12977499085113,118.542980260458));
#56175=CARTESIAN_POINT('Ctrl Pts',(18.3152260681784,1.11706291748731,118.56894164302));
#56176=CARTESIAN_POINT('Ctrl Pts',(18.013631331558,1.02122659296196,118.588388203893));
#56177=CARTESIAN_POINT('Ctrl Pts',(17.7507020897944,0.845342251383026,118.607810663731));
#56178=CARTESIAN_POINT('Ctrl Pts',(17.5469576086983,0.604112404067775,118.62721063314));
#56179=CARTESIAN_POINT('Ctrl Pts',(17.418115189222,0.316066123273868,118.646588439489));
#56180=CARTESIAN_POINT('Ctrl Pts',(17.3740914074908,0.00406156609269027,
118.665945648007));
#56181=CARTESIAN_POINT('Ctrl Pts',(17.418105330468,-0.307731076500601,118.68528270408));
#56182=CARTESIAN_POINT('Ctrl Pts',(17.5252095909573,-0.546868258948941,
118.701381492349));
#56183=CARTESIAN_POINT('Ctrl Pts',(17.6479384162453,-0.714878730507821,
118.714251085885));
#56184=CARTESIAN_POINT('Ctrl Pts',(17.7929243818857,-0.863723509943578,
118.727115583167));
#56185=CARTESIAN_POINT('Ctrl Pts',(18.0972164483336,-1.06793358028532,118.74961267773));
#56186=CARTESIAN_POINT('Ctrl Pts',(18.6276378637832,-1.15815365828481,118.781712261723));
#56187=CARTESIAN_POINT('Ctrl Pts',(19.2238118827329,-0.91106020954,118.820176086249));
#56188=CARTESIAN_POINT('Ctrl Pts',(19.5340790733567,-0.473298914368946,
118.852189669591));
#56189=CARTESIAN_POINT('Ctrl Pts',(19.6045033571726,-0.115359348913955,
118.874582530202));
#56190=CARTESIAN_POINT('Ctrl Pts',(19.6017475647411,0.0911640829913528,
118.88737350014));
#56191=CARTESIAN_POINT('Ctrl Pts',(19.5700196370974,0.29559108219492,118.900162446911));
#56192=CARTESIAN_POINT('Ctrl Pts',(19.4770780543413,0.538342967989427,118.916143236651));
#56193=CARTESIAN_POINT('Ctrl Pts',(19.2273588011135,0.871529045839169,118.941704029868));
#56194=CARTESIAN_POINT('Ctrl Pts',(18.7588367207674,1.13058490335296,118.973640684375));
#56195=CARTESIAN_POINT('Ctrl Pts',(18.1172887995021,1.09452313569986,119.011950738852));
#56196=CARTESIAN_POINT('Ctrl Pts',(17.593388380079,0.722780783019972,119.050254797413));
#56197=CARTESIAN_POINT('Ctrl Pts',(17.3886684004257,0.228286678671025,119.082177254148));
#56198=CARTESIAN_POINT('Ctrl Pts',(17.4011923319186,-0.187547154371747,
119.107720239302));
#56199=CARTESIAN_POINT('Ctrl Pts',(17.479741012236,-0.43518291567232,119.123688362763));
#56200=CARTESIAN_POINT('Ctrl Pts',(17.5695979738663,-0.592074644579124,
119.134867535548));
#56201=CARTESIAN_POINT('Ctrl Pts',(17.6297289359476,-0.675697287840335,
119.1412564699));
#56202=CARTESIAN_POINT('Ctrl Pts',(17.6957161316275,-0.754921963867992,
119.147645877012));
#56203=CARTESIAN_POINT('Ctrl Pts',(17.7882499830905,-0.84489988474299,119.155633946795));
#56204=CARTESIAN_POINT('Ctrl Pts',(17.9550205699679,-0.966828303763707,
119.168415926821));
#56205=CARTESIAN_POINT('Ctrl Pts',(18.1925073400234,-1.07312652027406,119.184398568056));
#56206=CARTESIAN_POINT('Ctrl Pts',(18.5018237176362,-1.11680179614521,119.203585076302));
#56207=CARTESIAN_POINT('Ctrl Pts',(18.8112727437243,-1.07312083019676,119.222781017226));
#56208=CARTESIAN_POINT('Ctrl Pts',(19.0966922989243,-0.945425429896232,
119.241986576724));
#56209=CARTESIAN_POINT('Ctrl Pts',(19.3357397025375,-0.743574694906012,
119.261203548649));
#56210=CARTESIAN_POINT('Ctrl Pts',(19.5096763702265,-0.483296157484075,
119.280432047793));
#56211=CARTESIAN_POINT('Ctrl Pts',(19.604829263032,-0.184805761734769,119.299674358162));
#56212=CARTESIAN_POINT('Ctrl Pts',(19.6136282032755,0.128548869667553,119.318929822438));
#56213=CARTESIAN_POINT('Ctrl Pts',(19.5483562428395,0.381754662526241,119.334989622353));
#56214=CARTESIAN_POINT('Ctrl Pts',(19.4555027014667,0.567586338753027,119.347844753828));
#56215=CARTESIAN_POINT('Ctrl Pts',(19.3083285466207,0.781707993580481,119.363921119013));
#56216=CARTESIAN_POINT('Ctrl Pts',(19.0213883195784,1.0173014385066,119.386447876364));
#56217=CARTESIAN_POINT('Ctrl Pts',(18.5601806816014,1.14326482672377,119.415452744608));
#56218=CARTESIAN_POINT('Ctrl Pts',(18.0870469004768,1.06976794361554,119.444502870166));
#56219=CARTESIAN_POINT('Ctrl Pts',(17.6845073765261,0.809000046868888,119.473601565479));
#56220=CARTESIAN_POINT('Ctrl Pts',(17.4231181242213,0.405838898540841,119.502752060927));
#56221=CARTESIAN_POINT('Ctrl Pts',(17.3490598832109,-0.0697983875198877,
119.531957712525));
#56222=CARTESIAN_POINT('Ctrl Pts',(17.4759534440631,-0.535171725229621,
119.561221496182));
#56223=CARTESIAN_POINT('Ctrl Pts',(17.7314548399343,-0.846550437506931,
119.58565944407));
#56224=CARTESIAN_POINT('Ctrl Pts',(17.999207559364,-1.0170868157945,119.605241751292));
#56225=CARTESIAN_POINT('Ctrl Pts',(18.2967905723551,-1.12863703662001,119.624846422395));
#56226=CARTESIAN_POINT('Ctrl Pts',(18.701022235534,-1.14581433888424,119.649394327387));
#56227=CARTESIAN_POINT('Ctrl Pts',(19.1533010528138,-0.965969567310355,
119.678922596865));
#56228=CARTESIAN_POINT('Ctrl Pts',(19.4935242230618,-0.616264784255005,
119.708524488639));
#56229=CARTESIAN_POINT('Ctrl Pts',(19.6616806751607,-0.15688731828813,119.738203011753));
#56230=CARTESIAN_POINT('Ctrl Pts',(19.6274500840142,0.332402173060607,119.767961008938));
#56231=CARTESIAN_POINT('Ctrl Pts',(19.3957290628344,0.766238455283539,119.797801335606));
#56232=CARTESIAN_POINT('Ctrl Pts',(19.0059018782433,1.06845895995986,119.827726746298));
#56233=CARTESIAN_POINT('Ctrl Pts',(18.5252515327408,1.18543071772727,119.857739979944));
#56234=CARTESIAN_POINT('Ctrl Pts',(18.037234743022,1.09564506473,119.887843657137));
#56235=CARTESIAN_POINT('Ctrl Pts',(17.6956019306827,0.860470084296629,119.913007640695));
#56236=CARTESIAN_POINT('Ctrl Pts',(17.4972936032911,0.600305772965447,119.93318661626));
#56237=CARTESIAN_POINT('Ctrl Pts',(17.3569038509229,0.304279815543778,119.953397785618));
#56238=CARTESIAN_POINT('Ctrl Pts',(17.3041660284991,-0.109796929925252,
119.978723169803));
#56239=CARTESIAN_POINT('Ctrl Pts',(17.4498994353956,-0.59078091166106,120.009214030095));
#56240=CARTESIAN_POINT('Ctrl Pts',(17.7804655429487,-0.971566966837065,
120.039807705564));
#56241=CARTESIAN_POINT('Ctrl Pts',(18.2393086861239,-1.18486584665598,120.07050641441));
#56242=CARTESIAN_POINT('Ctrl Pts',(18.7470163437987,-1.1921729938516,120.101312384752));
#56243=CARTESIAN_POINT('Ctrl Pts',(19.215087635489,-0.990765643040621,120.132227714623));
#56244=CARTESIAN_POINT('Ctrl Pts',(19.5613155231427,-0.614392148089554,
120.163254460057));
#56245=CARTESIAN_POINT('Ctrl Pts',(19.7242152497417,-0.127659401515012,
120.194394583265));
#56246=CARTESIAN_POINT('Ctrl Pts',(19.6739207775415,0.385049104109546,120.225649979257));
#56247=CARTESIAN_POINT('Ctrl Pts',(19.4176458057697,0.834175476321175,120.257022460356));
#56248=CARTESIAN_POINT('Ctrl Pts',(18.998699632526,1.14061462596676,120.288513762116));
#56249=CARTESIAN_POINT('Ctrl Pts',(18.4891879156563,1.24962833189955,120.320125537776));
#56250=CARTESIAN_POINT('Ctrl Pts',(17.9776202690671,1.14060959036587,120.351859359126));
#56251=CARTESIAN_POINT('Ctrl Pts',(17.5535525982464,0.830952823101709,120.383716714854));
#56252=CARTESIAN_POINT('Ctrl Pts',(17.2919248389954,0.373308289212946,120.415699010712));
#56253=CARTESIAN_POINT('Ctrl Pts',(17.2398314509524,-0.153353235375788,
120.447807567348));
#56254=CARTESIAN_POINT('Ctrl Pts',(17.4080575955601,-0.657352082285856,
120.480043619757));
#56255=CARTESIAN_POINT('Ctrl Pts',(17.7689006127485,-1.05024513051325,120.512408315922));
#56256=CARTESIAN_POINT('Ctrl Pts',(18.2607097297302,-1.26233444597482,120.544902716827));
#56257=CARTESIAN_POINT('Ctrl Pts',(18.7984052352737,-1.25502080659343,120.577527795704));
#56258=CARTESIAN_POINT('Ctrl Pts',(19.2881848794747,-1.0278144553583,120.610284437319));
#56259=CARTESIAN_POINT('Ctrl Pts',(19.6438781749597,-0.61873033468329,120.643173436616));
#56260=CARTESIAN_POINT('Ctrl Pts',(19.8020987090859,-0.0979461688159152,
120.676195498978));
#56261=CARTESIAN_POINT('Ctrl Pts',(19.7335320823132,0.444227716269205,120.709351239055));
#56262=CARTESIAN_POINT('Ctrl Pts',(19.4483480211883,0.912997875362089,120.742641182014));
#56263=CARTESIAN_POINT('Ctrl Pts',(18.9947430992497,1.22566304840365,120.776065760162));
#56264=CARTESIAN_POINT('Ctrl Pts',(18.4508057834443,1.32618611440986,120.809625317582));
#56265=CARTESIAN_POINT('Ctrl Pts',(17.9110852264692,1.19525527808251,120.843320100399));
#56266=CARTESIAN_POINT('Ctrl Pts',(17.4701505494149,0.853917314146234,120.877150274951));
#56267=CARTESIAN_POINT('Ctrl Pts',(17.2060388865232,0.360310149126953,120.911115893666));
#56268=CARTESIAN_POINT('Ctrl Pts',(17.1664153816519,-0.200398871563149,
120.945216959522));
#56269=CARTESIAN_POINT('Ctrl Pts',(17.3116264220795,-0.597882955951257,
120.970894211169));
#56270=CARTESIAN_POINT('Ctrl Pts',(17.4713230749973,-0.824292723162997,
120.988054644643));
#56271=CARTESIAN_POINT('Ctrl Pts',(17.5930295495418,-0.963403094471689,
120.999506127854));
#56272=CARTESIAN_POINT('Ctrl Pts',(17.8429222056168,-1.17180944522949,121.019575839724));
#56273=CARTESIAN_POINT('Ctrl Pts',(18.2831358555107,-1.3472696457857,121.048331046648));
#56274=CARTESIAN_POINT('Ctrl Pts',(18.8536622082132,-1.32345121615729,121.082971735828));
#56275=CARTESIAN_POINT('Ctrl Pts',(19.3666123501032,-1.06776818445665,121.11774633767));
#56276=CARTESIAN_POINT('Ctrl Pts',(19.7318189194698,-0.623135744515387,
121.152654299799));
#56277=CARTESIAN_POINT('Ctrl Pts',(19.8841229814082,-0.0660261383455702,
121.187694946127));
#56278=CARTESIAN_POINT('Ctrl Pts',(19.7952691811095,0.506861240356869,121.22286752838));
#56279=CARTESIAN_POINT('Ctrl Pts',(19.4789909654556,0.995298037449156,121.258171199464));
#56280=CARTESIAN_POINT('Ctrl Pts',(18.9889997447394,1.31312136899922,121.293605027892));
#56281=CARTESIAN_POINT('Ctrl Pts',(18.4098258930854,1.40341469896206,121.329167991327));
#56282=CARTESIAN_POINT('Ctrl Pts',(17.8422514541543,1.2487159173822,121.364858980876));
#56283=CARTESIAN_POINT('Ctrl Pts',(17.3857498366357,0.874358654879244,121.400676801254));
#56284=CARTESIAN_POINT('Ctrl Pts',(17.1210452069084,0.344343613450397,121.436620170121));
#56285=CARTESIAN_POINT('Ctrl Pts',(17.0958251015548,-0.249607404749667,
121.472687721701));
#56286=CARTESIAN_POINT('Ctrl Pts',(17.3161507636215,-0.803935931388206,
121.508878001574));
#56287=CARTESIAN_POINT('Ctrl Pts',(17.7451068582081,-1.22131693446959,121.545189480257));
#56288=CARTESIAN_POINT('Ctrl Pts',(18.3089795239874,-1.42776624833079,121.581620531396));
#56289=CARTESIAN_POINT('Ctrl Pts',(18.9099344796403,-1.38575758159487,121.618169476059));
#56290=CARTESIAN_POINT('Ctrl Pts',(19.443003408243,-1.10105588624391,121.654834501032));
#56291=CARTESIAN_POINT('Ctrl Pts',(19.814447080578,-0.621956720707161,121.691613814933));
#56292=CARTESIAN_POINT('Ctrl Pts',(19.9582412943487,-0.0311460741792062,
121.728505359742));
#56293=CARTESIAN_POINT('Ctrl Pts',(19.8478423707596,0.568675584892993,121.765507307081));
#56294=CARTESIAN_POINT('Ctrl Pts',(19.5010738542693,1.07254435780881,121.802617407826));
#56295=CARTESIAN_POINT('Ctrl Pts',(18.9772465487843,1.39174398963045,121.839833580231));
#56296=CARTESIAN_POINT('Ctrl Pts',(18.3670349923433,1.46935809393124,121.877153590267));
#56297=CARTESIAN_POINT('Ctrl Pts',(17.7767415245785,1.29047771303663,121.91457510912));
#56298=CARTESIAN_POINT('Ctrl Pts',(17.3097639110163,0.88502066898406,121.952095792454));
#56299=CARTESIAN_POINT('Ctrl Pts',(17.0484530789278,0.322744770605088,121.98971320241));
#56300=CARTESIAN_POINT('Ctrl Pts',(17.0395741793232,-0.29877511550778,122.027424807101));
#56301=CARTESIAN_POINT('Ctrl Pts',(17.2859276060077,-0.871100232399064,
122.065228088574));
#56302=CARTESIAN_POINT('Ctrl Pts',(17.7456411246251,-1.29387701195727,122.103120366714));
#56303=CARTESIAN_POINT('Ctrl Pts',(18.3392916665445,-1.49245955151488,122.141098983942));
#56304=CARTESIAN_POINT('Ctrl Pts',(18.9636467540723,-1.43110986029732,122.179161195417));
#56305=CARTESIAN_POINT('Ctrl Pts',(19.5096427527803,-1.11943132446743,122.217304158637));
#56306=CARTESIAN_POINT('Ctrl Pts',(19.8814701962045,-0.610888906864692,
122.255525076564));
#56307=CARTESIAN_POINT('Ctrl Pts',(20.0134084028596,0.00638374819795061,
122.293820960483));
#56308=CARTESIAN_POINT('Ctrl Pts',(19.8814680357448,0.624863883396621,122.332188933733));
#56309=CARTESIAN_POINT('Ctrl Pts',(19.5077372244298,1.13643840843378,122.370625859871));
#56310=CARTESIAN_POINT('Ctrl Pts',(18.9567207702999,1.45127557085421,122.409128868261));
#56311=CARTESIAN_POINT('Ctrl Pts',(18.3241217337611,1.51368240153528,122.447694658652));
#56312=CARTESIAN_POINT('Ctrl Pts',(17.7202826349282,1.31196813537611,122.486320211507));
#56313=CARTESIAN_POINT('Ctrl Pts',(17.2508103246174,0.880536550537675,122.525002285958));
#56314=CARTESIAN_POINT('Ctrl Pts',(16.9981604164449,0.294249197224712,122.563737660687));
#56315=CARTESIAN_POINT('Ctrl Pts',(17.0060423714049,-0.274042958784632,
122.598213625129));
#56316=CARTESIAN_POINT('Ctrl Pts',(17.1818706810392,-0.73303144472968,122.628410343682));
#56317=CARTESIAN_POINT('Ctrl Pts',(17.5191721715142,-1.18310393837461,122.662947355674));
#56318=CARTESIAN_POINT('Ctrl Pts',(18.1531350042187,-1.53390972067408,122.706165522702));
#56319=CARTESIAN_POINT('Ctrl Pts',(19.0227874461394,-1.48519217492529,122.758094642985));
#56320=CARTESIAN_POINT('Ctrl Pts',(19.7338192740336,-0.980774656373063,
122.810082875595));
#56321=CARTESIAN_POINT('Ctrl Pts',(20.067922277282,-0.174626022127283,122.862122158172));
#56322=CARTESIAN_POINT('Ctrl Pts',(19.921708544036,0.68662933685667,122.914204231648));
#56323=CARTESIAN_POINT('Ctrl Pts',(19.4364076102001,1.22943043838242,122.957634782588));
#56324=CARTESIAN_POINT('Ctrl Pts',(18.9192757117743,1.45961435937841,122.992392354061));
#56325=CARTESIAN_POINT('Ctrl Pts',(18.5146998498917,1.51727349960696,123.017500336371));
#56326=CARTESIAN_POINT('Ctrl Pts',(18.1254479581993,1.46800683442712,123.041646590114));
#56327=CARTESIAN_POINT('Ctrl Pts',(17.65765089863,1.28524666288511,123.072557499479));
#56328=CARTESIAN_POINT('Ctrl Pts',(17.1864413110902,0.84817385210292,123.111201426539));
#56329=CARTESIAN_POINT('Ctrl Pts',(16.9818560590682,0.238917012125818,123.149847159061));
#56330=CARTESIAN_POINT('Ctrl Pts',(17.0077477842283,-0.262729802221198,
123.180762273051));
#56331=CARTESIAN_POINT('Ctrl Pts',(17.1549558342261,-0.742832495303323,
123.211674984775));
#56332=CARTESIAN_POINT('Ctrl Pts',(17.5555345576308,-1.24539323375308,123.250310351106));
#56333=CARTESIAN_POINT('Ctrl Pts',(18.2066766855254,-1.51951236558385,123.292795159863));
#56334=CARTESIAN_POINT('Ctrl Pts',(18.8397001520098,-1.49532848220801,123.331402485356));
#56335=CARTESIAN_POINT('Ctrl Pts',(19.361933038917,-1.2676766648096,123.36613474992));
#56336=CARTESIAN_POINT('Ctrl Pts',(19.7646594303858,-0.864798752237798,
123.400850262946));
#56337=CARTESIAN_POINT('Ctrl Pts',(19.992247479715,-0.343129638214644,123.435546682762));
#56338=CARTESIAN_POINT('Ctrl Pts',(20.0134975784261,0.225403110709894,123.470221342828));
#56339=CARTESIAN_POINT('Ctrl Pts',(19.8256820027275,0.761912608646907,123.504872214536));
#56340=CARTESIAN_POINT('Ctrl Pts',(19.516918297423,1.12076930887003,123.533725575818));
#56341=CARTESIAN_POINT('Ctrl Pts',(19.2041810039955,1.32499554631978,123.556794181975));
#56342=CARTESIAN_POINT('Ctrl Pts',(18.8020588760868,1.49233095074489,123.583695662073));
#56343=CARTESIAN_POINT('Ctrl Pts',(18.1960164011262,1.52254678614699,123.620174599657));
#56344=CARTESIAN_POINT('Ctrl Pts',(17.6216673694243,1.24564088295246,123.658522649907));
#56345=CARTESIAN_POINT('Ctrl Pts',(17.2833151529131,0.880111521286915,123.689167672577));
#56346=CARTESIAN_POINT('Ctrl Pts',(17.1050831264071,0.552606139546885,123.712134313292));
#56347=CARTESIAN_POINT('Ctrl Pts',(16.9816547923198,0.0706959663075114,
123.742732173804));
#56348=CARTESIAN_POINT('Ctrl Pts',(17.0529092044043,-0.496279877167484,
123.777112906262));
#56349=CARTESIAN_POINT('Ctrl Pts',(17.3864957981709,-1.02604026133052,123.815255128178));
#56350=CARTESIAN_POINT('Ctrl Pts',(17.857593613417,-1.37397111071324,123.850964243175));
#56351=CARTESIAN_POINT('Ctrl Pts',(18.4515962038669,-1.51829287387834,123.888044644597));
#56352=CARTESIAN_POINT('Ctrl Pts',(19.0746522170704,-1.40326627781162,123.926485479005));
#56353=CARTESIAN_POINT('Ctrl Pts',(19.5520449521414,-1.07433327180886,123.961659739466));
#56354=CARTESIAN_POINT('Ctrl Pts',(19.7870135179904,-0.729922634281818,
123.987199138138));
#56355=CARTESIAN_POINT('Ctrl Pts',(19.9172825726675,-0.412389600249223,
124.008461419526));
#56356=CARTESIAN_POINT('Ctrl Pts',(19.9813821346012,-0.0901260863987032,
124.028642265937));
#56357=CARTESIAN_POINT('Ctrl Pts',(19.9464919895927,0.322871316840072,124.054100150558));
#56358=CARTESIAN_POINT('Ctrl Pts',(19.7988560610193,0.709540527634926,124.079522689038));
#56359=CARTESIAN_POINT('Ctrl Pts',(19.5502809158787,1.03976970882056,124.104909666808));
#56360=CARTESIAN_POINT('Ctrl Pts',(19.2205019215012,1.28789198571529,124.130259814538));
#56361=CARTESIAN_POINT('Ctrl Pts',(18.8675304954949,1.42261786918923,124.153463104108));
#56362=CARTESIAN_POINT('Ctrl Pts',(18.5284830739033,1.46304402439271,124.174529127565));
#56363=CARTESIAN_POINT('Ctrl Pts',(18.1207874834896,1.4260614944801,124.199779233887));
#56364=CARTESIAN_POINT('Ctrl Pts',(17.6438940253866,1.2206283929953,124.231286143554));
#56365=CARTESIAN_POINT('Ctrl Pts',(17.2233006573008,0.762755887841534,124.269003086711));
#56366=CARTESIAN_POINT('Ctrl Pts',(17.0268753162689,0.174604680404742,124.306625880741));
#56367=CARTESIAN_POINT('Ctrl Pts',(17.0876702801681,-0.440949978759675,
124.344152137287));
#56368=CARTESIAN_POINT('Ctrl Pts',(17.3937696919832,-0.976537539345891,
124.381579352596));
#56369=CARTESIAN_POINT('Ctrl Pts',(17.8905867113653,-1.33941486357803,124.41890518565));
#56370=CARTESIAN_POINT('Ctrl Pts',(18.4906153716989,-1.46735186134762,124.456127313473));
#56371=CARTESIAN_POINT('Ctrl Pts',(19.0888593629504,-1.33941777641846,124.493243511411));
#56372=CARTESIAN_POINT('Ctrl Pts',(19.5812312587733,-0.97933823951139,124.530251612046));
#56373=CARTESIAN_POINT('Ctrl Pts',(19.8826841702414,-0.45113379238791,124.567149528264));
#56374=CARTESIAN_POINT('Ctrl Pts',(19.9419184246875,0.15228968271957,124.603935243626));
#56375=CARTESIAN_POINT('Ctrl Pts',(19.7501149544944,0.72549274055214,124.640606820178));
#56376=CARTESIAN_POINT('Ctrl Pts',(19.3422099788232,1.16895227798287,124.677162396834));
#56377=CARTESIAN_POINT('Ctrl Pts',(18.7905344628525,1.4063573661534,124.713600191806));
#56378=CARTESIAN_POINT('Ctrl Pts',(18.1919768114847,1.39775285517752,124.749918502117));
#56379=CARTESIAN_POINT('Ctrl Pts',(17.650949463827,1.14625964667207,124.786115706138));
#56380=CARTESIAN_POINT('Ctrl Pts',(17.2611574231578,0.697245715919318,124.822190264427));
#56381=CARTESIAN_POINT('Ctrl Pts',(17.0893550841156,0.130141700592976,124.858140721292));
#56382=CARTESIAN_POINT('Ctrl Pts',(17.1639091103876,-0.45562104348777,124.893965705161));
#56383=CARTESIAN_POINT('Ctrl Pts',(17.4701273616986,-0.958058662722596,
124.929663929076));
#56384=CARTESIAN_POINT('Ctrl Pts',(17.9531200725725,-1.29040433417455,124.965234192037));
#56385=CARTESIAN_POINT('Ctrl Pts',(18.5276405431088,-1.39610073357796,125.000675380104));
#56386=CARTESIAN_POINT('Ctrl Pts',(19.0931401580165,-1.25842381920182,125.035986467183));
#56387=CARTESIAN_POINT('Ctrl Pts',(19.5513770476802,-0.903101174061878,
125.071166515444));
#56388=CARTESIAN_POINT('Ctrl Pts',(19.8234925261704,-0.393520928653388,
125.106214675531));
#56389=CARTESIAN_POINT('Ctrl Pts',(19.863585446952,0.18057846519377,125.141130187601));
#56390=CARTESIAN_POINT('Ctrl Pts',(19.6664477552688,0.718918428921209,125.175912381995));
#56391=CARTESIAN_POINT('Ctrl Pts',(19.2681597354425,1.12820343239091,125.210560679702));
#56392=CARTESIAN_POINT('Ctrl Pts',(18.7394968083553,1.33829386724977,125.245074592494));
#56393=CARTESIAN_POINT('Ctrl Pts',(18.1733515600056,1.31422440666254,125.279453723019));
#56394=CARTESIAN_POINT('Ctrl Pts',(17.6684072336029,1.06200918227394,125.313697765461));
#56395=CARTESIAN_POINT('Ctrl Pts',(17.3119333434095,0.62727345561428,125.347806505814));
#56396=CARTESIAN_POINT('Ctrl Pts',(17.164703194465,0.0870075502303987,125.381779821996));
#56397=CARTESIAN_POINT('Ctrl Pts',(17.2506394082675,-0.464067284867245,
125.415617683646));
#56398=CARTESIAN_POINT('Ctrl Pts',(17.5529500312885,-0.93010635281992,125.449320152153));
#56399=CARTESIAN_POINT('Ctrl Pts',(18.0173742562096,-1.23080998259887,125.482887380882));
#56400=CARTESIAN_POINT('Ctrl Pts',(18.5619148970354,-1.31525442806852,125.516319615136));
#56401=CARTESIAN_POINT('Ctrl Pts',(19.0913123481237,-1.17050448618906,125.54961719185));
#56402=CARTESIAN_POINT('Ctrl Pts',(19.5137054329361,-0.823554001177106,
125.582780539051));
#56403=CARTESIAN_POINT('Ctrl Pts',(19.7565657136191,-0.336311890299757,
125.615810175785));
#56404=CARTESIAN_POINT('Ctrl Pts',(19.7791421686803,0.205437475860851,125.64870671201));
#56405=CARTESIAN_POINT('Ctrl Pts',(19.5792831503527,0.707131271594729,125.681470848156));
#56406=CARTESIAN_POINT('Ctrl Pts',(19.1934974783569,1.08192650056308,125.714103374504));
#56407=CARTESIAN_POINT('Ctrl Pts',(18.6903000531182,1.26572269937722,125.74660517022));
#56408=CARTESIAN_POINT('Ctrl Pts',(18.1580528586921,1.22811231780654,125.778977203127));
#56409=CARTESIAN_POINT('Ctrl Pts',(17.6894582924859,0.977390643756032,125.811220529498));
#56410=CARTESIAN_POINT('Ctrl Pts',(17.3654249182296,0.55880467658169,125.843336292948));
#56411=CARTESIAN_POINT('Ctrl Pts',(17.2411113552341,0.0464007134562138,
125.875325723779));
#56412=CARTESIAN_POINT('Ctrl Pts',(17.3365525714722,-0.470062155704644,
125.907190137343));
#56413=CARTESIAN_POINT('Ctrl Pts',(17.6334582774054,-0.900821679431447,
125.938930933878));
#56414=CARTESIAN_POINT('Ctrl Pts',(18.078689306533,-1.17169762162142,125.970549597961));
#56415=CARTESIAN_POINT('Ctrl Pts',(18.593754716555,-1.23684923441498,126.002047697117));
#56416=CARTESIAN_POINT('Ctrl Pts',(19.0886338471913,-1.0865147767173,126.033426880753));
#56417=CARTESIAN_POINT('Ctrl Pts',(19.4774918201155,-0.748430497103195,
126.064688878174));
#56418=CARTESIAN_POINT('Ctrl Pts',(19.6935481589647,-0.282732209663939,
126.095835498253));
#56419=CARTESIAN_POINT('Ctrl Pts',(19.7005261381603,0.228725868558277,126.126868628752));
#56420=CARTESIAN_POINT('Ctrl Pts',(19.4987238371462,0.696739517761545,126.157790234506));
#56421=CARTESIAN_POINT('Ctrl Pts',(19.1246955649095,1.04029099805458,126.188602356125));
#56422=CARTESIAN_POINT('Ctrl Pts',(18.6446468213007,1.20055180571536,126.219307107577));
#56423=CARTESIAN_POINT('Ctrl Pts',(18.1427337757278,1.15093580581614,126.24990667576));
#56424=CARTESIAN_POINT('Ctrl Pts',(17.7063324713574,0.901488522300449,126.280403319565));
#56425=CARTESIAN_POINT('Ctrl Pts',(17.4108529526162,0.496892712939118,126.310799367952));
#56426=CARTESIAN_POINT('Ctrl Pts',(17.3067328954843,0.0084812245335301,
126.34109721811));
#56427=CARTESIAN_POINT('Ctrl Pts',(17.4108490145204,-0.47831756693869,126.371299332964));
#56428=CARTESIAN_POINT('Ctrl Pts',(17.7038045321021,-0.878895943230857,
126.401408240409));
#56429=CARTESIAN_POINT('Ctrl Pts',(18.1335240920449,-1.12414442958507,126.431426532286));
#56430=CARTESIAN_POINT('Ctrl Pts',(18.6244919535479,-1.17234924842773,126.461356862258));
#56431=CARTESIAN_POINT('Ctrl Pts',(19.0909970917821,-1.01626672882518,126.491201943604));
#56432=CARTESIAN_POINT('Ctrl Pts',(19.4520665620905,-0.684179402726174,
126.520964546554));
#56433=CARTESIAN_POINT('Ctrl Pts',(19.6454906893739,-0.234786668051046,
126.550647497157));
#56434=CARTESIAN_POINT('Ctrl Pts',(19.6385159835268,0.253149219888882,126.580253676135));
#56435=CARTESIAN_POINT('Ctrl Pts',(19.4333722711128,0.694578566817253,126.609786017081));
#56436=CARTESIAN_POINT('Ctrl Pts',(19.0667063558325,1.01295613554844,126.639247502871));
#56437=CARTESIAN_POINT('Ctrl Pts',(18.6030514946211,1.1534838541102,126.668641164986));
#56438=CARTESIAN_POINT('Ctrl Pts',(18.1234957510667,1.09251755167767,126.697970077986));
#56439=CARTESIAN_POINT('Ctrl Pts',(17.7115308462464,0.841530068193854,126.727237365886));
#56440=CARTESIAN_POINT('Ctrl Pts',(17.4385535098235,0.444964463531077,126.756446186453));
#56441=CARTESIAN_POINT('Ctrl Pts',(17.3515170588706,-0.0276122872710075,
126.785599752877));
#56442=CARTESIAN_POINT('Ctrl Pts',(17.4648884689082,-0.493692017961726,
126.814701285522));
#56443=CARTESIAN_POINT('Ctrl Pts',(17.7582364067503,-0.872180645238306,
126.843754094616));
#56444=CARTESIAN_POINT('Ctrl Pts',(18.1799399597792,-1.09750112430032,126.872761421116));
#56445=CARTESIAN_POINT('Ctrl Pts',(18.6561791423461,-1.13087232076486,126.901726730967));
#56446=CARTESIAN_POINT('Ctrl Pts',(19.1039589342991,-0.967064360638307,
126.930653153623));
#56447=CARTESIAN_POINT('Ctrl Pts',(19.3883902256841,-0.690354148280827,
126.954729317772));
#56448=CARTESIAN_POINT('Ctrl Pts',(19.5332457227074,-0.414056911611768,
126.973973920849));
#56449=CARTESIAN_POINT('Ctrl Pts',(19.6177437769726,-0.113905111418309,
126.993208932229));
#56450=CARTESIAN_POINT('Ctrl Pts',(19.6011038359952,0.281732384417546,127.017234385341));
#56451=CARTESIAN_POINT('Ctrl Pts',(19.3890514321733,0.706565085330299,127.04604027079));
#56452=CARTESIAN_POINT('Ctrl Pts',(19.0223011451343,1.00751421476368,127.074824428941));
#56453=CARTESIAN_POINT('Ctrl Pts',(18.5648792017946,1.13234542273552,127.103590628698));
#56454=CARTESIAN_POINT('Ctrl Pts',(18.0966155583551,1.05950100369092,127.13234222422));
#56455=CARTESIAN_POINT('Ctrl Pts',(17.6990872091144,0.801854248777839,127.161082806753));
#56456=CARTESIAN_POINT('Ctrl Pts',(17.4415305074347,0.404417889894389,127.18981585486));
#56457=CARTESIAN_POINT('Ctrl Pts',(17.3687695530042,-0.0634870235218906,
127.218544916761));
#56458=CARTESIAN_POINT('Ctrl Pts',(17.4934609062107,-0.520295799873725,
127.247273508358));
#56459=CARTESIAN_POINT('Ctrl Pts',(17.7938846953223,-0.886376575644098,
127.276005163098));
#56460=CARTESIAN_POINT('Ctrl Pts',(18.2177247634987,-1.0978765550393,127.304743403475));
#56461=CARTESIAN_POINT('Ctrl Pts',(18.6911508939668,-1.11782834790528,127.333491753923));
#56462=CARTESIAN_POINT('Ctrl Pts',(19.1316465689169,-0.942594483611371,
127.362253727978));
#56463=CARTESIAN_POINT('Ctrl Pts',(19.4623516371648,-0.602527764442204,
127.391032833955));
#56464=CARTESIAN_POINT('Ctrl Pts',(19.6254375334004,-0.156728820867022,
127.419832557726));
#56465=CARTESIAN_POINT('Ctrl Pts',(19.5921943171502,0.317197263638082,127.448656399276));
#56466=CARTESIAN_POINT('Ctrl Pts',(19.368068361135,0.736614311055538,127.477507771776));
#56467=CARTESIAN_POINT('Ctrl Pts',(18.9917822982762,1.02822677014049,127.506390229474));
#56468=CARTESIAN_POINT('Ctrl Pts',(18.5286553795516,1.1408523543525,127.535306988223));
#56469=CARTESIAN_POINT('Ctrl Pts',(18.0593071007243,1.05438854513454,127.564261845145));
#56470=CARTESIAN_POINT('Ctrl Pts',(17.665645179454,0.78337931240486,127.593257348673));
#56471=CARTESIAN_POINT('Ctrl Pts',(17.4166255106301,0.374596672588247,127.622298651964));
#56472=CARTESIAN_POINT('Ctrl Pts',(17.356168808789,-0.10102697056375,127.651385319048));
#56473=CARTESIAN_POINT('Ctrl Pts',(17.4955452283241,-0.560666528004949,
127.680527574784));
#56474=CARTESIAN_POINT('Ctrl Pts',(17.8109503297906,-0.923997881438208,
127.709717292561));
#56475=CARTESIAN_POINT('Ctrl Pts',(18.2483725221223,-1.12713601481138,127.738975362331));
#56476=CARTESIAN_POINT('Ctrl Pts',(18.7311725427411,-1.13411043401417,127.768275574607));
#56477=CARTESIAN_POINT('Ctrl Pts',(19.1762783013378,-0.942422457862223,
127.797675015527));
#56478=CARTESIAN_POINT('Ctrl Pts',(19.5046484170361,-0.585761601815651,
127.827081897376));
#56479=CARTESIAN_POINT('Ctrl Pts',(19.6582495271737,-0.123680562238502,
127.85662756148));
#56480=CARTESIAN_POINT('Ctrl Pts',(19.6201095104048,0.280620801278878,127.881304584504));
#56481=CARTESIAN_POINT('Ctrl Pts',(19.4907597078714,0.572725205601487,127.900977353949));
#56482=CARTESIAN_POINT('Ctrl Pts',(19.3483928135265,0.768967247407983,127.915853796736));
#56483=CARTESIAN_POINT('Ctrl Pts',(19.1686762334047,0.931517072832566,127.930784609013));
#56484=CARTESIAN_POINT('Ctrl Pts',(18.9634686971736,1.051701521621,127.945656286825));
#56485=CARTESIAN_POINT('Ctrl Pts',(18.7395400780403,1.12529086281877,127.960455609962));
#56486=CARTESIAN_POINT('Ctrl Pts',(18.5767277357217,1.14299969027711,127.970442080495));
#56487=CARTESIAN_POINT('Ctrl Pts',(18.491314532458,1.14371857755274,127.975498274504));
#56488=CARTESIAN_POINT('Ctrl Pts',(18.319436888783,1.28857481063387,112.710548866174));
#56489=CARTESIAN_POINT('Ctrl Pts',(18.2367206542011,1.27796812314438,112.715656822746));
#56490=CARTESIAN_POINT('Ctrl Pts',(18.1122722696272,1.24996406005619,112.723602742685));
#56491=CARTESIAN_POINT('Ctrl Pts',(17.9105741471188,1.1715572059241,112.7372275449));
#56492=CARTESIAN_POINT('Ctrl Pts',(17.7147016928909,1.05680544825268,112.75142581384));
#56493=CARTESIAN_POINT('Ctrl Pts',(17.5092914781924,0.870936460786282,112.768496063499));
#56494=CARTESIAN_POINT('Ctrl Pts',(17.3452643787265,0.645338607702756,112.785608543142));
#56495=CARTESIAN_POINT('Ctrl Pts',(17.1949694671818,0.305633664533222,112.808486356608));
#56496=CARTESIAN_POINT('Ctrl Pts',(17.1504041586296,-0.163958059400556,
112.8371493128));
#56497=CARTESIAN_POINT('Ctrl Pts',(17.3295581344551,-0.704127606930189,
112.871679546659));
#56498=CARTESIAN_POINT('Ctrl Pts',(17.7163063911852,-1.12497913550319,112.906352649458));
#56499=CARTESIAN_POINT('Ctrl Pts',(18.2431925961433,-1.35205912276461,112.941152109412));
#56500=CARTESIAN_POINT('Ctrl Pts',(18.8187741112765,-1.34427642838518,112.976089285723));
#56501=CARTESIAN_POINT('Ctrl Pts',(19.3432395618757,-1.10098396627254,113.011156346434));
#56502=CARTESIAN_POINT('Ctrl Pts',(19.7238494382154,-0.663159822701633,
113.046357078694));
#56503=CARTESIAN_POINT('Ctrl Pts',(19.8931314314799,-0.105956319615994,
113.08168722595));
#56504=CARTESIAN_POINT('Ctrl Pts',(19.8197719071333,0.473908286429459,113.117148366555));
#56505=CARTESIAN_POINT('Ctrl Pts',(19.514861434432,0.975046989864885,113.152737815001));
#56506=CARTESIAN_POINT('Ctrl Pts',(19.0301258646803,1.30913564752012,113.188455340763));
#56507=CARTESIAN_POINT('Ctrl Pts',(18.4491549165285,1.416472562517,113.224299311997));
#56508=CARTESIAN_POINT('Ctrl Pts',(17.8730091730699,1.27666467315962,113.260268611474));
#56509=CARTESIAN_POINT('Ctrl Pts',(17.4026034483492,0.912474225359778,113.296361769111));
#56510=CARTESIAN_POINT('Ctrl Pts',(17.1210280345443,0.386131812194797,113.332577359437));
#56511=CARTESIAN_POINT('Ctrl Pts',(17.0788544181136,-0.211299879373549,
113.368913814958));
#56512=CARTESIAN_POINT('Ctrl Pts',(17.2850565553758,-0.775695991436841,
113.405369493798));
#56513=CARTESIAN_POINT('Ctrl Pts',(17.705146965038,-1.20803167965084,113.441942712263));
#56514=CARTESIAN_POINT('Ctrl Pts',(18.2669652505624,-1.43177932086286,113.478631613973));
#56515=CARTESIAN_POINT('Ctrl Pts',(18.8730309513044,-1.40645905314605,113.51543444437));
#56516=CARTESIAN_POINT('Ctrl Pts',(19.4175618056869,-1.13497091574588,113.55234907248));
#56517=CARTESIAN_POINT('Ctrl Pts',(19.8048480383929,-0.663350581086933,
113.589373656825));
#56518=CARTESIAN_POINT('Ctrl Pts',(19.966197057422,-0.0729778537808475,
113.626505971993));
#56519=CARTESIAN_POINT('Ctrl Pts',(19.8720657245217,0.533549954628291,113.663743893195));
#56520=CARTESIAN_POINT('Ctrl Pts',(19.5374817640394,1.0501311842453,113.701085198819));
#56521=CARTESIAN_POINT('Ctrl Pts',(19.0196808505253,1.38594482959087,113.738527490934));
#56522=CARTESIAN_POINT('Ctrl Pts',(18.5101754020758,1.46526119175664,113.769811704289));
#56523=CARTESIAN_POINT('Ctrl Pts',(18.1090240872925,1.39960741569811,113.794887075397));
#56524=CARTESIAN_POINT('Ctrl Pts',(17.729655069815,1.25220225914757,113.819994103033));
#56525=CARTESIAN_POINT('Ctrl Pts',(17.3289300722954,0.923586877948104,113.851436567131));
#56526=CARTESIAN_POINT('Ctrl Pts',(17.0504721252432,0.365805609893722,113.889258509496));
#56527=CARTESIAN_POINT('Ctrl Pts',(17.0240290762783,-0.258477757917008,
113.927168961164));
#56528=CARTESIAN_POINT('Ctrl Pts',(17.2554238425403,-0.840447617959809,
113.965165177094));
#56529=CARTESIAN_POINT('Ctrl Pts',(17.7053131011304,-1.27808626113464,114.003244380208));
#56530=CARTESIAN_POINT('Ctrl Pts',(18.2959641544648,-1.49425702735341,114.041403784502));
#56531=CARTESIAN_POINT('Ctrl Pts',(18.9246622805112,-1.4502272181577,114.079640512388));
#56532=CARTESIAN_POINT('Ctrl Pts',(19.4816239236303,-1.15267110135651,114.117951609114));
#56533=CARTESIAN_POINT('Ctrl Pts',(19.8691907107327,-0.652639427392253,
114.156334167846));
#56534=CARTESIAN_POINT('Ctrl Pts',(20.0189810591327,-0.03683256961316,114.194785080069));
#56535=CARTESIAN_POINT('Ctrl Pts',(19.9039833865991,0.587522999416328,114.2333013558));
#56536=CARTESIAN_POINT('Ctrl Pts',(19.5434230734537,1.11127572106957,114.271879839515));
#56537=CARTESIAN_POINT('Ctrl Pts',(18.9995399107886,1.44259279852258,114.310517384521));
#56538=CARTESIAN_POINT('Ctrl Pts',(18.3668596633944,1.52297273199859,114.349210799966));
#56539=CARTESIAN_POINT('Ctrl Pts',(17.7556977562459,1.33767203016567,114.387956849117));
#56540=CARTESIAN_POINT('Ctrl Pts',(17.272914349715,0.918370107647551,114.426752263094));
#56541=CARTESIAN_POINT('Ctrl Pts',(17.0031861863323,0.337753138207008,114.46559374694));
#56542=CARTESIAN_POINT('Ctrl Pts',(16.9941242219495,-0.303088855509916,
114.504477951706));
#56543=CARTESIAN_POINT('Ctrl Pts',(17.2478715429229,-0.892350566926149,
114.543401543985));
#56544=CARTESIAN_POINT('Ctrl Pts',(17.720592505509,-1.32694200600498,114.582361077963));
#56545=CARTESIAN_POINT('Ctrl Pts',(18.3301332049521,-1.53077558802408,114.621353247865));
#56546=CARTESIAN_POINT('Ctrl Pts',(18.8635057740616,-1.47820468577621,114.653870882415));
#56547=CARTESIAN_POINT('Ctrl Pts',(19.2496685905278,-1.30821665552171,114.679897931973));
#56548=CARTESIAN_POINT('Ctrl Pts',(19.5923918636366,-1.06191387672613,114.705932982827));
#56549=CARTESIAN_POINT('Ctrl Pts',(19.9091081456583,-0.628734129737697,
114.738490494062));
#56550=CARTESIAN_POINT('Ctrl Pts',(20.0436482399265,0.00136013336455928,
114.777578396996));
#56551=CARTESIAN_POINT('Ctrl Pts',(19.9090928165798,0.631655323772199,114.816681421648));
#56552=CARTESIAN_POINT('Ctrl Pts',(19.5286868815429,1.1521949790643,114.855796201813));
#56553=CARTESIAN_POINT('Ctrl Pts',(18.9687372623033,1.47200625927751,114.894919129408));
#56554=CARTESIAN_POINT('Ctrl Pts',(18.3269247722238,1.53523233022917,114.934046750203));
#56555=CARTESIAN_POINT('Ctrl Pts',(17.7152334288248,1.33076841613399,114.973175454517));
#56556=CARTESIAN_POINT('Ctrl Pts',(17.2404725580255,0.894349558877001,115.012301840373));
#56557=CARTESIAN_POINT('Ctrl Pts',(16.9853446354984,0.302108848816737,115.051422158546));
#56558=CARTESIAN_POINT('Ctrl Pts',(16.9934993376988,-0.27079628228924,115.086187634404));
#56559=CARTESIAN_POINT('Ctrl Pts',(17.1704122775008,-0.733300276011371,
115.116598560424));
#56560=CARTESIAN_POINT('Ctrl Pts',(17.3615831320585,-0.98758491633179,115.136144037193));
#56561=CARTESIAN_POINT('Ctrl Pts',(17.5154254407977,-1.13081668225498,115.149171118788));
#56562=CARTESIAN_POINT('Ctrl Pts',(17.5970581795022,-1.19692836165928,115.155684477762));
#56563=CARTESIAN_POINT('Ctrl Pts',(17.6831967780099,-1.25709479715135,115.162197134421));
#56564=CARTESIAN_POINT('Ctrl Pts',(17.8633620834074,-1.36516570458449,115.175222025971));
#56565=CARTESIAN_POINT('Ctrl Pts',(18.1604819038664,-1.47854845945174,115.194753812955));
#56566=CARTESIAN_POINT('Ctrl Pts',(18.582786890695,-1.51417568969967,115.220787745291));
#56567=CARTESIAN_POINT('Ctrl Pts',(18.9983836416472,-1.43149328105734,115.246809679889));
#56568=CARTESIAN_POINT('Ctrl Pts',(19.374473528925,-1.23714016652633,115.27282057109));
#56569=CARTESIAN_POINT('Ctrl Pts',(19.6822598946567,-0.946311359030486,
115.298817689622));
#56570=CARTESIAN_POINT('Ctrl Pts',(19.8967480474023,-0.582015055171165,
115.324801432878));
#56571=CARTESIAN_POINT('Ctrl Pts',(20.0386193688326,-0.0359715504243672,
115.359425895719));
#56572=CARTESIAN_POINT('Ctrl Pts',(19.941536265269,0.535299448860012,115.394018366274));
#56573=CARTESIAN_POINT('Ctrl Pts',(19.6668198938765,0.944384240575756,115.424255526598));
#56574=CARTESIAN_POINT('Ctrl Pts',(19.4671125145751,1.13894829771433,115.44152396901));
#56575=CARTESIAN_POINT('Ctrl Pts',(19.2416596715355,1.3035791132569,115.458786271138));
#56576=CARTESIAN_POINT('Ctrl Pts',(19.0175256336374,1.40399060754221,115.473882214218));
#56577=CARTESIAN_POINT('Ctrl Pts',(18.8150509122225,1.45460978349152,115.486814484407));
#56578=CARTESIAN_POINT('Ctrl Pts',(18.7124011810244,1.4728082953005,115.493279478184));
#56579=CARTESIAN_POINT('Ctrl Pts',(18.6259805295674,1.48196183269604,115.498665769091));
#56580=CARTESIAN_POINT('Ctrl Pts',(18.5565983881251,1.48554743331276,115.502974301951));
#56581=CARTESIAN_POINT('Ctrl Pts',(18.275006635137,1.49093350233563,115.520445423601));
#56582=CARTESIAN_POINT('Ctrl Pts',(17.7643189677256,1.36044159259875,115.552131188091));
#56583=CARTESIAN_POINT('Ctrl Pts',(17.3297966145357,0.957318076594017,115.587783846009));
#56584=CARTESIAN_POINT('Ctrl Pts',(17.1366050542202,0.593850002954031,115.613220643608));
#56585=CARTESIAN_POINT('Ctrl Pts',(17.0708721336454,0.399095376421441,115.625931295202));
#56586=CARTESIAN_POINT('Ctrl Pts',(17.0385717481457,0.238286256682236,115.636095006768));
#56587=CARTESIAN_POINT('Ctrl Pts',(17.0000053948983,-0.0873641069959773,
115.656416799589));
#56588=CARTESIAN_POINT('Ctrl Pts',(17.0954817402936,-0.627463061463085,
115.689403138097));
#56589=CARTESIAN_POINT('Ctrl Pts',(17.5683032047114,-1.2202390337612,115.734986014693));
#56590=CARTESIAN_POINT('Ctrl Pts',(18.2073749791171,-1.48915585063008,115.776682365231));
#56591=CARTESIAN_POINT('Ctrl Pts',(18.827714255502,-1.46536270236631,115.81451460932));
#56592=CARTESIAN_POINT('Ctrl Pts',(19.3387291215206,-1.24252555435953,115.848504801486));
#56593=CARTESIAN_POINT('Ctrl Pts',(19.7323390465761,-0.84870905484788,115.882433969696));
#56594=CARTESIAN_POINT('Ctrl Pts',(19.917317868452,-0.424382854990528,115.910656120296));
#56595=CARTESIAN_POINT('Ctrl Pts',(19.9647758151583,-0.0623666971425709,
115.933200950891));
#56596=CARTESIAN_POINT('Ctrl Pts',(19.9494967945027,0.210678396553568,115.950093741532));
#56597=CARTESIAN_POINT('Ctrl Pts',(19.8946537689314,0.431722595099945,115.964156440341));
#56598=CARTESIAN_POINT('Ctrl Pts',(19.8267524040723,0.599946781165768,115.975398400255));
#56599=CARTESIAN_POINT('Ctrl Pts',(19.7020401592803,0.841706463647344,115.992253058882));
#56600=CARTESIAN_POINT('Ctrl Pts',(19.4317853790293,1.15561589179994,116.017502153899));
#56601=CARTESIAN_POINT('Ctrl Pts',(18.9444409086331,1.41307035879397,116.051097502054));
#56602=CARTESIAN_POINT('Ctrl Pts',(18.3979015457458,1.47453073660614,116.084620132269));
#56603=CARTESIAN_POINT('Ctrl Pts',(18.0004069582635,1.36793073631313,116.1097063674));
#56604=CARTESIAN_POINT('Ctrl Pts',(17.763366663899,1.23962198295239,116.126406802779));
#56605=CARTESIAN_POINT('Ctrl Pts',(17.6140480708204,1.1398854968943,116.137534246267));
#56606=CARTESIAN_POINT('Ctrl Pts',(17.3790836560323,0.929981622126309,116.156989690435));
#56607=CARTESIAN_POINT('Ctrl Pts',(17.2215832331742,0.679602546844773,116.175024509631));
#56608=CARTESIAN_POINT('Ctrl Pts',(17.1450352066694,0.469669982396278,116.188878617737));
#56609=CARTESIAN_POINT('Ctrl Pts',(17.1249441446997,0.405767087289566,116.193033537477));
#56610=CARTESIAN_POINT('Ctrl Pts',(17.1079301441042,0.340970796669862,116.197187251518));
#56611=CARTESIAN_POINT('Ctrl Pts',(17.0939473695056,0.275494153967272,116.201339691278));
#56612=CARTESIAN_POINT('Ctrl Pts',(17.0830227708597,0.209443458520346,116.205490910608));
#56613=CARTESIAN_POINT('Ctrl Pts',(17.0726655652121,0.120824547382831,116.211024197657));
#56614=CARTESIAN_POINT('Ctrl Pts',(17.0610173800014,-0.124379540531134,
116.226234061721));
#56615=CARTESIAN_POINT('Ctrl Pts',(17.1369245229291,-0.5249310381429,116.251084258337));
#56616=CARTESIAN_POINT('Ctrl Pts',(17.4255200195769,-0.984001270082908,
116.284135719174));
#56617=CARTESIAN_POINT('Ctrl Pts',(17.8607605682645,-1.30506353431624,116.317102617813));
#56618=CARTESIAN_POINT('Ctrl Pts',(18.3818866043649,-1.44455243472689,116.349983938512));
#56619=CARTESIAN_POINT('Ctrl Pts',(18.916470350186,-1.38418902476214,116.382777928971));
#56620=CARTESIAN_POINT('Ctrl Pts',(19.3908578736671,-1.13333494037052,116.415483428707));
#56621=CARTESIAN_POINT('Ctrl Pts',(19.662129258784,-0.817824110576332,116.440850810503));
#56622=CARTESIAN_POINT('Ctrl Pts',(19.7921004518703,-0.556121431420674,
116.458936888485));
#56623=CARTESIAN_POINT('Ctrl Pts',(19.8690655500124,-0.335782443963777,
116.473391787428));
#56624=CARTESIAN_POINT('Ctrl Pts',(19.9308282800101,0.0701141608640084,
116.498652513443));
#56625=CARTESIAN_POINT('Ctrl Pts',(19.7975561020439,0.653379656102897,116.534635638022));
#56626=CARTESIAN_POINT('Ctrl Pts',(19.3238121146665,1.18955843336623,116.577647401962));
#56627=CARTESIAN_POINT('Ctrl Pts',(18.6542573597491,1.43288587092525,116.620488268205));
#56628=CARTESIAN_POINT('Ctrl Pts',(17.9525424324882,1.32679118729713,116.663155847902));
#56629=CARTESIAN_POINT('Ctrl Pts',(17.4716228570456,0.961996366384522,116.699450989897));
#56630=CARTESIAN_POINT('Ctrl Pts',(17.2242845453766,0.540894020126181,116.729451046567));
#56631=CARTESIAN_POINT('Ctrl Pts',(17.0944240343639,0.041457592091441,116.761140226464));
#56632=CARTESIAN_POINT('Ctrl Pts',(17.2055334687691,-0.610901669378824,
116.8006093271));
#56633=CARTESIAN_POINT('Ctrl Pts',(17.7327235525077,-1.19996474577183,116.847741724244));
#56634=CARTESIAN_POINT('Ctrl Pts',(18.4886274023919,-1.41711476065944,116.894641370113));
#56635=CARTESIAN_POINT('Ctrl Pts',(19.2403913761961,-1.19999329817096,116.941306241231));
#56636=CARTESIAN_POINT('Ctrl Pts',(19.7589583230562,-0.618976305235332,
116.987734609023));
#56637=CARTESIAN_POINT('Ctrl Pts',(19.866303857657,0.0173456111094613,117.026226666982));
#56638=CARTESIAN_POINT('Ctrl Pts',(19.7405351404932,0.500732911611066,117.05690073817));
#56639=CARTESIAN_POINT('Ctrl Pts',(19.5511427517233,0.822664799957136,117.079846452937));
#56640=CARTESIAN_POINT('Ctrl Pts',(19.2800271222083,1.07822752115069,117.102732140544));
#56641=CARTESIAN_POINT('Ctrl Pts',(18.840099008821,1.30647550082486,117.13316636068));
#56642=CARTESIAN_POINT('Ctrl Pts',(18.2057864265544,1.34185814168128,117.171058787474));
#56643=CARTESIAN_POINT('Ctrl Pts',(17.5421074842011,0.974328602971076,117.216288928054));
#56644=CARTESIAN_POINT('Ctrl Pts',(17.1777038347398,0.313792671011465,117.261278280207));
#56645=CARTESIAN_POINT('Ctrl Pts',(17.2203225463522,-0.435464225919962,
117.306027156934));
#56646=CARTESIAN_POINT('Ctrl Pts',(17.652724667813,-1.04386133116569,117.350536141848));
#56647=CARTESIAN_POINT('Ctrl Pts',(18.3388239098277,-1.32745573236693,117.39480611765));
#56648=CARTESIAN_POINT('Ctrl Pts',(19.0667149711576,-1.20320856043253,117.438838249758));
#56649=CARTESIAN_POINT('Ctrl Pts',(19.6139786084161,-0.713397943859653,
117.482633994782));
#56650=CARTESIAN_POINT('Ctrl Pts',(19.8156811381899,-0.0112791664943189,
117.526195091984));
#56651=CARTESIAN_POINT('Ctrl Pts',(19.6140022601783,0.686784214414896,117.569523562413));
#56652=CARTESIAN_POINT('Ctrl Pts',(19.0747275941947,1.16798331893147,117.612621710931));
#56653=CARTESIAN_POINT('Ctrl Pts',(18.3658643708616,1.28788138840837,117.655492120034));
#56654=CARTESIAN_POINT('Ctrl Pts',(17.7053431257873,1.01371279747136,117.69813764302));
#56655=CARTESIAN_POINT('Ctrl Pts',(17.2940790801678,0.433188982502828,117.740561406275));
#56656=CARTESIAN_POINT('Ctrl Pts',(17.2549003691858,-0.273508324804743,
117.782766808914));
#56657=CARTESIAN_POINT('Ctrl Pts',(17.5959737510632,-0.889574255288579,
117.824757505323));
#56658=CARTESIAN_POINT('Ctrl Pts',(18.2094168755739,-1.22806570874149,117.866537413039));
#56659=CARTESIAN_POINT('Ctrl Pts',(18.9055013390443,-1.18847566627298,117.908110699435));
#56660=CARTESIAN_POINT('Ctrl Pts',(19.4709991235593,-0.786645501256251,
117.949481800211));
#56661=CARTESIAN_POINT('Ctrl Pts',(19.7349121554302,-0.148494032303403,
117.990655350317));
#56662=CARTESIAN_POINT('Ctrl Pts',(19.6384296844279,0.41595364745626,118.024806143826));
#56663=CARTESIAN_POINT('Ctrl Pts',(19.3912822005401,0.783910465160815,118.052032979065));
#56664=CARTESIAN_POINT('Ctrl Pts',(19.0539455301924,1.06997780245999,118.079198326187));
#56665=CARTESIAN_POINT('Ctrl Pts',(18.5086041618223,1.22692728472169,118.113040992046));
#56666=CARTESIAN_POINT('Ctrl Pts',(17.8570681242743,1.03871258992206,118.153475788182));
#56667=CARTESIAN_POINT('Ctrl Pts',(17.4074661243136,0.535028360348281,118.193739748399));
#56668=CARTESIAN_POINT('Ctrl Pts',(17.295184410072,-0.12802353903353,118.233838994046));
#56669=CARTESIAN_POINT('Ctrl Pts',(17.5518536435643,-0.746678185841251,
118.273779650817));
#56670=CARTESIAN_POINT('Ctrl Pts',(18.09623557474,-1.13252353284961,118.313568149567));
#56671=CARTESIAN_POINT('Ctrl Pts',(18.7600131800788,-1.16944565236424,118.353211038631));
#56672=CARTESIAN_POINT('Ctrl Pts',(19.3396804878931,-0.848740522078599,
118.392715097256));
#56673=CARTESIAN_POINT('Ctrl Pts',(19.6587833880623,-0.270665095166121,
118.432087186673));
#56674=CARTESIAN_POINT('Ctrl Pts',(19.6216208701028,0.386364157140476,118.471334476116));
#56675=CARTESIAN_POINT('Ctrl Pts',(19.2416211971827,0.921545428620454,118.510464030869));
#56676=CARTESIAN_POINT('Ctrl Pts',(18.7378784200697,1.12977499085113,118.542980260458));
#56677=CARTESIAN_POINT('Ctrl Pts',(18.3152260681784,1.11706291748731,118.56894164302));
#56678=CARTESIAN_POINT('Ctrl Pts',(18.013631331558,1.02122659296196,118.588388203893));
#56679=CARTESIAN_POINT('Ctrl Pts',(17.7507020897944,0.845342251383026,118.607810663731));
#56680=CARTESIAN_POINT('Ctrl Pts',(17.5469576086983,0.604112404067775,118.62721063314));
#56681=CARTESIAN_POINT('Ctrl Pts',(17.418115189222,0.316066123273868,118.646588439489));
#56682=CARTESIAN_POINT('Ctrl Pts',(17.3740914074908,0.00406156609269027,
118.665945648007));
#56683=CARTESIAN_POINT('Ctrl Pts',(17.418105330468,-0.307731076500601,118.68528270408));
#56684=CARTESIAN_POINT('Ctrl Pts',(17.5252095909573,-0.546868258948941,
118.701381492349));
#56685=CARTESIAN_POINT('Ctrl Pts',(17.6479384162453,-0.714878730507821,
118.714251085885));
#56686=CARTESIAN_POINT('Ctrl Pts',(17.7929243818857,-0.863723509943578,
118.727115583167));
#56687=CARTESIAN_POINT('Ctrl Pts',(18.0972164483336,-1.06793358028532,118.74961267773));
#56688=CARTESIAN_POINT('Ctrl Pts',(18.6276378637832,-1.15815365828481,118.781712261723));
#56689=CARTESIAN_POINT('Ctrl Pts',(19.2238118827329,-0.91106020954,118.820176086249));
#56690=CARTESIAN_POINT('Ctrl Pts',(19.5340790733567,-0.473298914368946,
118.852189669591));
#56691=CARTESIAN_POINT('Ctrl Pts',(19.6045033571726,-0.115359348913955,
118.874582530202));
#56692=CARTESIAN_POINT('Ctrl Pts',(19.6017475647411,0.0911640829913528,
118.88737350014));
#56693=CARTESIAN_POINT('Ctrl Pts',(19.5700196370974,0.29559108219492,118.900162446911));
#56694=CARTESIAN_POINT('Ctrl Pts',(19.4770780543413,0.538342967989427,118.916143236651));
#56695=CARTESIAN_POINT('Ctrl Pts',(19.2273588011135,0.871529045839169,118.941704029868));
#56696=CARTESIAN_POINT('Ctrl Pts',(18.7588367207674,1.13058490335296,118.973640684375));
#56697=CARTESIAN_POINT('Ctrl Pts',(18.1172887995021,1.09452313569986,119.011950738852));
#56698=CARTESIAN_POINT('Ctrl Pts',(17.593388380079,0.722780783019972,119.050254797413));
#56699=CARTESIAN_POINT('Ctrl Pts',(17.3886684004257,0.228286678671025,119.082177254148));
#56700=CARTESIAN_POINT('Ctrl Pts',(17.4011923319186,-0.187547154371747,
119.107720239302));
#56701=CARTESIAN_POINT('Ctrl Pts',(17.479741012236,-0.43518291567232,119.123688362763));
#56702=CARTESIAN_POINT('Ctrl Pts',(17.5695979738663,-0.592074644579124,
119.134867535548));
#56703=CARTESIAN_POINT('Ctrl Pts',(17.6297289359476,-0.675697287840335,
119.1412564699));
#56704=CARTESIAN_POINT('Ctrl Pts',(17.6957161316275,-0.754921963867992,
119.147645877012));
#56705=CARTESIAN_POINT('Ctrl Pts',(17.7882499830905,-0.84489988474299,119.155633946795));
#56706=CARTESIAN_POINT('Ctrl Pts',(17.9550205699679,-0.966828303763707,
119.168415926821));
#56707=CARTESIAN_POINT('Ctrl Pts',(18.1925073400234,-1.07312652027406,119.184398568056));
#56708=CARTESIAN_POINT('Ctrl Pts',(18.5018237176362,-1.11680179614521,119.203585076302));
#56709=CARTESIAN_POINT('Ctrl Pts',(18.8112727437243,-1.07312083019676,119.222781017226));
#56710=CARTESIAN_POINT('Ctrl Pts',(19.0966922989243,-0.945425429896232,
119.241986576724));
#56711=CARTESIAN_POINT('Ctrl Pts',(19.3357397025375,-0.743574694906012,
119.261203548649));
#56712=CARTESIAN_POINT('Ctrl Pts',(19.5096763702265,-0.483296157484075,
119.280432047793));
#56713=CARTESIAN_POINT('Ctrl Pts',(19.604829263032,-0.184805761734769,119.299674358162));
#56714=CARTESIAN_POINT('Ctrl Pts',(19.6136282032755,0.128548869667553,119.318929822438));
#56715=CARTESIAN_POINT('Ctrl Pts',(19.5483562428395,0.381754662526241,119.334989622353));
#56716=CARTESIAN_POINT('Ctrl Pts',(19.4555027014667,0.567586338753027,119.347844753828));
#56717=CARTESIAN_POINT('Ctrl Pts',(19.3083285466207,0.781707993580481,119.363921119013));
#56718=CARTESIAN_POINT('Ctrl Pts',(19.0213883195784,1.0173014385066,119.386447876364));
#56719=CARTESIAN_POINT('Ctrl Pts',(18.5601806816014,1.14326482672377,119.415452744608));
#56720=CARTESIAN_POINT('Ctrl Pts',(18.0870469004768,1.06976794361554,119.444502870166));
#56721=CARTESIAN_POINT('Ctrl Pts',(17.6845073765261,0.809000046868888,119.473601565479));
#56722=CARTESIAN_POINT('Ctrl Pts',(17.4231181242213,0.405838898540841,119.502752060927));
#56723=CARTESIAN_POINT('Ctrl Pts',(17.3490598832109,-0.0697983875198877,
119.531957712525));
#56724=CARTESIAN_POINT('Ctrl Pts',(17.4759534440631,-0.535171725229621,
119.561221496182));
#56725=CARTESIAN_POINT('Ctrl Pts',(17.7314548399343,-0.846550437506931,
119.58565944407));
#56726=CARTESIAN_POINT('Ctrl Pts',(17.999207559364,-1.0170868157945,119.605241751292));
#56727=CARTESIAN_POINT('Ctrl Pts',(18.2967905723551,-1.12863703662001,119.624846422395));
#56728=CARTESIAN_POINT('Ctrl Pts',(18.701022235534,-1.14581433888424,119.649394327387));
#56729=CARTESIAN_POINT('Ctrl Pts',(19.1533010528138,-0.965969567310355,
119.678922596865));
#56730=CARTESIAN_POINT('Ctrl Pts',(19.4935242230618,-0.616264784255005,
119.708524488639));
#56731=CARTESIAN_POINT('Ctrl Pts',(19.6616806751607,-0.15688731828813,119.738203011753));
#56732=CARTESIAN_POINT('Ctrl Pts',(19.6274500840142,0.332402173060607,119.767961008938));
#56733=CARTESIAN_POINT('Ctrl Pts',(19.3957290628344,0.766238455283539,119.797801335606));
#56734=CARTESIAN_POINT('Ctrl Pts',(19.0059018782433,1.06845895995986,119.827726746298));
#56735=CARTESIAN_POINT('Ctrl Pts',(18.5252515327408,1.18543071772727,119.857739979944));
#56736=CARTESIAN_POINT('Ctrl Pts',(18.037234743022,1.09564506473,119.887843657137));
#56737=CARTESIAN_POINT('Ctrl Pts',(17.6956019306827,0.860470084296629,119.913007640695));
#56738=CARTESIAN_POINT('Ctrl Pts',(17.4972936032911,0.600305772965447,119.93318661626));
#56739=CARTESIAN_POINT('Ctrl Pts',(17.3569038509229,0.304279815543778,119.953397785618));
#56740=CARTESIAN_POINT('Ctrl Pts',(17.3041660284991,-0.109796929925252,
119.978723169803));
#56741=CARTESIAN_POINT('Ctrl Pts',(17.4498994353956,-0.59078091166106,120.009214030095));
#56742=CARTESIAN_POINT('Ctrl Pts',(17.7804655429487,-0.971566966837065,
120.039807705564));
#56743=CARTESIAN_POINT('Ctrl Pts',(18.2393086861239,-1.18486584665598,120.07050641441));
#56744=CARTESIAN_POINT('Ctrl Pts',(18.7470163437987,-1.1921729938516,120.101312384752));
#56745=CARTESIAN_POINT('Ctrl Pts',(19.215087635489,-0.990765643040621,120.132227714623));
#56746=CARTESIAN_POINT('Ctrl Pts',(19.5613155231427,-0.614392148089554,
120.163254460057));
#56747=CARTESIAN_POINT('Ctrl Pts',(19.7242152497417,-0.127659401515012,
120.194394583265));
#56748=CARTESIAN_POINT('Ctrl Pts',(19.6739207775415,0.385049104109546,120.225649979257));
#56749=CARTESIAN_POINT('Ctrl Pts',(19.4176458057697,0.834175476321175,120.257022460356));
#56750=CARTESIAN_POINT('Ctrl Pts',(18.998699632526,1.14061462596676,120.288513762116));
#56751=CARTESIAN_POINT('Ctrl Pts',(18.4891879156563,1.24962833189955,120.320125537776));
#56752=CARTESIAN_POINT('Ctrl Pts',(17.9776202690671,1.14060959036587,120.351859359126));
#56753=CARTESIAN_POINT('Ctrl Pts',(17.5535525982464,0.830952823101709,120.383716714854));
#56754=CARTESIAN_POINT('Ctrl Pts',(17.2919248389954,0.373308289212946,120.415699010712));
#56755=CARTESIAN_POINT('Ctrl Pts',(17.2398314509524,-0.153353235375788,
120.447807567348));
#56756=CARTESIAN_POINT('Ctrl Pts',(17.4080575955601,-0.657352082285856,
120.480043619757));
#56757=CARTESIAN_POINT('Ctrl Pts',(17.7689006127485,-1.05024513051325,120.512408315922));
#56758=CARTESIAN_POINT('Ctrl Pts',(18.2607097297302,-1.26233444597482,120.544902716827));
#56759=CARTESIAN_POINT('Ctrl Pts',(18.7984052352737,-1.25502080659343,120.577527795704));
#56760=CARTESIAN_POINT('Ctrl Pts',(19.2881848794747,-1.0278144553583,120.610284437319));
#56761=CARTESIAN_POINT('Ctrl Pts',(19.6438781749597,-0.61873033468329,120.643173436616));
#56762=CARTESIAN_POINT('Ctrl Pts',(19.8020987090859,-0.0979461688159152,
120.676195498978));
#56763=CARTESIAN_POINT('Ctrl Pts',(19.7335320823132,0.444227716269205,120.709351239055));
#56764=CARTESIAN_POINT('Ctrl Pts',(19.4483480211883,0.912997875362089,120.742641182014));
#56765=CARTESIAN_POINT('Ctrl Pts',(18.9947430992497,1.22566304840365,120.776065760162));
#56766=CARTESIAN_POINT('Ctrl Pts',(18.4508057834443,1.32618611440986,120.809625317582));
#56767=CARTESIAN_POINT('Ctrl Pts',(17.9110852264692,1.19525527808251,120.843320100399));
#56768=CARTESIAN_POINT('Ctrl Pts',(17.4701505494149,0.853917314146234,120.877150274951));
#56769=CARTESIAN_POINT('Ctrl Pts',(17.2060388865232,0.360310149126953,120.911115893666));
#56770=CARTESIAN_POINT('Ctrl Pts',(17.1664153816519,-0.200398871563149,
120.945216959522));
#56771=CARTESIAN_POINT('Ctrl Pts',(17.3116264220795,-0.597882955951257,
120.970894211169));
#56772=CARTESIAN_POINT('Ctrl Pts',(17.4713230749973,-0.824292723162997,
120.988054644643));
#56773=CARTESIAN_POINT('Ctrl Pts',(17.5930295495418,-0.963403094471689,
120.999506127854));
#56774=CARTESIAN_POINT('Ctrl Pts',(17.8429222056168,-1.17180944522949,121.019575839724));
#56775=CARTESIAN_POINT('Ctrl Pts',(18.2831358555107,-1.3472696457857,121.048331046648));
#56776=CARTESIAN_POINT('Ctrl Pts',(18.8536622082132,-1.32345121615729,121.082971735828));
#56777=CARTESIAN_POINT('Ctrl Pts',(19.3666123501032,-1.06776818445665,121.11774633767));
#56778=CARTESIAN_POINT('Ctrl Pts',(19.7318189194698,-0.623135744515387,
121.152654299799));
#56779=CARTESIAN_POINT('Ctrl Pts',(19.8841229814082,-0.0660261383455702,
121.187694946127));
#56780=CARTESIAN_POINT('Ctrl Pts',(19.7952691811095,0.506861240356869,121.22286752838));
#56781=CARTESIAN_POINT('Ctrl Pts',(19.4789909654556,0.995298037449156,121.258171199464));
#56782=CARTESIAN_POINT('Ctrl Pts',(18.9889997447394,1.31312136899922,121.293605027892));
#56783=CARTESIAN_POINT('Ctrl Pts',(18.4098258930854,1.40341469896206,121.329167991327));
#56784=CARTESIAN_POINT('Ctrl Pts',(17.8422514541543,1.2487159173822,121.364858980876));
#56785=CARTESIAN_POINT('Ctrl Pts',(17.3857498366357,0.874358654879244,121.400676801254));
#56786=CARTESIAN_POINT('Ctrl Pts',(17.1210452069084,0.344343613450397,121.436620170121));
#56787=CARTESIAN_POINT('Ctrl Pts',(17.0958251015548,-0.249607404749667,
121.472687721701));
#56788=CARTESIAN_POINT('Ctrl Pts',(17.3161507636215,-0.803935931388206,
121.508878001574));
#56789=CARTESIAN_POINT('Ctrl Pts',(17.7451068582081,-1.22131693446959,121.545189480257));
#56790=CARTESIAN_POINT('Ctrl Pts',(18.3089795239874,-1.42776624833079,121.581620531396));
#56791=CARTESIAN_POINT('Ctrl Pts',(18.9099344796403,-1.38575758159487,121.618169476059));
#56792=CARTESIAN_POINT('Ctrl Pts',(19.443003408243,-1.10105588624391,121.654834501032));
#56793=CARTESIAN_POINT('Ctrl Pts',(19.814447080578,-0.621956720707161,121.691613814933));
#56794=CARTESIAN_POINT('Ctrl Pts',(19.9582412943487,-0.0311460741792062,
121.728505359742));
#56795=CARTESIAN_POINT('Ctrl Pts',(19.8478423707596,0.568675584892993,121.765507307081));
#56796=CARTESIAN_POINT('Ctrl Pts',(19.5010738542693,1.07254435780881,121.802617407826));
#56797=CARTESIAN_POINT('Ctrl Pts',(18.9772465487843,1.39174398963045,121.839833580231));
#56798=CARTESIAN_POINT('Ctrl Pts',(18.3670349923433,1.46935809393124,121.877153590267));
#56799=CARTESIAN_POINT('Ctrl Pts',(17.7767415245785,1.29047771303663,121.91457510912));
#56800=CARTESIAN_POINT('Ctrl Pts',(17.3097639110163,0.88502066898406,121.952095792454));
#56801=CARTESIAN_POINT('Ctrl Pts',(17.0484530789278,0.322744770605088,121.98971320241));
#56802=CARTESIAN_POINT('Ctrl Pts',(17.0395741793232,-0.29877511550778,122.027424807101));
#56803=CARTESIAN_POINT('Ctrl Pts',(17.2859276060077,-0.871100232399064,
122.065228088574));
#56804=CARTESIAN_POINT('Ctrl Pts',(17.7456411246251,-1.29387701195727,122.103120366714));
#56805=CARTESIAN_POINT('Ctrl Pts',(18.3392916665445,-1.49245955151488,122.141098983942));
#56806=CARTESIAN_POINT('Ctrl Pts',(18.9636467540723,-1.43110986029732,122.179161195417));
#56807=CARTESIAN_POINT('Ctrl Pts',(19.5096427527803,-1.11943132446743,122.217304158637));
#56808=CARTESIAN_POINT('Ctrl Pts',(19.8814701962045,-0.610888906864692,
122.255525076564));
#56809=CARTESIAN_POINT('Ctrl Pts',(20.0134084028596,0.00638374819795061,
122.293820960483));
#56810=CARTESIAN_POINT('Ctrl Pts',(19.8814680357448,0.624863883396621,122.332188933733));
#56811=CARTESIAN_POINT('Ctrl Pts',(19.5077372244298,1.13643840843378,122.370625859871));
#56812=CARTESIAN_POINT('Ctrl Pts',(18.9567207702999,1.45127557085421,122.409128868261));
#56813=CARTESIAN_POINT('Ctrl Pts',(18.3241217337611,1.51368240153528,122.447694658652));
#56814=CARTESIAN_POINT('Ctrl Pts',(17.7202826349282,1.31196813537611,122.486320211507));
#56815=CARTESIAN_POINT('Ctrl Pts',(17.2508103246174,0.880536550537675,122.525002285958));
#56816=CARTESIAN_POINT('Ctrl Pts',(16.9981604164449,0.294249197224712,122.563737660687));
#56817=CARTESIAN_POINT('Ctrl Pts',(17.0060423714049,-0.274042958784632,
122.598213625129));
#56818=CARTESIAN_POINT('Ctrl Pts',(17.1818706810392,-0.73303144472968,122.628410343682));
#56819=CARTESIAN_POINT('Ctrl Pts',(17.5191721715142,-1.18310393837461,122.662947355674));
#56820=CARTESIAN_POINT('Ctrl Pts',(18.1531350042187,-1.53390972067408,122.706165522702));
#56821=CARTESIAN_POINT('Ctrl Pts',(19.0227874461394,-1.48519217492529,122.758094642985));
#56822=CARTESIAN_POINT('Ctrl Pts',(19.7338192740336,-0.980774656373063,
122.810082875595));
#56823=CARTESIAN_POINT('Ctrl Pts',(20.067922277282,-0.174626022127283,122.862122158172));
#56824=CARTESIAN_POINT('Ctrl Pts',(19.921708544036,0.68662933685667,122.914204231648));
#56825=CARTESIAN_POINT('Ctrl Pts',(19.4364076102001,1.22943043838242,122.957634782588));
#56826=CARTESIAN_POINT('Ctrl Pts',(18.9192757117743,1.45961435937841,122.992392354061));
#56827=CARTESIAN_POINT('Ctrl Pts',(18.5146998498917,1.51727349960696,123.017500336371));
#56828=CARTESIAN_POINT('Ctrl Pts',(18.1254479581993,1.46800683442712,123.041646590114));
#56829=CARTESIAN_POINT('Ctrl Pts',(17.65765089863,1.28524666288511,123.072557499479));
#56830=CARTESIAN_POINT('Ctrl Pts',(17.1864413110902,0.84817385210292,123.111201426539));
#56831=CARTESIAN_POINT('Ctrl Pts',(16.9818560590682,0.238917012125818,123.149847159061));
#56832=CARTESIAN_POINT('Ctrl Pts',(17.0077477842283,-0.262729802221198,
123.180762273051));
#56833=CARTESIAN_POINT('Ctrl Pts',(17.1549558342261,-0.742832495303323,
123.211674984775));
#56834=CARTESIAN_POINT('Ctrl Pts',(17.5555345576308,-1.24539323375308,123.250310351106));
#56835=CARTESIAN_POINT('Ctrl Pts',(18.2066766855254,-1.51951236558385,123.292795159863));
#56836=CARTESIAN_POINT('Ctrl Pts',(18.8397001520098,-1.49532848220801,123.331402485356));
#56837=CARTESIAN_POINT('Ctrl Pts',(19.361933038917,-1.2676766648096,123.36613474992));
#56838=CARTESIAN_POINT('Ctrl Pts',(19.7646594303858,-0.864798752237798,
123.400850262946));
#56839=CARTESIAN_POINT('Ctrl Pts',(19.992247479715,-0.343129638214644,123.435546682762));
#56840=CARTESIAN_POINT('Ctrl Pts',(20.0134975784261,0.225403110709894,123.470221342828));
#56841=CARTESIAN_POINT('Ctrl Pts',(19.8256820027275,0.761912608646907,123.504872214536));
#56842=CARTESIAN_POINT('Ctrl Pts',(19.516918297423,1.12076930887003,123.533725575818));
#56843=CARTESIAN_POINT('Ctrl Pts',(19.2041810039955,1.32499554631978,123.556794181975));
#56844=CARTESIAN_POINT('Ctrl Pts',(18.8020588760868,1.49233095074489,123.583695662073));
#56845=CARTESIAN_POINT('Ctrl Pts',(18.1960164011262,1.52254678614699,123.620174599657));
#56846=CARTESIAN_POINT('Ctrl Pts',(17.6216673694243,1.24564088295246,123.658522649907));
#56847=CARTESIAN_POINT('Ctrl Pts',(17.2833151529131,0.880111521286915,123.689167672577));
#56848=CARTESIAN_POINT('Ctrl Pts',(17.1050831264071,0.552606139546885,123.712134313292));
#56849=CARTESIAN_POINT('Ctrl Pts',(16.9816547923198,0.0706959663075114,
123.742732173804));
#56850=CARTESIAN_POINT('Ctrl Pts',(17.0529092044043,-0.496279877167484,
123.777112906262));
#56851=CARTESIAN_POINT('Ctrl Pts',(17.3864957981709,-1.02604026133052,123.815255128178));
#56852=CARTESIAN_POINT('Ctrl Pts',(17.857593613417,-1.37397111071324,123.850964243175));
#56853=CARTESIAN_POINT('Ctrl Pts',(18.4515962038669,-1.51829287387834,123.888044644597));
#56854=CARTESIAN_POINT('Ctrl Pts',(19.0746522170704,-1.40326627781162,123.926485479005));
#56855=CARTESIAN_POINT('Ctrl Pts',(19.5520449521414,-1.07433327180886,123.961659739466));
#56856=CARTESIAN_POINT('Ctrl Pts',(19.7870135179904,-0.729922634281818,
123.987199138138));
#56857=CARTESIAN_POINT('Ctrl Pts',(19.9172825726675,-0.412389600249223,
124.008461419526));
#56858=CARTESIAN_POINT('Ctrl Pts',(19.9813821346012,-0.0901260863987032,
124.028642265937));
#56859=CARTESIAN_POINT('Ctrl Pts',(19.9464919895927,0.322871316840072,124.054100150558));
#56860=CARTESIAN_POINT('Ctrl Pts',(19.7988560610193,0.709540527634926,124.079522689038));
#56861=CARTESIAN_POINT('Ctrl Pts',(19.5502809158787,1.03976970882056,124.104909666808));
#56862=CARTESIAN_POINT('Ctrl Pts',(19.2205019215012,1.28789198571529,124.130259814538));
#56863=CARTESIAN_POINT('Ctrl Pts',(18.8675304954949,1.42261786918923,124.153463104108));
#56864=CARTESIAN_POINT('Ctrl Pts',(18.5284830739033,1.46304402439271,124.174529127565));
#56865=CARTESIAN_POINT('Ctrl Pts',(18.1207874834896,1.4260614944801,124.199779233887));
#56866=CARTESIAN_POINT('Ctrl Pts',(17.6438940253866,1.2206283929953,124.231286143554));
#56867=CARTESIAN_POINT('Ctrl Pts',(17.2233006573008,0.762755887841534,124.269003086711));
#56868=CARTESIAN_POINT('Ctrl Pts',(17.0268753162689,0.174604680404742,124.306625880741));
#56869=CARTESIAN_POINT('Ctrl Pts',(17.0876702801681,-0.440949978759675,
124.344152137287));
#56870=CARTESIAN_POINT('Ctrl Pts',(17.3937696919832,-0.976537539345891,
124.381579352596));
#56871=CARTESIAN_POINT('Ctrl Pts',(17.8905867113653,-1.33941486357803,124.41890518565));
#56872=CARTESIAN_POINT('Ctrl Pts',(18.4906153716989,-1.46735186134762,124.456127313473));
#56873=CARTESIAN_POINT('Ctrl Pts',(19.0888593629504,-1.33941777641846,124.493243511411));
#56874=CARTESIAN_POINT('Ctrl Pts',(19.5812312587733,-0.97933823951139,124.530251612046));
#56875=CARTESIAN_POINT('Ctrl Pts',(19.8826841702414,-0.45113379238791,124.567149528264));
#56876=CARTESIAN_POINT('Ctrl Pts',(19.9419184246875,0.15228968271957,124.603935243626));
#56877=CARTESIAN_POINT('Ctrl Pts',(19.7501149544944,0.72549274055214,124.640606820178));
#56878=CARTESIAN_POINT('Ctrl Pts',(19.3422099788232,1.16895227798287,124.677162396834));
#56879=CARTESIAN_POINT('Ctrl Pts',(18.7905344628525,1.4063573661534,124.713600191806));
#56880=CARTESIAN_POINT('Ctrl Pts',(18.1919768114847,1.39775285517752,124.749918502117));
#56881=CARTESIAN_POINT('Ctrl Pts',(17.650949463827,1.14625964667207,124.786115706138));
#56882=CARTESIAN_POINT('Ctrl Pts',(17.2611574231578,0.697245715919318,124.822190264427));
#56883=CARTESIAN_POINT('Ctrl Pts',(17.0893550841156,0.130141700592976,124.858140721292));
#56884=CARTESIAN_POINT('Ctrl Pts',(17.1639091103876,-0.45562104348777,124.893965705161));
#56885=CARTESIAN_POINT('Ctrl Pts',(17.4701273616986,-0.958058662722596,
124.929663929076));
#56886=CARTESIAN_POINT('Ctrl Pts',(17.9531200725725,-1.29040433417455,124.965234192037));
#56887=CARTESIAN_POINT('Ctrl Pts',(18.5276405431088,-1.39610073357796,125.000675380104));
#56888=CARTESIAN_POINT('Ctrl Pts',(19.0931401580165,-1.25842381920182,125.035986467183));
#56889=CARTESIAN_POINT('Ctrl Pts',(19.5513770476802,-0.903101174061878,
125.071166515444));
#56890=CARTESIAN_POINT('Ctrl Pts',(19.8234925261704,-0.393520928653388,
125.106214675531));
#56891=CARTESIAN_POINT('Ctrl Pts',(19.863585446952,0.18057846519377,125.141130187601));
#56892=CARTESIAN_POINT('Ctrl Pts',(19.6664477552688,0.718918428921209,125.175912381995));
#56893=CARTESIAN_POINT('Ctrl Pts',(19.2681597354425,1.12820343239091,125.210560679702));
#56894=CARTESIAN_POINT('Ctrl Pts',(18.7394968083553,1.33829386724977,125.245074592494));
#56895=CARTESIAN_POINT('Ctrl Pts',(18.1733515600056,1.31422440666254,125.279453723019));
#56896=CARTESIAN_POINT('Ctrl Pts',(17.6684072336029,1.06200918227394,125.313697765461));
#56897=CARTESIAN_POINT('Ctrl Pts',(17.3119333434095,0.62727345561428,125.347806505814));
#56898=CARTESIAN_POINT('Ctrl Pts',(17.164703194465,0.0870075502303987,125.381779821996));
#56899=CARTESIAN_POINT('Ctrl Pts',(17.2506394082675,-0.464067284867245,
125.415617683646));
#56900=CARTESIAN_POINT('Ctrl Pts',(17.5529500312885,-0.93010635281992,125.449320152153));
#56901=CARTESIAN_POINT('Ctrl Pts',(18.0173742562096,-1.23080998259887,125.482887380882));
#56902=CARTESIAN_POINT('Ctrl Pts',(18.5619148970354,-1.31525442806852,125.516319615136));
#56903=CARTESIAN_POINT('Ctrl Pts',(19.0913123481237,-1.17050448618906,125.54961719185));
#56904=CARTESIAN_POINT('Ctrl Pts',(19.5137054329361,-0.823554001177106,
125.582780539051));
#56905=CARTESIAN_POINT('Ctrl Pts',(19.7565657136191,-0.336311890299757,
125.615810175785));
#56906=CARTESIAN_POINT('Ctrl Pts',(19.7791421686803,0.205437475860851,125.64870671201));
#56907=CARTESIAN_POINT('Ctrl Pts',(19.5792831503527,0.707131271594729,125.681470848156));
#56908=CARTESIAN_POINT('Ctrl Pts',(19.1934974783569,1.08192650056308,125.714103374504));
#56909=CARTESIAN_POINT('Ctrl Pts',(18.6903000531182,1.26572269937722,125.74660517022));
#56910=CARTESIAN_POINT('Ctrl Pts',(18.1580528586921,1.22811231780654,125.778977203127));
#56911=CARTESIAN_POINT('Ctrl Pts',(17.6894582924859,0.977390643756032,125.811220529498));
#56912=CARTESIAN_POINT('Ctrl Pts',(17.3654249182296,0.55880467658169,125.843336292948));
#56913=CARTESIAN_POINT('Ctrl Pts',(17.2411113552341,0.0464007134562138,
125.875325723779));
#56914=CARTESIAN_POINT('Ctrl Pts',(17.3365525714722,-0.470062155704644,
125.907190137343));
#56915=CARTESIAN_POINT('Ctrl Pts',(17.6334582774054,-0.900821679431447,
125.938930933878));
#56916=CARTESIAN_POINT('Ctrl Pts',(18.078689306533,-1.17169762162142,125.970549597961));
#56917=CARTESIAN_POINT('Ctrl Pts',(18.593754716555,-1.23684923441498,126.002047697117));
#56918=CARTESIAN_POINT('Ctrl Pts',(19.0886338471913,-1.0865147767173,126.033426880753));
#56919=CARTESIAN_POINT('Ctrl Pts',(19.4774918201155,-0.748430497103195,
126.064688878174));
#56920=CARTESIAN_POINT('Ctrl Pts',(19.6935481589647,-0.282732209663939,
126.095835498253));
#56921=CARTESIAN_POINT('Ctrl Pts',(19.7005261381603,0.228725868558277,126.126868628752));
#56922=CARTESIAN_POINT('Ctrl Pts',(19.4987238371462,0.696739517761545,126.157790234506));
#56923=CARTESIAN_POINT('Ctrl Pts',(19.1246955649095,1.04029099805458,126.188602356125));
#56924=CARTESIAN_POINT('Ctrl Pts',(18.6446468213007,1.20055180571536,126.219307107577));
#56925=CARTESIAN_POINT('Ctrl Pts',(18.1427337757278,1.15093580581614,126.24990667576));
#56926=CARTESIAN_POINT('Ctrl Pts',(17.7063324713574,0.901488522300449,126.280403319565));
#56927=CARTESIAN_POINT('Ctrl Pts',(17.4108529526162,0.496892712939118,126.310799367952));
#56928=CARTESIAN_POINT('Ctrl Pts',(17.3067328954843,0.0084812245335301,
126.34109721811));
#56929=CARTESIAN_POINT('Ctrl Pts',(17.4108490145204,-0.47831756693869,126.371299332964));
#56930=CARTESIAN_POINT('Ctrl Pts',(17.7038045321021,-0.878895943230857,
126.401408240409));
#56931=CARTESIAN_POINT('Ctrl Pts',(18.1335240920449,-1.12414442958507,126.431426532286));
#56932=CARTESIAN_POINT('Ctrl Pts',(18.6244919535479,-1.17234924842773,126.461356862258));
#56933=CARTESIAN_POINT('Ctrl Pts',(19.0909970917821,-1.01626672882518,126.491201943604));
#56934=CARTESIAN_POINT('Ctrl Pts',(19.4520665620905,-0.684179402726174,
126.520964546554));
#56935=CARTESIAN_POINT('Ctrl Pts',(19.6454906893739,-0.234786668051046,
126.550647497157));
#56936=CARTESIAN_POINT('Ctrl Pts',(19.6385159835268,0.253149219888882,126.580253676135));
#56937=CARTESIAN_POINT('Ctrl Pts',(19.4333722711128,0.694578566817253,126.609786017081));
#56938=CARTESIAN_POINT('Ctrl Pts',(19.0667063558325,1.01295613554844,126.639247502871));
#56939=CARTESIAN_POINT('Ctrl Pts',(18.6030514946211,1.1534838541102,126.668641164986));
#56940=CARTESIAN_POINT('Ctrl Pts',(18.1234957510667,1.09251755167767,126.697970077986));
#56941=CARTESIAN_POINT('Ctrl Pts',(17.7115308462464,0.841530068193854,126.727237365886));
#56942=CARTESIAN_POINT('Ctrl Pts',(17.4385535098235,0.444964463531077,126.756446186453));
#56943=CARTESIAN_POINT('Ctrl Pts',(17.3515170588706,-0.0276122872710075,
126.785599752877));
#56944=CARTESIAN_POINT('Ctrl Pts',(17.4648884689082,-0.493692017961726,
126.814701285522));
#56945=CARTESIAN_POINT('Ctrl Pts',(17.7582364067503,-0.872180645238306,
126.843754094616));
#56946=CARTESIAN_POINT('Ctrl Pts',(18.1799399597792,-1.09750112430032,126.872761421116));
#56947=CARTESIAN_POINT('Ctrl Pts',(18.6561791423461,-1.13087232076486,126.901726730967));
#56948=CARTESIAN_POINT('Ctrl Pts',(19.1039589342991,-0.967064360638307,
126.930653153623));
#56949=CARTESIAN_POINT('Ctrl Pts',(19.3883902256841,-0.690354148280827,
126.954729317772));
#56950=CARTESIAN_POINT('Ctrl Pts',(19.5332457227074,-0.414056911611768,
126.973973920849));
#56951=CARTESIAN_POINT('Ctrl Pts',(19.6177437769726,-0.113905111418309,
126.993208932229));
#56952=CARTESIAN_POINT('Ctrl Pts',(19.6011038359952,0.281732384417546,127.017234385341));
#56953=CARTESIAN_POINT('Ctrl Pts',(19.3890514321733,0.706565085330299,127.04604027079));
#56954=CARTESIAN_POINT('Ctrl Pts',(19.0223011451343,1.00751421476368,127.074824428941));
#56955=CARTESIAN_POINT('Ctrl Pts',(18.5648792017946,1.13234542273552,127.103590628698));
#56956=CARTESIAN_POINT('Ctrl Pts',(18.0966155583551,1.05950100369092,127.13234222422));
#56957=CARTESIAN_POINT('Ctrl Pts',(17.6990872091144,0.801854248777839,127.161082806753));
#56958=CARTESIAN_POINT('Ctrl Pts',(17.4415305074347,0.404417889894389,127.18981585486));
#56959=CARTESIAN_POINT('Ctrl Pts',(17.3687695530042,-0.0634870235218906,
127.218544916761));
#56960=CARTESIAN_POINT('Ctrl Pts',(17.4934609062107,-0.520295799873725,
127.247273508358));
#56961=CARTESIAN_POINT('Ctrl Pts',(17.7938846953223,-0.886376575644098,
127.276005163098));
#56962=CARTESIAN_POINT('Ctrl Pts',(18.2177247634987,-1.0978765550393,127.304743403475));
#56963=CARTESIAN_POINT('Ctrl Pts',(18.6911508939668,-1.11782834790528,127.333491753923));
#56964=CARTESIAN_POINT('Ctrl Pts',(19.1316465689169,-0.942594483611371,
127.362253727978));
#56965=CARTESIAN_POINT('Ctrl Pts',(19.4623516371648,-0.602527764442204,
127.391032833955));
#56966=CARTESIAN_POINT('Ctrl Pts',(19.6254375334004,-0.156728820867022,
127.419832557726));
#56967=CARTESIAN_POINT('Ctrl Pts',(19.5921943171502,0.317197263638082,127.448656399276));
#56968=CARTESIAN_POINT('Ctrl Pts',(19.368068361135,0.736614311055538,127.477507771776));
#56969=CARTESIAN_POINT('Ctrl Pts',(18.9917822982762,1.02822677014049,127.506390229474));
#56970=CARTESIAN_POINT('Ctrl Pts',(18.5286553795516,1.1408523543525,127.535306988223));
#56971=CARTESIAN_POINT('Ctrl Pts',(18.0593071007243,1.05438854513454,127.564261845145));
#56972=CARTESIAN_POINT('Ctrl Pts',(17.665645179454,0.78337931240486,127.593257348673));
#56973=CARTESIAN_POINT('Ctrl Pts',(17.4166255106301,0.374596672588247,127.622298651964));
#56974=CARTESIAN_POINT('Ctrl Pts',(17.356168808789,-0.10102697056375,127.651385319048));
#56975=CARTESIAN_POINT('Ctrl Pts',(17.4955452283241,-0.560666528004949,
127.680527574784));
#56976=CARTESIAN_POINT('Ctrl Pts',(17.8109503297906,-0.923997881438208,
127.709717292561));
#56977=CARTESIAN_POINT('Ctrl Pts',(18.2483725221223,-1.12713601481138,127.738975362331));
#56978=CARTESIAN_POINT('Ctrl Pts',(18.7311725427411,-1.13411043401417,127.768275574607));
#56979=CARTESIAN_POINT('Ctrl Pts',(19.1762783013378,-0.942422457862223,
127.797675015527));
#56980=CARTESIAN_POINT('Ctrl Pts',(19.5046484170361,-0.585761601815651,
127.827081897376));
#56981=CARTESIAN_POINT('Ctrl Pts',(19.6582495271737,-0.123680562238502,
127.85662756148));
#56982=CARTESIAN_POINT('Ctrl Pts',(19.6201095104048,0.280620801278878,127.881304584504));
#56983=CARTESIAN_POINT('Ctrl Pts',(19.4907597078714,0.572725205601487,127.900977353949));
#56984=CARTESIAN_POINT('Ctrl Pts',(19.3483928135265,0.768967247407983,127.915853796736));
#56985=CARTESIAN_POINT('Ctrl Pts',(19.1686762334047,0.931517072832566,127.930784609013));
#56986=CARTESIAN_POINT('Ctrl Pts',(18.9634686971736,1.051701521621,127.945656286825));
#56987=CARTESIAN_POINT('Ctrl Pts',(18.7934282466761,1.10758167118611,127.956894169607));
#56988=CARTESIAN_POINT('Ctrl Pts',(18.692507014378,1.12612980783387,127.963248051465));
#56989=CARTESIAN_POINT('Ctrl Pts',(18.6702756913488,1.12955277882793,127.964633433995));
#56990=CARTESIAN_POINT('',(0.,0.,0.));
#56991=CARTESIAN_POINT('Origin',(0.,0.,-0.785));
#56992=CARTESIAN_POINT('',(-0.492894796571446,0.000311056548144339,-1.57911584740964));
#56993=CARTESIAN_POINT('',(-0.492681024549354,0.000145720506528142,-1.60088415259036));
#56994=CARTESIAN_POINT('',(-0.4925,-6.03138548580071E-17,-0.785));
#56995=CARTESIAN_POINT('',(0.217165055346613,0.442373225884384,-1.6275));
#56996=CARTESIAN_POINT('Ctrl Pts',(-0.492894796571446,0.000311056548144339,
-1.57911584740964));
#56997=CARTESIAN_POINT('Ctrl Pts',(-0.493072781975635,0.0225970133474953,
-1.58019890716347));
#56998=CARTESIAN_POINT('Ctrl Pts',(-0.49169270506612,0.0448619688323287,
-1.58128196691731));
#56999=CARTESIAN_POINT('Ctrl Pts',(-0.48867934824822,0.0669043084087307,
-1.58236502667114));
#57000=CARTESIAN_POINT('Ctrl Pts',(-0.46677608813157,0.227123999105002,
-1.5902374894904));
#57001=CARTESIAN_POINT('Ctrl Pts',(-0.358579539374524,0.375581922119211,
-1.59810995230966));
#57002=CARTESIAN_POINT('Ctrl Pts',(-0.212592472031373,0.445197883180087,
-1.60598241512892));
#57003=CARTESIAN_POINT('Ctrl Pts',(-0.0795850009787494,0.508624343442078,
-1.61315494341928));
#57004=CARTESIAN_POINT('Ctrl Pts',(0.0847918659550201,0.50660516259901,
-1.62032747170964));
#57005=CARTESIAN_POINT('Ctrl Pts',(0.217490523462166,0.442550970777087,
-1.6275));
#57006=CARTESIAN_POINT('',(-0.21683958723106,0.44219548099168,-1.6275));
#57007=CARTESIAN_POINT('Origin',(0.,0.,-1.6275));
#57008=CARTESIAN_POINT('Ctrl Pts',(-0.216839587231058,0.442195480991681,
-1.6275));
#57009=CARTESIAN_POINT('Ctrl Pts',(-0.289748988500098,0.406442866693165,
-1.62356376859037));
#57010=CARTESIAN_POINT('Ctrl Pts',(-0.353117841415619,0.352318189275016,
-1.61962753718074));
#57011=CARTESIAN_POINT('Ctrl Pts',(-0.400486606282593,0.286264167711519,
-1.61569130577111));
#57012=CARTESIAN_POINT('Ctrl Pts',(-0.447855371149569,0.220210146148021,
-1.61175507436148));
#57013=CARTESIAN_POINT('Ctrl Pts',(-0.479224047967998,0.142226780439174,
-1.60781884295185));
#57014=CARTESIAN_POINT('Ctrl Pts',(-0.489180114775594,0.0617636412371016,
-1.60388261154222));
#57015=CARTESIAN_POINT('Ctrl Pts',(-0.491708155307928,0.0413324728658215,
-1.60288312522493));
#57016=CARTESIAN_POINT('Ctrl Pts',(-0.49285561428007,0.0207414206897894,
-1.60188363890765));
#57017=CARTESIAN_POINT('Ctrl Pts',(-0.492681024549354,0.000145720506528142,
-1.60088415259036));
#57018=CARTESIAN_POINT('Origin',(0.,0.,-0.785));
#57019=CARTESIAN_POINT('',(-0.491724062797573,2.84481552980109E-5,-1.42911584740964));
#57020=CARTESIAN_POINT('',(-0.491725215890323,5.26094410910955E-5,-1.45088415259036));
#57021=CARTESIAN_POINT('',(-0.4925,-6.03138548580071E-17,-0.785));
#57022=CARTESIAN_POINT('Ctrl Pts',(-0.491724062797573,2.84481552980109E-5,
-1.42911584740964));
#57023=CARTESIAN_POINT('Ctrl Pts',(-0.491766038698159,0.0797124417823624,
-1.43296413024792));
#57024=CARTESIAN_POINT('Ctrl Pts',(-0.473465280791214,0.159378202380034,
-1.43681241308619));
#57025=CARTESIAN_POINT('Ctrl Pts',(-0.43671528821848,0.229354820363482,
-1.44066069592447));
#57026=CARTESIAN_POINT('Ctrl Pts',(-0.361535536028939,0.372506544507255,
-1.44853315874373));
#57027=CARTESIAN_POINT('Ctrl Pts',(-0.209147193490587,0.475109971852566,
-1.45640562156299));
#57028=CARTESIAN_POINT('Ctrl Pts',(-0.048228220013445,0.490917381779544,
-1.46427808438225));
#57029=CARTESIAN_POINT('Ctrl Pts',(0.112690753463697,0.506724791706522,
-1.47215054720151));
#57030=CARTESIAN_POINT('Ctrl Pts',(0.282140357879629,0.435736184215168,
-1.48002301002077));
#57031=CARTESIAN_POINT('Ctrl Pts',(0.383738024817693,0.309953148400658,
-1.48789547284003));
#57032=CARTESIAN_POINT('Ctrl Pts',(0.485335691755757,0.184170112586147,
-1.49576793565929));
#57033=CARTESIAN_POINT('Ctrl Pts',(0.519081421215954,0.00359264844848062,
-1.50364039847855));
#57034=CARTESIAN_POINT('Ctrl Pts',(0.469784530510368,-0.150403090698195,
-1.51151286129781));
#57035=CARTESIAN_POINT('Ctrl Pts',(0.420487639804781,-0.304398829844871,
-1.51938532411706));
#57036=CARTESIAN_POINT('Ctrl Pts',(0.288148128933412,-0.431812844000556,
-1.52725778693632));
#57037=CARTESIAN_POINT('Ctrl Pts',(0.132376511934491,-0.475195091226392,
-1.53513024975558));
#57038=CARTESIAN_POINT('Ctrl Pts',(-0.0233951050644308,-0.518577338452229,
-1.54300271257484));
#57039=CARTESIAN_POINT('Ctrl Pts',(-0.202598828190905,-0.477927818748217,
-1.5508751753941));
#57040=CARTESIAN_POINT('Ctrl Pts',(-0.324395704016015,-0.371612329707044,
-1.55874763821336));
#57041=CARTESIAN_POINT('Ctrl Pts',(-0.429436286749963,-0.27992327079748,
-1.56553704127879));
#57042=CARTESIAN_POINT('Ctrl Pts',(-0.491779055131949,-0.139393463792468,
-1.57232644434422));
#57043=CARTESIAN_POINT('Ctrl Pts',(-0.492894796571446,0.000311056548144339,
-1.57911584740964));
#57044=CARTESIAN_POINT('Ctrl Pts',(-0.492681024549354,0.000145720506528142,
-1.60088415259036));
#57045=CARTESIAN_POINT('Ctrl Pts',(-0.491480456721719,-0.141480793986821,
-1.59401117608839));
#57046=CARTESIAN_POINT('Ctrl Pts',(-0.427764999610373,-0.283327095887921,
-1.58713819958642));
#57047=CARTESIAN_POINT('Ctrl Pts',(-0.320567499630029,-0.374915910947789,
-1.58026522308444));
#57048=CARTESIAN_POINT('Ctrl Pts',(-0.197781057297411,-0.479823812351491,
-1.57239276026518));
#57049=CARTESIAN_POINT('Ctrl Pts',(-0.0179464790603139,-0.51879424278185,
-1.56452029744593));
#57050=CARTESIAN_POINT('Ctrl Pts',(0.137413483204638,-0.473829273326357,
-1.55664783462667));
#57051=CARTESIAN_POINT('Ctrl Pts',(0.29277344546959,-0.428864303870864,
-1.54877537180741));
#57052=CARTESIAN_POINT('Ctrl Pts',(0.423658791762397,-0.299963934529519,
-1.54090290898815));
#57053=CARTESIAN_POINT('Ctrl Pts',(0.471309471097307,-0.145433967873361,
-1.53303044616889));
#57054=CARTESIAN_POINT('Ctrl Pts',(0.518960150432216,0.00909599878279682,
-1.52515798334963));
#57055=CARTESIAN_POINT('Ctrl Pts',(0.483376162809228,0.189255562753767,
-1.51728552053037));
#57056=CARTESIAN_POINT('Ctrl Pts',(0.380476665429358,0.313951811038567,
-1.50941305771111));
#57057=CARTESIAN_POINT('Ctrl Pts',(0.277577168049488,0.438648059323367,
-1.50154059489185));
#57058=CARTESIAN_POINT('Ctrl Pts',(0.107362160912737,0.507880991921996,
-1.49366813207259));
#57059=CARTESIAN_POINT('Ctrl Pts',(-0.0533889325663778,0.490391165225274,
-1.48579566925333));
#57060=CARTESIAN_POINT('Ctrl Pts',(-0.214140026045492,0.472901338528552,
-1.47792320643407));
#57061=CARTESIAN_POINT('Ctrl Pts',(-0.365427205866971,0.368688752536479,
-1.47005074361481));
#57062=CARTESIAN_POINT('Ctrl Pts',(-0.439095781953566,0.224751935185655,
-1.46217828079555));
#57063=CARTESIAN_POINT('Ctrl Pts',(-0.474325009118265,0.155919563159685,
-1.45841357139382));
#57064=CARTESIAN_POINT('Ctrl Pts',(-0.491803862332235,0.0780027715797182,
-1.45464886199209));
#57065=CARTESIAN_POINT('Ctrl Pts',(-0.491725215890323,5.26094410910955E-5,
-1.45088415259036));
#57066=CARTESIAN_POINT('Origin',(0.,0.,-0.785));
#57067=CARTESIAN_POINT('',(-0.492844994071537,-0.000375497391989388,-1.27911584740964));
#57068=CARTESIAN_POINT('',(-0.492796742099722,-0.000388985907888563,-1.30088415259036));
#57069=CARTESIAN_POINT('',(-0.4925,-6.03138548580071E-17,-0.785));
#57070=CARTESIAN_POINT('Ctrl Pts',(-0.492844994071537,-0.000375497391989388,
-1.27911584740964));
#57071=CARTESIAN_POINT('Ctrl Pts',(-0.49169234062138,0.135775279584172,
-1.28572935333236));
#57072=CARTESIAN_POINT('Ctrl Pts',(-0.432845290990704,0.272801628077903,
-1.29234285925508));
#57073=CARTESIAN_POINT('Ctrl Pts',(-0.33250996431107,0.364365032885267,
-1.2989563651778));
#57074=CARTESIAN_POINT('Ctrl Pts',(-0.213074654511156,0.473358584622236,
-1.30682882799706));
#57075=CARTESIAN_POINT('Ctrl Pts',(-0.0348520950583099,0.517932941093665,
-1.31470129081632));
#57076=CARTESIAN_POINT('Ctrl Pts',(0.121830995151941,0.477997897412073,
-1.32257375363558));
#57077=CARTESIAN_POINT('Ctrl Pts',(0.278514085362191,0.438062853730481,
-1.33044621645484));
#57078=CARTESIAN_POINT('Ctrl Pts',(0.413657706329846,0.313618409895869,
-1.3383186792741));
#57079=CARTESIAN_POINT('Ctrl Pts',(0.466350984614939,0.160753135356507,
-1.34619114209336));
#57080=CARTESIAN_POINT('Ctrl Pts',(0.519044262900032,0.00788786081714538,
-1.35406360491262));
#57081=CARTESIAN_POINT('Ctrl Pts',(0.489287198502561,-0.173398244426965,
-1.36193606773188));
#57082=CARTESIAN_POINT('Ctrl Pts',(0.390491992071155,-0.301397825554306,
-1.36980853055114));
#57083=CARTESIAN_POINT('Ctrl Pts',(0.291696785639748,-0.429397406681647,
-1.3776809933704));
#57084=CARTESIAN_POINT('Ctrl Pts',(0.123863437174404,-0.504110463692217,
-1.38555345618966));
#57085=CARTESIAN_POINT('Ctrl Pts',(-0.0373644791913577,-0.491862563024499,
-1.39342591900891));
#57086=CARTESIAN_POINT('Ctrl Pts',(-0.198592395557119,-0.479614662356781,
-1.40129838182817));
#57087=CARTESIAN_POINT('Ctrl Pts',(-0.353214879823299,-0.380405804010775,
-1.40917084464743));
#57088=CARTESIAN_POINT('Ctrl Pts',(-0.431540541036024,-0.238951364366653,
-1.41704330746669));
#57089=CARTESIAN_POINT('Ctrl Pts',(-0.471578400227735,-0.166643861961637,
-1.42106748744768));
#57090=CARTESIAN_POINT('Ctrl Pts',(-0.49168016826437,-0.0832977379475879,
-1.42509166742866));
#57091=CARTESIAN_POINT('Ctrl Pts',(-0.491724062797573,2.84481552980109E-5,
-1.42911584740964));
#57092=CARTESIAN_POINT('Ctrl Pts',(-0.491725215890323,5.26094410910955E-5,
-1.45088415259036));
#57093=CARTESIAN_POINT('Ctrl Pts',(-0.491639403107431,-0.0850004479807165,
-1.44677639917283));
#57094=CARTESIAN_POINT('Ctrl Pts',(-0.470650596961721,-0.170093234554161,
-1.4426686457553));
#57095=CARTESIAN_POINT('Ctrl Pts',(-0.429009346683205,-0.24346817854896,
-1.43856089233777));
#57096=CARTESIAN_POINT('Ctrl Pts',(-0.349204362974535,-0.384090426223178,
-1.43068842951851));
#57097=CARTESIAN_POINT('Ctrl Pts',(-0.19354442320548,-0.481673872862038,
-1.42281596669926));
#57098=CARTESIAN_POINT('Ctrl Pts',(-0.0321958015858799,-0.492228826589368,
-1.41494350388));
#57099=CARTESIAN_POINT('Ctrl Pts',(0.12915282003372,-0.502783780316697,
-1.40707104106074));
#57100=CARTESIAN_POINT('Ctrl Pts',(0.296190123503867,-0.426310241132496,
-1.39919857824148));
#57101=CARTESIAN_POINT('Ctrl Pts',(0.393635112256126,-0.297279702079536,
-1.39132611542222));
#57102=CARTESIAN_POINT('Ctrl Pts',(0.491080101008387,-0.168249163026577,
-1.38345365260296));
#57103=CARTESIAN_POINT('Ctrl Pts',(0.51893277504276,0.0133383758951397,
-1.3755811897837));
#57104=CARTESIAN_POINT('Ctrl Pts',(0.464637291129985,0.165641568032344,
-1.36770872696444));
#57105=CARTESIAN_POINT('Ctrl Pts',(0.41034180721721,0.317944760169548,-1.35983626414518));
#57106=CARTESIAN_POINT('Ctrl Pts',(0.273898165357287,0.440963605522239,
-1.35196380132592));
#57107=CARTESIAN_POINT('Ctrl Pts',(0.116804197737899,0.479251095989714,
-1.34409133850666));
#57108=CARTESIAN_POINT('Ctrl Pts',(-0.0402897698814872,0.517538586457189,
-1.3362188756874));
#57109=CARTESIAN_POINT('Ctrl Pts',(-0.218034063260338,0.47109472203945,
-1.32834641286814));
#57110=CARTESIAN_POINT('Ctrl Pts',(-0.336318056393163,0.360852819953089,
-1.32047395004888));
#57111=CARTESIAN_POINT('Ctrl Pts',(-0.434430490466894,0.269411019045462,
-1.31394401756271));
#57112=CARTESIAN_POINT('Ctrl Pts',(-0.4916335119489,0.134075389234701,-1.30741408507653));
#57113=CARTESIAN_POINT('Ctrl Pts',(-0.492796742099722,-0.000388985907888563,
-1.30088415259036));
#57114=CARTESIAN_POINT('Origin',(0.,0.,-0.785));
#57115=CARTESIAN_POINT('',(-0.492699669112094,0.000410100521544665,-1.12911584740964));
#57116=CARTESIAN_POINT('',(-0.492749550373132,0.00040022685197263,-1.15088415259036));
#57117=CARTESIAN_POINT('',(-0.4925,-6.03138548580071E-17,-0.785));
#57118=CARTESIAN_POINT('Ctrl Pts',(-0.492699669112094,0.000410100521544665,
-1.12911584740964));
#57119=CARTESIAN_POINT('Ctrl Pts',(-0.49297563193663,0.0314429855949232,
-1.13062211359755));
#57120=CARTESIAN_POINT('Ctrl Pts',(-0.490290307645473,0.062428299335654,
-1.13212837978545));
#57121=CARTESIAN_POINT('Ctrl Pts',(-0.484469335446466,0.0928128968948493,
-1.13363464597335));
#57122=CARTESIAN_POINT('Ctrl Pts',(-0.454046168826502,0.25161724136183,
-1.14150710879261));
#57123=CARTESIAN_POINT('Ctrl Pts',(-0.337969510299702,0.39401239700866,
-1.14937957161187));
#57124=CARTESIAN_POINT('Ctrl Pts',(-0.188556356186219,0.455819340204937,
-1.15725203443113));
#57125=CARTESIAN_POINT('Ctrl Pts',(-0.039143202072734,0.517626283401215,
-1.16512449725039));
#57126=CARTESIAN_POINT('Ctrl Pts',(0.143606447627436,0.498845014146939,
-1.17299696006965));
#57127=CARTESIAN_POINT('Ctrl Pts',(0.277325367211442,0.407940450716456,
-1.18086942288891));
#57128=CARTESIAN_POINT('Ctrl Pts',(0.411044286795446,0.317035887285973,
-1.18874188570817));
#57129=CARTESIAN_POINT('Ctrl Pts',(0.495732476263288,0.154008029679284,
-1.19661434852743));
#57130=CARTESIAN_POINT('Ctrl Pts',(0.493220056252468,-0.00766471525244823,
-1.20448681134669));
#57131=CARTESIAN_POINT('Ctrl Pts',(0.490707636241647,-0.169337460184181,
-1.21235927416595));
#57132=CARTESIAN_POINT('Ctrl Pts',(0.400994606752165,-0.329655092440956,
-1.22023173698521));
#57133=CARTESIAN_POINT('Ctrl Pts',(0.26451559998051,-0.416360739939686,
-1.22810419980447));
#57134=CARTESIAN_POINT('Ctrl Pts',(0.128036593208856,-0.503066387438416,
-1.23597666262373));
#57135=CARTESIAN_POINT('Ctrl Pts',(-0.0552083908449711,-0.516160050179099,
-1.24384912544299));
#57136=CARTESIAN_POINT('Ctrl Pts',(-0.20262888612291,-0.449740264872263,
-1.25172158826224));
#57137=CARTESIAN_POINT('Ctrl Pts',(-0.350049381400848,-0.383320479565428,
-1.2595940510815));
#57138=CARTESIAN_POINT('Ctrl Pts',(-0.461645387902899,-0.237387246211074,
-1.26746651390076));
#57139=CARTESIAN_POINT('Ctrl Pts',(-0.487119361080433,-0.0777142560326435,
-1.27533897672002));
#57140=CARTESIAN_POINT('Ctrl Pts',(-0.49119313506329,-0.0521795006719227,
-1.27659793361656));
#57141=CARTESIAN_POINT('Ctrl Pts',(-0.493064414909343,-0.0262933632934072,
-1.2778568905131));
#57142=CARTESIAN_POINT('Ctrl Pts',(-0.492844994071537,-0.000375497391989388,
-1.27911584740964));
#57143=CARTESIAN_POINT('Ctrl Pts',(-0.492796742099722,-0.000388985907888563,
-1.30088415259036));
#57144=CARTESIAN_POINT('Ctrl Pts',(-0.493035897981524,-0.0280343716343784,
-1.29954162225727));
#57145=CARTESIAN_POINT('Ctrl Pts',(-0.490906259607873,-0.0556429295461318,
-1.29819909192419));
#57146=CARTESIAN_POINT('Ctrl Pts',(-0.486276335973135,-0.0828256273553652,
-1.2968565615911));
#57147=CARTESIAN_POINT('Ctrl Pts',(-0.45912692953348,-0.242222232822471,
-1.28898409877185));
#57148=CARTESIAN_POINT('Ctrl Pts',(-0.346004423767372,-0.386975504001697,
-1.28111163595259));
#57149=CARTESIAN_POINT('Ctrl Pts',(-0.197894517027637,-0.45184343470324,
-1.27323917313333));
#57150=CARTESIAN_POINT('Ctrl Pts',(-0.0497846102879024,-0.516711365404783,
-1.26536671031407));
#57151=CARTESIAN_POINT('Ctrl Pts',(0.13331269742546,-0.501693955628644,
-1.25749424749481));
#57152=CARTESIAN_POINT('Ctrl Pts',(0.268873574359746,-0.413559793115497,
-1.24962178467555));
#57153=CARTESIAN_POINT('Ctrl Pts',(0.404434451294034,-0.32542563060235,
-1.24174932185629));
#57154=CARTESIAN_POINT('Ctrl Pts',(0.492458897449246,-0.164174715352196,
-1.23387685903703));
#57155=CARTESIAN_POINT('Ctrl Pts',(0.493273304253071,-0.00248452317121441,
-1.22600439621777));
#57156=CARTESIAN_POINT('Ctrl Pts',(0.494087711056895,0.159205669009766,
-1.21813193339851));
#57157=CARTESIAN_POINT('Ctrl Pts',(0.407692078509334,0.321335138121573,
-1.21025947057925));
#57158=CARTESIAN_POINT('Ctrl Pts',(0.273025869168142,0.410830371438833,
-1.20238700775999));
#57159=CARTESIAN_POINT('Ctrl Pts',(0.138359659826949,0.500325604756093,
-1.19451454494073));
#57160=CARTESIAN_POINT('Ctrl Pts',(-0.0445771263078751,0.517186602278804,
-1.18664208212147));
#57161=CARTESIAN_POINT('Ctrl Pts',(-0.193332929681909,0.453813942791155,
-1.17876961930221));
#57162=CARTESIAN_POINT('Ctrl Pts',(-0.342088733055942,0.390441283303506,
-1.17089715648295));
#57163=CARTESIAN_POINT('Ctrl Pts',(-0.456663553669186,0.246834966805496,
-1.1630246936637));
#57164=CARTESIAN_POINT('Ctrl Pts',(-0.485417284176169,0.0877198949225954,
-1.15515223084444));
#57165=CARTESIAN_POINT('Ctrl Pts',(-0.490613589945532,0.0589649976818075,
-1.15372953809308));
#57166=CARTESIAN_POINT('Ctrl Pts',(-0.493007076876324,0.0297036021933078,
-1.15230684534172));
#57167=CARTESIAN_POINT('Ctrl Pts',(-0.492749550373132,0.00040022685197263,
-1.15088415259036));
#57168=CARTESIAN_POINT('Origin',(0.,0.,-0.785));
#57169=CARTESIAN_POINT('',(-0.491746356789813,-0.00010883115493171,-0.979115847409641));
#57170=CARTESIAN_POINT('',(-0.491736157223136,-8.20785977434006E-5,-1.00088415259036));
#57171=CARTESIAN_POINT('',(-0.4925,-6.03138548580071E-17,-0.785));
#57172=CARTESIAN_POINT('Ctrl Pts',(-0.491746356789813,-0.00010883115493171,
-0.979115847409641));
#57173=CARTESIAN_POINT('Ctrl Pts',(-0.491568688029523,0.0883286966854865,
-0.983387336681989));
#57174=CARTESIAN_POINT('Ctrl Pts',(-0.468769837714688,0.176851663470972,
-0.987658825954337));
#57175=CARTESIAN_POINT('Ctrl Pts',(-0.42390686631858,0.252245395083429,
-0.991930315226685));
#57176=CARTESIAN_POINT('Ctrl Pts',(-0.341223274775056,0.391197950288614,
-0.999802778045945));
#57177=CARTESIAN_POINT('Ctrl Pts',(-0.183593550391466,0.485553877341615,
-1.0076752408652));
#57178=CARTESIAN_POINT('Ctrl Pts',(-0.0220631010459361,0.492785947666456,
-1.01554770368446));
#57179=CARTESIAN_POINT('Ctrl Pts',(0.139467348299593,0.500018017991297,
-1.02342016650372));
#57180=CARTESIAN_POINT('Ctrl Pts',(0.304898522607063,0.420126231587979,
-1.03129262932298));
#57181=CARTESIAN_POINT('Ctrl Pts',(0.39966881688194,0.289118673655937,-1.03916509214224));
#57182=CARTESIAN_POINT('Ctrl Pts',(0.494439111156818,0.158111115723894,
-1.0470375549615));
#57183=CARTESIAN_POINT('Ctrl Pts',(0.518548525399102,-0.0240122137368738,
-1.05491001778076));
#57184=CARTESIAN_POINT('Ctrl Pts',(0.461130687884588,-0.17516637624073,
-1.06278248060002));
#57185=CARTESIAN_POINT('Ctrl Pts',(0.403712850370075,-0.326320538744583,
-1.07065494341928));
#57186=CARTESIAN_POINT('Ctrl Pts',(0.264767761098766,-0.446505534291526,
-1.07852740623854));
#57187=CARTESIAN_POINT('Ctrl Pts',(0.10691946257642,-0.481552696116318,
-1.0863998690578));
#57188=CARTESIAN_POINT('Ctrl Pts',(-0.0509288359459257,-0.51659985794111,
-1.09427233187706));
#57189=CARTESIAN_POINT('Ctrl Pts',(-0.227680343719308,-0.466509186043751,
-1.10214479469632));
#57190=CARTESIAN_POINT('Ctrl Pts',(-0.343671260249434,-0.353857083451506,
-1.11001725751558));
#57191=CARTESIAN_POINT('Ctrl Pts',(-0.437469223991527,-0.262759106553689,
-1.11638345414693));
#57192=CARTESIAN_POINT('Ctrl Pts',(-0.491533319088407,-0.130749617463121,
-1.12274965077829));
#57193=CARTESIAN_POINT('Ctrl Pts',(-0.492699669112094,0.000410100521544665,
-1.12911584740964));
#57194=CARTESIAN_POINT('Ctrl Pts',(-0.492749550373132,0.00040022685197263,
-1.15088415259036));
#57195=CARTESIAN_POINT('Ctrl Pts',(-0.4915820553322,-0.132446470359704,
-1.14443438252246));
#57196=CARTESIAN_POINT('Ctrl Pts',(-0.435929409661543,-0.266155961616792,
-1.13798461245456));
#57197=CARTESIAN_POINT('Ctrl Pts',(-0.339936079966906,-0.357446751494053,
-1.13153484238666));
#57198=CARTESIAN_POINT('Ctrl Pts',(-0.222768504849936,-0.468874498760009,
-1.1236623795674));
#57199=CARTESIAN_POINT('Ctrl Pts',(-0.0455007142152706,-0.517106166024128,
-1.11578991674814));
#57200=CARTESIAN_POINT('Ctrl Pts',(0.111970798701792,-0.480403224995691,
-1.10791745392888));
#57201=CARTESIAN_POINT('Ctrl Pts',(0.269442311618853,-0.443700283967254,
-1.10004499110962));
#57202=CARTESIAN_POINT('Ctrl Pts',(0.407117546818311,-0.322062734646261,
-1.09217252829036));
#57203=CARTESIAN_POINT('Ctrl Pts',(0.462944797876401,-0.17031392463671,
-1.0843000654711));
#57204=CARTESIAN_POINT('Ctrl Pts',(0.518772048934492,-0.0185651146271575,
-1.07642760265184));
#57205=CARTESIAN_POINT('Ctrl Pts',(0.492751315851212,0.163294956070952,
-1.06855513983258));
#57206=CARTESIAN_POINT('Ctrl Pts',(0.396610422658507,0.293300002140747,
-1.06068267701332));
#57207=CARTESIAN_POINT('Ctrl Pts',(0.300469529465803,0.423305048210542,
-1.05281021419406));
#57208=CARTESIAN_POINT('Ctrl Pts',(0.134208476163673,0.501455069652022,
-1.0449377513748));
#57209=CARTESIAN_POINT('Ctrl Pts',(-0.0272370970959901,0.49252701361753,
-1.03706528855555));
#57210=CARTESIAN_POINT('Ctrl Pts',(-0.188682670355654,0.483598957583038,
-1.02919282573629));
#57211=CARTESIAN_POINT('Ctrl Pts',(-0.345312763572852,0.387592824072574,
-1.02132036291703));
#57212=CARTESIAN_POINT('Ctrl Pts',(-0.426532513251872,0.247779607313462,
-1.01344790009777));
#57213=CARTESIAN_POINT('Ctrl Pts',(-0.469739001954307,0.173403138606935,
-1.00925998426196));
#57214=CARTESIAN_POINT('Ctrl Pts',(-0.491604942376349,0.0866296016571418,
-1.00507206842616));
#57215=CARTESIAN_POINT('Ctrl Pts',(-0.491736157223136,-8.20785977434006E-5,
-1.00088415259036));
#57216=CARTESIAN_POINT('Origin',(0.,0.,-0.785));
#57217=CARTESIAN_POINT('',(-0.493065289251647,-0.000280683390702752,-0.829115847409641));
#57218=CARTESIAN_POINT('',(-0.493025735351581,-0.000302692969106977,-0.850884152590359));
#57219=CARTESIAN_POINT('',(-0.4925,-6.03138548580071E-17,-0.785));
#57220=CARTESIAN_POINT('Ctrl Pts',(-0.493065289251647,-0.000280683390702752,
-0.829115847409641));
#57221=CARTESIAN_POINT('Ctrl Pts',(-0.492073025151649,0.144413259987423,
-0.836152559766433));
#57222=CARTESIAN_POINT('Ctrl Pts',(-0.424455104245118,0.289914875416531,
-0.843189272123224));
#57223=CARTESIAN_POINT('Ctrl Pts',(-0.31267145716183,0.38152500642237,-0.850225984480016));
#57224=CARTESIAN_POINT('Ctrl Pts',(-0.187611264156348,0.484015674456412,
-0.858098447299275));
#57225=CARTESIAN_POINT('Ctrl Pts',(-0.00727120091729211,0.519053262387343,
-0.865970910118535));
#57226=CARTESIAN_POINT('Ctrl Pts',(0.147067531334825,0.470845953445812,
-0.873843372937794));
#57227=CARTESIAN_POINT('Ctrl Pts',(0.301406263586942,0.422638644504282,
-0.881715835757054));
#57228=CARTESIAN_POINT('Ctrl Pts',(0.429743664852121,0.29118643869029,-0.889588298576313));
#57229=CARTESIAN_POINT('Ctrl Pts',(0.474236691555723,0.135736255404997,
-0.897460761395573));
#57230=CARTESIAN_POINT('Ctrl Pts',(0.518729718259325,-0.0197139278802952,
-0.905333224214832));
#57231=CARTESIAN_POINT('Ctrl Pts',(0.479378370401352,-0.199162088636888,
-0.913205687034091));
#57232=CARTESIAN_POINT('Ctrl Pts',(0.373918722627788,-0.321729015660929,
-0.921078149853351));
#57233=CARTESIAN_POINT('Ctrl Pts',(0.268459074854222,-0.444295942684971,
-0.92895061267261));
#57234=CARTESIAN_POINT('Ctrl Pts',(0.0968911271650634,-0.509981635976461,
-0.936823075491869));
#57235=CARTESIAN_POINT('Ctrl Pts',(-0.063457605803671,-0.489180848883629,
-0.944695538311129));
#57236=CARTESIAN_POINT('Ctrl Pts',(-0.223806338772403,-0.468380061790797,
-0.952568001130388));
#57237=CARTESIAN_POINT('Ctrl Pts',(-0.372935857020711,-0.361092794313646,
-0.960440463949648));
#57238=CARTESIAN_POINT('Ctrl Pts',(-0.443631886793136,-0.215674568896387,
-0.968312926768907));
#57239=CARTESIAN_POINT('Ctrl Pts',(-0.475969230128613,-0.149158258182883,
-0.971913900315818));
#57240=CARTESIAN_POINT('Ctrl Pts',(-0.491896136050658,-0.0746639050419697,
-0.97551487386273));
#57241=CARTESIAN_POINT('Ctrl Pts',(-0.491746356789813,-0.00010883115493171,
-0.979115847409641));
#57242=CARTESIAN_POINT('Ctrl Pts',(-0.491736157223136,-8.20785977434006E-5,
-1.00088415259036));
#57243=CARTESIAN_POINT('Ctrl Pts',(-0.491851600629084,-0.0763714006472224,
-0.997199605606902));
#57244=CARTESIAN_POINT('Ctrl Pts',(-0.475143152162094,-0.152612842159027,
-0.993515058623445));
#57245=CARTESIAN_POINT('Ctrl Pts',(-0.441342370069444,-0.220321653526826,
-0.989830511639988));
#57246=CARTESIAN_POINT('Ctrl Pts',(-0.369123071067154,-0.36498939760024,
-0.981958048820729));
#57247=CARTESIAN_POINT('Ctrl Pts',(-0.218875066921732,-0.470704585739309,
-0.974085586001469));
#57248=CARTESIAN_POINT('Ctrl Pts',(-0.0583167449524224,-0.489820248550804,
-0.966213123182209));
#57249=CARTESIAN_POINT('Ctrl Pts',(0.102241577016886,-0.508935911362299,
-0.95834066036295));
#57250=CARTESIAN_POINT('Ctrl Pts',(0.273110216810081,-0.441452048846223,
-0.950468197543691));
#57251=CARTESIAN_POINT('Ctrl Pts',(0.377276845346877,-0.317784361800476,
-0.942595734724432));
#57252=CARTESIAN_POINT('Ctrl Pts',(0.481443473883674,-0.194116674754727,
-0.934723271905173));
#57253=CARTESIAN_POINT('Ctrl Pts',(0.518908091164071,-0.014265163179308,
-0.926850809085913));
#57254=CARTESIAN_POINT('Ctrl Pts',(0.472784992262523,0.140709167173152,
-0.918978346266654));
#57255=CARTESIAN_POINT('Ctrl Pts',(0.426661893360975,0.295683497525611,
-0.911105883447394));
#57256=CARTESIAN_POINT('Ctrl Pts',(0.296951078277482,0.425780646655112,
-0.903233420628134));
#57257=CARTESIAN_POINT('Ctrl Pts',(0.142114602924627,0.472364433749384,
-0.895360957808875));
#57258=CARTESIAN_POINT('Ctrl Pts',(-0.0127218724282286,0.518948220843657,
-0.887488494989616));
#57259=CARTESIAN_POINT('Ctrl Pts',(-0.192684008050446,0.482018645902701,
-0.879616032170357));
#57260=CARTESIAN_POINT('Ctrl Pts',(-0.316660938750639,0.378220264536789,
-0.871743569351098));
#57261=CARTESIAN_POINT('Ctrl Pts',(-0.426160194810032,0.286543164002481,
-0.864790430430852));
#57262=CARTESIAN_POINT('Ctrl Pts',(-0.491986368099344,0.142702872821624,
-0.857837291510605));
#57263=CARTESIAN_POINT('Ctrl Pts',(-0.493025735351581,-0.000302692969106977,
-0.850884152590359));
#57264=CARTESIAN_POINT('Origin',(0.,0.,-0.785));
#57265=CARTESIAN_POINT('',(-0.492442945015723,0.000430954536069797,-0.679115847409641));
#57266=CARTESIAN_POINT('',(-0.492493380507229,0.000430700144442887,-0.700884152590359));
#57267=CARTESIAN_POINT('',(-0.4925,-6.03138548580071E-17,-0.785));
#57268=CARTESIAN_POINT('Ctrl Pts',(-0.492442945015723,0.000430954536069797,
-0.679115847409641));
#57269=CARTESIAN_POINT('Ctrl Pts',(-0.492794956060319,0.0402362573843546,
-0.681045320031617));
#57270=CARTESIAN_POINT('Ctrl Pts',(-0.488365618774981,0.0799642458113595,
-0.682974792653592));
#57271=CARTESIAN_POINT('Ctrl Pts',(-0.478850766148977,0.118434430852565,
-0.684904265275568));
#57272=CARTESIAN_POINT('Ctrl Pts',(-0.440029109559597,0.27539706299233,
-0.692776728094828));
#57273=CARTESIAN_POINT('Ctrl Pts',(-0.316547316553595,0.411420655704654,
-0.700649190914088));
#57274=CARTESIAN_POINT('Ctrl Pts',(-0.164059955984402,0.465197916472846,
-0.708521653733347));
#57275=CARTESIAN_POINT('Ctrl Pts',(-0.0115725954152106,0.518975177241037,
-0.716394116552607));
#57276=CARTESIAN_POINT('Ctrl Pts',(0.16992033271717,0.490506106065098,-0.724266579371865));
#57277=CARTESIAN_POINT('Ctrl Pts',(0.298618018623332,0.392622018743623,
-0.732139042191125));
#57278=CARTESIAN_POINT('Ctrl Pts',(0.427315704529493,0.294737931422147,
-0.740011505010384));
#57279=CARTESIAN_POINT('Ctrl Pts',(0.503218148209435,0.127438827955136,
-0.747883967829644));
#57280=CARTESIAN_POINT('Ctrl Pts',(0.49211530399918,-0.0338717909113338,
-0.755756430648903));
#57281=CARTESIAN_POINT('Ctrl Pts',(0.481012459788925,-0.195182409777806,
-0.763628893468163));
#57282=CARTESIAN_POINT('Ctrl Pts',(0.382904327688472,-0.350504544043738,
-0.771501356287422));
#57283=CARTESIAN_POINT('Ctrl Pts',(0.242009295357658,-0.42983284147396,
-0.779373819106681));
#57284=CARTESIAN_POINT('Ctrl Pts',(0.101114263026846,-0.509161138904182,
-0.78724628192594));
#57285=CARTESIAN_POINT('Ctrl Pts',(-0.082567669534326,-0.512495599498696,
-0.7951187447452));
#57286=CARTESIAN_POINT('Ctrl Pts',(-0.22624908475085,-0.438333346094748,
-0.80299120756446));
#57287=CARTESIAN_POINT('Ctrl Pts',(-0.369930499967376,-0.364171092690799,
-0.810863670383719));
#57288=CARTESIAN_POINT('Ctrl Pts',(-0.473611397839254,-0.212512125288386,
-0.818736133202978));
#57289=CARTESIAN_POINT('Ctrl Pts',(-0.490561685389237,-0.0517107675186028,
-0.826608596022238));
#57290=CARTESIAN_POINT('Ctrl Pts',(-0.492361149036649,-0.0346398950093308,
-0.827444346484705));
#57291=CARTESIAN_POINT('Ctrl Pts',(-0.493183140477961,-0.0174659858392047,
-0.828280096947173));
#57292=CARTESIAN_POINT('Ctrl Pts',(-0.493065289251647,-0.000280683390702752,
-0.829115847409641));
#57293=CARTESIAN_POINT('Ctrl Pts',(-0.493025735351581,-0.000302692969106977,
-0.850884152590359));
#57294=CARTESIAN_POINT('Ctrl Pts',(-0.49316315748075,-0.0192104748833397,
-0.849964828691345));
#57295=CARTESIAN_POINT('Ctrl Pts',(-0.492168017944618,-0.0381036646601338,
-0.849045504792332));
#57296=CARTESIAN_POINT('Ctrl Pts',(-0.489991515851596,-0.056859766351132,
-0.848126180893318));
#57297=CARTESIAN_POINT('Ctrl Pts',(-0.471353436474192,-0.21747422808227,
-0.840253718074059));
#57298=CARTESIAN_POINT('Ctrl Pts',(-0.366085551941217,-0.368035963753677,
-0.8323812552548));
#57299=CARTESIAN_POINT('Ctrl Pts',(-0.221633227142547,-0.440685183847334,
-0.824508792435541));
#57300=CARTESIAN_POINT('Ctrl Pts',(-0.0771809023438781,-0.51333440394099,
-0.816636329616282));
#57301=CARTESIAN_POINT('Ctrl Pts',(0.106455862720485,-0.508071108456897,
-0.808763866797022));
#57302=CARTESIAN_POINT('Ctrl Pts',(0.246510007949834,-0.427267521134977,
-0.800891403977762));
#57303=CARTESIAN_POINT('Ctrl Pts',(0.386564153179185,-0.346463933813055,
-0.793018941158503));
#57304=CARTESIAN_POINT('Ctrl Pts',(0.483035678573522,-0.190120054653303,
-0.785146478339243));
#57305=CARTESIAN_POINT('Ctrl Pts',(0.492443832674891,-0.0287017472764125,
-0.777274015519984));
#57306=CARTESIAN_POINT('Ctrl Pts',(0.50185198677626,0.132716560100476,-0.769401552700724));
#57307=CARTESIAN_POINT('Ctrl Pts',(0.424196769584665,0.299209295694505,
-0.761529089881465));
#57308=CARTESIAN_POINT('Ctrl Pts',(0.294478220586881,0.395736397411412,
-0.753656627062206));
#57309=CARTESIAN_POINT('Ctrl Pts',(0.164759671589095,0.49226349912832,-0.745784164242946));
#57310=CARTESIAN_POINT('Ctrl Pts',(-0.0170222092148785,0.518824966968104,
-0.737911701423687));
#57311=CARTESIAN_POINT('Ctrl Pts',(-0.16893637796105,0.463449262419794,
-0.730039238604428));
#57312=CARTESIAN_POINT('Ctrl Pts',(-0.32085054670722,0.408073557871484,
-0.722166775785168));
#57313=CARTESIAN_POINT('Ctrl Pts',(-0.442897003395587,0.270760680935079,
-0.714294312965909));
#57314=CARTESIAN_POINT('Ctrl Pts',(-0.480068100660248,0.113399018360725,
-0.706421850146649));
#57315=CARTESIAN_POINT('Ctrl Pts',(-0.488783810056108,0.0765015732494849,
-0.704575950961219));
#57316=CARTESIAN_POINT('Ctrl Pts',(-0.492833179805818,0.0385018713240789,
-0.702730051775789));
#57317=CARTESIAN_POINT('Ctrl Pts',(-0.492493380507229,0.000430700144442887,
-0.700884152590359));
#57318=CARTESIAN_POINT('Origin',(0.,0.,-0.785));
#57319=CARTESIAN_POINT('',(-0.491840351485494,-0.000235604174339266,-0.529115847409641));
#57320=CARTESIAN_POINT('',(-0.491816277089331,-0.000212068874708314,-0.550884152590359));
#57321=CARTESIAN_POINT('',(-0.4925,-6.03138548580071E-17,-0.785));
#57322=CARTESIAN_POINT('Ctrl Pts',(-0.491840351485494,-0.000235604174339266,
-0.529115847409641));
#57323=CARTESIAN_POINT('Ctrl Pts',(-0.491412743741431,0.0969174984233381,
-0.53381054311606));
#57324=CARTESIAN_POINT('Ctrl Pts',(-0.463541921665293,0.194296900018551,
-0.53850523882248));
#57325=CARTESIAN_POINT('Ctrl Pts',(-0.40989902803581,0.274422225108048,
-0.543199934528899));
#57326=CARTESIAN_POINT('Ctrl Pts',(-0.319946087094793,0.408783146900192,
-0.551072397348158));
#57327=CARTESIAN_POINT('Ctrl Pts',(-0.157523578784168,0.494626608342158,
-0.558944860167418));
#57328=CARTESIAN_POINT('Ctrl Pts',(0.00416292928221056,0.493262040552515,
-0.566817322986677));
#57329=CARTESIAN_POINT('Ctrl Pts',(0.165849437348594,0.491897472762873,
-0.574689785805937));
#57330=CARTESIAN_POINT('Ctrl Pts',(0.326799945170732,0.403324875741616,
-0.582562248625196));
#57331=CARTESIAN_POINT('Ctrl Pts',(0.414472332492721,0.267464869118486,
-0.590434711444456));
#57332=CARTESIAN_POINT('Ctrl Pts',(0.502144719814708,0.13160486249536,-0.598307174263715));
#57333=CARTESIAN_POINT('Ctrl Pts',(0.516538986636549,-0.0515425537296376,
-0.606179637082975));
#57334=CARTESIAN_POINT('Ctrl Pts',(0.451167482309357,-0.199430874191682,
-0.614052099902234));
#57335=CARTESIAN_POINT('Ctrl Pts',(0.385795977982164,-0.347319194653728,
-0.621924562721493));
#57336=CARTESIAN_POINT('Ctrl Pts',(0.240658702505937,-0.459948419352821,
-0.629797025540753));
#57337=CARTESIAN_POINT('Ctrl Pts',(0.0811705830822261,-0.486555348430648,
-0.637669488360012));
#57338=CARTESIAN_POINT('Ctrl Pts',(-0.0783175363414848,-0.513162277508476,
-0.645541951179271));
#57339=CARTESIAN_POINT('Ctrl Pts',(-0.252156499712679,-0.453746910965039,
-0.653414413998531));
#57340=CARTESIAN_POINT('Ctrl Pts',(-0.361995221311897,-0.335088391909719,
-0.661286876817791));
#57341=CARTESIAN_POINT('Ctrl Pts',(-0.44491342121109,-0.245512050711285,
-0.667229867015074));
#57342=CARTESIAN_POINT('Ctrl Pts',(-0.491358711861264,-0.122173803848648,
-0.673172857212357));
#57343=CARTESIAN_POINT('Ctrl Pts',(-0.492442945015723,0.000430954536069797,
-0.679115847409641));
#57344=CARTESIAN_POINT('Ctrl Pts',(-0.492493380507229,0.000430700144442887,
-0.700884152590359));
#57345=CARTESIAN_POINT('Ctrl Pts',(-0.491383990508121,-0.123865543951382,
-0.69485758895653));
#57346=CARTESIAN_POINT('Ctrl Pts',(-0.443489685503747,-0.248923591237708,
-0.688831025322701));
#57347=CARTESIAN_POINT('Ctrl Pts',(-0.358456136920689,-0.338871533976663,
-0.682804461688872));
#57348=CARTESIAN_POINT('Ctrl Pts',(-0.247377338075509,-0.456369975527401,
-0.674931998869612));
#57349=CARTESIAN_POINT('Ctrl Pts',(-0.0729240025441891,-0.51395641041657,
-0.667059536050353));
#57350=CARTESIAN_POINT('Ctrl Pts',(0.086275879790834,-0.485676014645106,
-0.659187073231093));
#57351=CARTESIAN_POINT('Ctrl Pts',(0.245475762125855,-0.457395618873642,
-0.651314610411833));
#57352=CARTESIAN_POINT('Ctrl Pts',(0.38942219126458,-0.343248392441546,
-0.643442147592574));
#57353=CARTESIAN_POINT('Ctrl Pts',(0.453236967301004,-0.194681714887699,
-0.635569684773315));
#57354=CARTESIAN_POINT('Ctrl Pts',(0.517051743337429,-0.0461150373338516,
-0.627697221954055));
#57355=CARTESIAN_POINT('Ctrl Pts',(0.500734866271556,0.136871091341746,
-0.619824759134797));
#57356=CARTESIAN_POINT('Ctrl Pts',(0.411640527669831,0.271802859830283,
-0.611952296315537));
#57357=CARTESIAN_POINT('Ctrl Pts',(0.322546189068105,0.406734628318821,
-0.604079833496278));
#57358=CARTESIAN_POINT('Ctrl Pts',(0.160674388930523,0.493612036620296,
-0.596207370677018));
#57359=CARTESIAN_POINT('Ctrl Pts',(-0.00101751587672065,0.493278504794958,
-0.588334907857758));
#57360=CARTESIAN_POINT('Ctrl Pts',(-0.162709420683966,0.49294497296962,
-0.580462445038499));
#57361=CARTESIAN_POINT('Ctrl Pts',(-0.324221430160874,0.405400501017469,
-0.57258998221924));
#57362=CARTESIAN_POINT('Ctrl Pts',(-0.412758348824488,0.270102321606191,
-0.56471751939998));
#57363=CARTESIAN_POINT('Ctrl Pts',(-0.464616905254506,0.190854383257034,
-0.560106397130107));
#57364=CARTESIAN_POINT('Ctrl Pts',(-0.491439361299384,0.0952232297534331,
-0.555495274860233));
#57365=CARTESIAN_POINT('Ctrl Pts',(-0.491816277089331,-0.000212068874708314,
-0.550884152590359));
#57366=CARTESIAN_POINT('Origin',(0.,0.,-0.785));
#57367=CARTESIAN_POINT('',(-0.493221679829005,-0.00014905999630227,-0.379115847409641));
#57368=CARTESIAN_POINT('',(-0.493197442025473,-0.000177332146063924,-0.400884152590359));
#57369=CARTESIAN_POINT('',(-0.4925,-6.03138548580071E-17,-0.785));
#57370=CARTESIAN_POINT('Ctrl Pts',(-0.493221679829005,-0.00014905999630227,
-0.379115847409641));
#57371=CARTESIAN_POINT('Ctrl Pts',(-0.492603881529428,0.153118260426883,
-0.386575766200504));
#57372=CARTESIAN_POINT('Ctrl Pts',(-0.415450443578965,0.306923075433429,
-0.394035684991367));
#57373=CARTESIAN_POINT('Ctrl Pts',(-0.291948826220119,0.397606162425599,
-0.40149560378223));
#57374=CARTESIAN_POINT('Ctrl Pts',(-0.161617395271197,0.493304152001024,
-0.409368066601489));
#57375=CARTESIAN_POINT('Ctrl Pts',(0.0203301985725902,0.518705930657618,
-0.417240529420749));
#57376=CARTESIAN_POINT('Ctrl Pts',(0.171888191256297,0.462362651006137,
-0.425112992240008));
#57377=CARTESIAN_POINT('Ctrl Pts',(0.32344618394,0.406019371354658,-0.432985455059267));
#57378=CARTESIAN_POINT('Ctrl Pts',(0.444614575463624,0.267931033395105,
-0.440857917878527));
#57379=CARTESIAN_POINT('Ctrl Pts',(0.480781488250625,0.110335528963639,
-0.448730380697786));
#57380=CARTESIAN_POINT('Ctrl Pts',(0.516948401037627,-0.0472599754678293,
-0.456602843517046));
#57381=CARTESIAN_POINT('Ctrl Pts',(0.468113835088005,-0.224362646371213,
-0.464475306336305));
#57382=CARTESIAN_POINT('Ctrl Pts',(0.356288044656636,-0.341150408155024,
-0.472347769155565));
#57383=CARTESIAN_POINT('Ctrl Pts',(0.244462254225269,-0.457938169938832,
-0.480220231974824));
#57384=CARTESIAN_POINT('Ctrl Pts',(0.0696452393121575,-0.514411022603067,
-0.488092694794083));
#57385=CARTESIAN_POINT('Ctrl Pts',(-0.0893710915641801,-0.485116046552094,
-0.495965157613343));
#57386=CARTESIAN_POINT('Ctrl Pts',(-0.248387422440518,-0.45582107050112,
-0.503837620432602));
#57387=CARTESIAN_POINT('Ctrl Pts',(-0.391603069280081,-0.340758265734937,
-0.511710083251862));
#57388=CARTESIAN_POINT('Ctrl Pts',(-0.454469205914159,-0.191787672280683,
-0.519582546071121));
#57389=CARTESIAN_POINT('Ctrl Pts',(-0.479845501248111,-0.131654793469102,
-0.522760313183961));
#57390=CARTESIAN_POINT('Ctrl Pts',(-0.492129792572042,-0.0659970408363866,
-0.525938080296801));
#57391=CARTESIAN_POINT('Ctrl Pts',(-0.491840351485494,-0.000235604174339266,
-0.529115847409641));
#57392=CARTESIAN_POINT('Ctrl Pts',(-0.491816277089331,-0.000212068874708314,
-0.550884152590359));
#57393=CARTESIAN_POINT('Ctrl Pts',(-0.492082860944087,-0.06771125693402,
-0.547622812040973));
#57394=CARTESIAN_POINT('Ctrl Pts',(-0.479120309212638,-0.135112470413207,
-0.544361471491588));
#57395=CARTESIAN_POINT('Ctrl Pts',(-0.452429949774634,-0.196549889717956,
-0.541100130942202));
#57396=CARTESIAN_POINT('Ctrl Pts',(-0.388002804210847,-0.344852034760429,
-0.533227668122942));
#57397=CARTESIAN_POINT('Ctrl Pts',(-0.243586685232952,-0.458404437974975,
-0.525355205303683));
#57398=CARTESIAN_POINT('Ctrl Pts',(-0.0842714866745568,-0.486027813145279,
-0.517482742484424));
#57399=CARTESIAN_POINT('Ctrl Pts',(0.0750437118838385,-0.513651188315582,
-0.509610279665164));
#57400=CARTESIAN_POINT('Ctrl Pts',(0.249257990022733,-0.455345535441644,
-0.501737816845905));
#57401=CARTESIAN_POINT('Ctrl Pts',(0.35985110298877,-0.337389837552566,
-0.493865354026646));
#57402=CARTESIAN_POINT('Ctrl Pts',(0.470444215954808,-0.219434139663487,
-0.485992891207386));
#57403=CARTESIAN_POINT('Ctrl Pts',(0.517416163747986,-0.0418283967592656,
-0.478120428388126));
#57404=CARTESIAN_POINT('Ctrl Pts',(0.479596186721551,0.115378576999044,
-0.470247965568867));
#57405=CARTESIAN_POINT('Ctrl Pts',(0.441776209695117,0.272585550757351,
-0.462375502749608));
#57406=CARTESIAN_POINT('Ctrl Pts',(0.319164307849076,0.409393755369748,
-0.454503039930348));
#57407=CARTESIAN_POINT('Ctrl Pts',(0.167022978541554,0.464142266181422,
-0.446630577111089));
#57408=CARTESIAN_POINT('Ctrl Pts',(0.0148816492340293,0.518890776993097,
-0.43875811429183));
#57409=CARTESIAN_POINT('Ctrl Pts',(-0.166789107534976,0.491579594004046,
-0.43088565147257));
#57410=CARTESIAN_POINT('Ctrl Pts',(-0.296108328455227,0.394518158722321,
-0.423013188653311));
#57411=CARTESIAN_POINT('Ctrl Pts',(-0.417277936538399,0.303573471696024,
-0.415636843298994));
#57412=CARTESIAN_POINT('Ctrl Pts',(-0.492486417081148,0.151392754252931,
-0.408260497944676));
#57413=CARTESIAN_POINT('Ctrl Pts',(-0.493197442025473,-0.000177332146063924,
-0.400884152590359));
#57414=CARTESIAN_POINT('Origin',(0.,0.,-0.785));
#57415=CARTESIAN_POINT('',(-0.492199160006355,0.000404087486738508,-0.229115847409641));
#57416=CARTESIAN_POINT('',(-0.492244893268066,0.000412969905903395,-0.250884152590359));
#57417=CARTESIAN_POINT('',(-0.4925,-6.03138548580071E-17,-0.785));
#57418=CARTESIAN_POINT('Ctrl Pts',(-0.492199160006355,0.000404087486738508,
-0.229115847409641));
#57419=CARTESIAN_POINT('Ctrl Pts',(-0.492584826275126,0.0490014356714362,
-0.231468526465688));
#57420=CARTESIAN_POINT('Ctrl Pts',(-0.485956433324197,0.0974958164498649,
-0.233821205521735));
#57421=CARTESIAN_POINT('Ctrl Pts',(-0.471877297107457,0.143720885963992,
-0.236173884577782));
#57422=CARTESIAN_POINT('Ctrl Pts',(-0.424766121399625,0.298397802108716,
-0.244046347397041));
#57423=CARTESIAN_POINT('Ctrl Pts',(-0.294230090276064,0.427665580216661,
-0.251918810216301));
#57424=CARTESIAN_POINT('Ctrl Pts',(-0.139100117626822,0.473261186203299,
-0.259791273035561));
#57425=CARTESIAN_POINT('Ctrl Pts',(0.0160298550224196,0.518856792189937,
-0.26766373585482));
#57426=CARTESIAN_POINT('Ctrl Pts',(0.195753769197341,0.480780226055272,
-0.275536198674079));
#57427=CARTESIAN_POINT('Ctrl Pts',(0.319066529828403,0.376193347566822,
-0.283408661493339));
#57428=CARTESIAN_POINT('Ctrl Pts',(0.442379290459466,0.271606469078371,
-0.291281124312598));
#57429=CARTESIAN_POINT('Ctrl Pts',(0.509280897546665,0.100509278236134,
-0.299153587131858));
#57430=CARTESIAN_POINT('Ctrl Pts',(0.489618910158042,-0.0599830637448122,
-0.307026049951117));
#57431=CARTESIAN_POINT('Ctrl Pts',(0.469956922769419,-0.220475405725756,
-0.314898512770376));
#57432=CARTESIAN_POINT('Ctrl Pts',(0.363731340904977,-0.37036289884541,
-0.322770975589636));
#57433=CARTESIAN_POINT('Ctrl Pts',(0.218818741885396,-0.442089549274763,
-0.330643438408895));
#57434=CARTESIAN_POINT('Ctrl Pts',(0.0739061428658151,-0.513816199704116,
-0.338515901228154));
#57435=CARTESIAN_POINT('Ctrl Pts',(-0.109693473308903,-0.507382007443169,
-0.346388364047414));
#57436=CARTESIAN_POINT('Ctrl Pts',(-0.24922956536185,-0.425686980138714,
-0.354260826866673));
#57437=CARTESIAN_POINT('Ctrl Pts',(-0.388765657414798,-0.34399195283426,
-0.362133289685933));
#57438=CARTESIAN_POINT('Ctrl Pts',(-0.484238225345974,-0.187036090486295,
-0.370005752505192));
#57439=CARTESIAN_POINT('Ctrl Pts',(-0.492616875284533,-0.025561059065186,
-0.377878215324452));
#57440=CARTESIAN_POINT('Ctrl Pts',(-0.493055945252538,-0.0170992140902034,
-0.378290759352848));
#57441=CARTESIAN_POINT('Ctrl Pts',(-0.493255844946132,-0.00862495893857167,
-0.378703303381244));
#57442=CARTESIAN_POINT('Ctrl Pts',(-0.493221679829005,-0.00014905999630227,
-0.379115847409641));
#57443=CARTESIAN_POINT('Ctrl Pts',(-0.493197442025473,-0.000177332146063924,
-0.400884152590359));
#57444=CARTESIAN_POINT('Ctrl Pts',(-0.493245264066869,-0.0103716171765687,
-0.400388035125417));
#57445=CARTESIAN_POINT('Ctrl Pts',(-0.492956087592501,-0.0205631399415184,
-0.399891917660475));
#57446=CARTESIAN_POINT('Ctrl Pts',(-0.492321230439843,-0.0307330836272979,
-0.399395800195532));
#57447=CARTESIAN_POINT('Ctrl Pts',(-0.482247226432713,-0.19211120312079,
-0.391523337376273));
#57448=CARTESIAN_POINT('Ctrl Pts',(-0.385131533346962,-0.348055754533375,
-0.383650874557014));
#57449=CARTESIAN_POINT('Ctrl Pts',(-0.244745220248979,-0.428280861698101,
-0.375778411737754));
#57450=CARTESIAN_POINT('Ctrl Pts',(-0.104358907150996,-0.508505968862826,
-0.367905948918495));
#57451=CARTESIAN_POINT('Ctrl Pts',(0.0792980259592206,-0.51301163177969,
-0.360033486099235));
#57452=CARTESIAN_POINT('Ctrl Pts',(0.223449398871474,-0.439767088000122,
-0.352161023279976));
#57453=CARTESIAN_POINT('Ctrl Pts',(0.367600771783729,-0.366522544220555,
-0.344288560460717));
#57454=CARTESIAN_POINT('Ctrl Pts',(0.472246584498022,-0.215527793744555,
-0.336416097641457));
#57455=CARTESIAN_POINT('Ctrl Pts',(0.49022190455631,-0.0548378132669632,
-0.328543634822198));
#57456=CARTESIAN_POINT('Ctrl Pts',(0.508197224614599,0.105852167210629,
-0.320671172002939));
#57457=CARTESIAN_POINT('Ctrl Pts',(0.439502052016882,0.276237377689811,
-0.312798709183679));
#57458=CARTESIAN_POINT('Ctrl Pts',(0.315097926507763,0.379523419652241,
-0.30492624636442));
#57459=CARTESIAN_POINT('Ctrl Pts',(0.190693800998646,0.482809461614669,
-0.297053783545161));
#57460=CARTESIAN_POINT('Ctrl Pts',(0.0105807225781267,0.518996335060344,
-0.289181320725901));
#57461=CARTESIAN_POINT('Ctrl Pts',(-0.144062197569475,0.471774143744356,
-0.281308857906642));
#57462=CARTESIAN_POINT('Ctrl Pts',(-0.298705117717077,0.424551952428368,
-0.273436395087382));
#57463=CARTESIAN_POINT('Ctrl Pts',(-0.427877879591762,0.293920696350717,
-0.265563932268123));
#57464=CARTESIAN_POINT('Ctrl Pts',(-0.473361346043439,0.138757445912334,
-0.257691469448863));
#57465=CARTESIAN_POINT('Ctrl Pts',(-0.486471193836867,0.0940342364678234,
-0.255422363829362));
#57466=CARTESIAN_POINT('Ctrl Pts',(-0.492628267870041,0.0472729478900636,
-0.25315325820986));
#57467=CARTESIAN_POINT('Ctrl Pts',(-0.492244893268066,0.000412969905903395,
-0.250884152590359));
#57468=CARTESIAN_POINT('Origin',(0.,0.,-0.785));
#57469=CARTESIAN_POINT('',(-0.492093596265288,-0.000318355522334279,-0.0791158474096402));
#57470=CARTESIAN_POINT('',(-0.491975623968706,-0.000315807630563663,-0.100884152590359));
#57471=CARTESIAN_POINT('',(-0.4925,-6.03138548580071E-17,-0.785));
#57472=CARTESIAN_POINT('Ctrl Pts',(-0.492093596265288,-0.000318355522334279,
-0.0791158474096402));
#57473=CARTESIAN_POINT('Ctrl Pts',(-0.491378781731003,0.105499822008811,
-0.0842337495501311));
#57474=CARTESIAN_POINT('Ctrl Pts',(-0.457753103959109,0.211702860821235,
-0.089351651690622));
#57475=CARTESIAN_POINT('Ctrl Pts',(-0.394687347650209,0.295813436971342,
-0.0944695538311129));
#57476=CARTESIAN_POINT('Ctrl Pts',(-0.297678298223042,0.425194063109043,
-0.102342016650372));
#57477=CARTESIAN_POINT('Ctrl Pts',(-0.131010407576646,0.502301209513945,
-0.110214479469632));
#57478=CARTESIAN_POINT('Ctrl Pts',(0.0303537882400381,0.49234839688357,
-0.118086942288891));
#57479=CARTESIAN_POINT('Ctrl Pts',(0.191717984056725,0.482395584253196,
-0.12595940510815));
#57480=CARTESIAN_POINT('Ctrl Pts',(0.347778485043697,0.385382812587542,
-0.13383186792741));
#57481=CARTESIAN_POINT('Ctrl Pts',(0.428116051422676,0.245052162104028,
-0.141704330746669));
#57482=CARTESIAN_POINT('Ctrl Pts',(0.508453617801651,0.104721511620518,
-0.149576793565929));
#57483=CARTESIAN_POINT('Ctrl Pts',(0.513068249572635,-0.0789270176808498,
-0.157449256385188));
#57484=CARTESIAN_POINT('Ctrl Pts',(0.43992221351322,-0.223130098498712,
-0.165321719204447));
#57485=CARTESIAN_POINT('Ctrl Pts',(0.366776177453803,-0.36733317931658,
-0.173194182023707));
#57486=CARTESIAN_POINT('Ctrl Pts',(0.215869473563981,-0.472090811650941,
-0.181066644842966));
#57487=CARTESIAN_POINT('Ctrl Pts',(0.0551954744401251,-0.490182910244527,
-0.188939107662226));
#57488=CARTESIAN_POINT('Ctrl Pts',(-0.105478524683729,-0.508275008838114,
-0.196811570481485));
#57489=CARTESIAN_POINT('Ctrl Pts',(-0.275919819041619,-0.439701573690924,
-0.204684033300745));
#57490=CARTESIAN_POINT('Ctrl Pts',(-0.379297306074508,-0.315371829026578,
-0.212556496120004));
#57491=CARTESIAN_POINT('Ctrl Pts',(-0.451780515904327,-0.228197926572105,
-0.218076279883216));
#57492=CARTESIAN_POINT('Ctrl Pts',(-0.491294321582725,-0.113613526924198,
-0.223596063646428));
#57493=CARTESIAN_POINT('Ctrl Pts',(-0.492199160006355,0.000404087486738508,
-0.229115847409641));
#57494=CARTESIAN_POINT('Ctrl Pts',(-0.492244893268066,0.000412969905903395,
-0.250884152590359));
#57495=CARTESIAN_POINT('Ctrl Pts',(-0.491298183331906,-0.115303633482406,
-0.245280795390601));
#57496=CARTESIAN_POINT('Ctrl Pts',(-0.450467838346037,-0.231622044558184,
-0.239677438190843));
#57497=CARTESIAN_POINT('Ctrl Pts',(-0.375962843028185,-0.319338025106157,
-0.234074080991085));
#57498=CARTESIAN_POINT('Ctrl Pts',(-0.271286702532588,-0.442575000887142,
-0.226201618171826));
#57499=CARTESIAN_POINT('Ctrl Pts',(-0.100140250512727,-0.509353707650003,
-0.218329155352567));
#57500=CARTESIAN_POINT('Ctrl Pts',(0.0603374458436118,-0.489575667285348,
-0.210456692533307));
#57501=CARTESIAN_POINT('Ctrl Pts',(0.220815142199958,-0.469797626920692,
-0.202584229714048));
#57502=CARTESIAN_POINT('Ctrl Pts',(0.370624082892782,-0.363462839428512,
-0.194711766894788));
#57503=CARTESIAN_POINT('Ctrl Pts',(0.442246704181642,-0.218498685373315,
-0.186839304075529));
#57504=CARTESIAN_POINT('Ctrl Pts',(0.513869325470499,-0.0735345313181219,
-0.178966841256269));
#57505=CARTESIAN_POINT('Ctrl Pts',(0.507305627355399,0.110058989300087,
-0.17109437843701));
#57506=CARTESIAN_POINT('Ctrl Pts',(0.425508298637621,0.249536520685491,
-0.163221915617751));
#57507=CARTESIAN_POINT('Ctrl Pts',(0.343710969919843,0.389014052070895,
-0.155349452798491));
#57508=CARTESIAN_POINT('Ctrl Pts',(0.186680010599389,0.484375594223496,
-0.147476989979232));
#57509=CARTESIAN_POINT('Ctrl Pts',(0.0252018055069099,0.492636420199208,
-0.139604527159972));
#57510=CARTESIAN_POINT('Ctrl Pts',(-0.136276399585572,0.50089724617492,
-0.131732064340713));
#57511=CARTESIAN_POINT('Ctrl Pts',(-0.302201850450079,0.422057355973741,
-0.123859601521453));
#57512=CARTESIAN_POINT('Ctrl Pts',(-0.39781102594903,0.291658920200447,
-0.115987138702194));
#57513=CARTESIAN_POINT('Ctrl Pts',(-0.458951742345601,0.20827096356799,
-0.110952809998249));
#57514=CARTESIAN_POINT('Ctrl Pts',(-0.491337168305235,0.103798543278651,
-0.105918481294304));
#57515=CARTESIAN_POINT('Ctrl Pts',(-0.491975623968706,-0.000315807630563663,
-0.100884152590359));
#57516=CARTESIAN_POINT('Origin',(0.,0.,-1.90478126690739));
#57517=CARTESIAN_POINT('',(-0.406714108344742,-0.000263120031215911,-0.0297812669073861));
#57518=CARTESIAN_POINT('',(-0.40704949043302,-3.9445486058054E-7,-0.000218733092610173));
#57519=CARTESIAN_POINT('',(-0.40705,-2.29167262861955E-14,-1.90478126690739));
#57520=CARTESIAN_POINT('',(-0.1293270056281,-0.385958842514677,0.));
#57521=CARTESIAN_POINT('Ctrl Pts',(-0.406714108344742,-0.000263120031215928,
-0.0297812669073861));
#57522=CARTESIAN_POINT('Ctrl Pts',(-0.407032085020554,-0.0473350676737868,
-0.0270267062286178));
#57523=CARTESIAN_POINT('Ctrl Pts',(-0.379781121781836,-0.216644350034151,
-0.0170996172594891));
#57524=CARTESIAN_POINT('Ctrl Pts',(-0.244382435473693,-0.347137952462494,
-0.00717252829036035));
#57525=CARTESIAN_POINT('Ctrl Pts',(-0.129150719006634,-0.38654594480115,
-6.28837260041593E-18));
#57526=CARTESIAN_POINT('',(-0.407032914766026,-0.00372944996920639,-2.22044604925031E-16));
#57527=CARTESIAN_POINT('Origin',(0.,0.,0.));
#57528=CARTESIAN_POINT('Ctrl Pts',(-0.40704949043302,-3.9445486056883E-7,
-0.000218733092610175));
#57529=CARTESIAN_POINT('Ctrl Pts',(-0.407049825054718,-0.00124330109335373,
-0.000145822061740043));
#57530=CARTESIAN_POINT('Ctrl Pts',(-0.407044304842328,-0.00248633476599664,
-7.29110308699103E-5));
#57531=CARTESIAN_POINT('Ctrl Pts',(-0.407032914766026,-0.00372944996921217,
2.22044604925031E-16));
#57532=CARTESIAN_POINT('Origin',(0.,0.,-1.90478126690739));
#57533=CARTESIAN_POINT('',(-0.406801356508805,0.000333977282159546,-0.179781266907386));
#57534=CARTESIAN_POINT('',(-0.406616604541039,-0.000261014205145876,-0.150218733092611));
#57535=CARTESIAN_POINT('',(-0.40705,-2.29167262861955E-14,-1.90478126690739));
#57536=CARTESIAN_POINT('Ctrl Pts',(-0.406801356508805,0.000333977282159493,
-0.179781266907386));
#57537=CARTESIAN_POINT('Ctrl Pts',(-0.406053509848213,-0.0939012916436638,
-0.174261483144174));
#57538=CARTESIAN_POINT('Ctrl Pts',(-0.32681765341167,-0.323673971963636,
-0.160869236561703));
#57539=CARTESIAN_POINT('Ctrl Pts',(0.053691564255565,-0.476763774871506,
-0.139604527159972));
#57540=CARTESIAN_POINT('Ctrl Pts',(0.427863587514561,-0.217018023145409,
-0.115987138702194));
#57541=CARTESIAN_POINT('Ctrl Pts',(0.416421643175193,0.238337106918288,
-0.0923697502444159));
#57542=CARTESIAN_POINT('Ctrl Pts',(0.0294708192559207,0.478879535587345,
-0.0687523617866379));
#57543=CARTESIAN_POINT('Ctrl Pts',(-0.335582261652634,0.309991567748977,
-0.0478895340076277));
#57544=CARTESIAN_POINT('Ctrl Pts',(-0.406123315946409,0.0871953351242249,
-0.0348991690478773));
#57545=CARTESIAN_POINT('Ctrl Pts',(-0.406714108344742,-0.000263120031215928,
-0.0297812669073861));
#57546=CARTESIAN_POINT('Ctrl Pts',(-0.406616604541039,-0.000261014205145928,
-0.150218733092611));
#57547=CARTESIAN_POINT('Ctrl Pts',(-0.406914088541965,-0.0487723759716419,
-0.147380598977297));
#57548=CARTESIAN_POINT('Ctrl Pts',(-0.376565976179168,-0.231490392209914,
-0.136670002042723));
#57549=CARTESIAN_POINT('Ctrl Pts',(-0.106905499254799,-0.467723490470255,
-0.118086942288891));
#57550=CARTESIAN_POINT('Ctrl Pts',(0.331923550485991,-0.346239581300314,
-0.0944695538311125));
#57551=CARTESIAN_POINT('Ctrl Pts',(0.472036117814807,0.0871616494771883,
-0.0708521653733347));
#57552=CARTESIAN_POINT('Ctrl Pts',(0.18569067875618,0.442363687480316,-0.0472347769155563));
#57553=CARTESIAN_POINT('Ctrl Pts',(-0.190742685458467,0.405446943649056,
-0.0275536198674078));
#57554=CARTESIAN_POINT('Ctrl Pts',(-0.37380969085203,0.198095302065577,
-0.0118816052597593));
#57555=CARTESIAN_POINT('Ctrl Pts',(-0.407031759908428,0.0658572197920024,
-0.00408205347136984));
#57556=CARTESIAN_POINT('Ctrl Pts',(-0.40704949043302,-3.9445486056883E-7,
-0.000218733092610175));
#57557=CARTESIAN_POINT('Origin',(0.,0.,-1.90478126690739));
#57558=CARTESIAN_POINT('',(-0.407646466546998,-0.000123197708628549,-0.329781266907387));
#57559=CARTESIAN_POINT('',(-0.406839154933536,0.000341318579049288,-0.300218733092611));
#57560=CARTESIAN_POINT('',(-0.40705,-2.29167262861955E-14,-1.90478126690739));
#57561=CARTESIAN_POINT('Ctrl Pts',(-0.407646466546998,-0.000123197708628555,
-0.329781266907387));
#57562=CARTESIAN_POINT('Ctrl Pts',(-0.407674703929589,-0.00712850667197845,
-0.329368722878991));
#57563=CARTESIAN_POINT('Ctrl Pts',(-0.404356705170022,-0.147786891764727,
-0.321083716031335));
#57564=CARTESIAN_POINT('Ctrl Pts',(-0.242405994059508,-0.414032097806954,
-0.30492624636442));
#57565=CARTESIAN_POINT('Ctrl Pts',(0.21282785627909,-0.429985628526655,
-0.281308857906642));
#57566=CARTESIAN_POINT('Ctrl Pts',(0.476213377687744,-0.0583407306117992,
-0.257691469448864));
#57567=CARTESIAN_POINT('Ctrl Pts',(0.310331352318132,0.365893451311033,
-0.234074080991085));
#57568=CARTESIAN_POINT('Ctrl Pts',(-0.135292724422396,0.460304007118841,
-0.210456692533307));
#57569=CARTESIAN_POINT('Ctrl Pts',(-0.383310271424921,0.214696131983949,
-0.192359087838741));
#57570=CARTESIAN_POINT('Ctrl Pts',(-0.407120108701099,0.0404995622132968,
-0.182133945963434));
#57571=CARTESIAN_POINT('Ctrl Pts',(-0.406801356508805,0.000333977282159493,
-0.179781266907386));
#57572=CARTESIAN_POINT('Ctrl Pts',(-0.406839154933536,0.000341318579049298,
-0.300218733092611));
#57573=CARTESIAN_POINT('Ctrl Pts',(-0.406056701574109,-0.0952981604244157,
-0.294615375892853));
#57574=CARTESIAN_POINT('Ctrl Pts',(-0.324898677082925,-0.326502977776057,
-0.281139555873836));
#57575=CARTESIAN_POINT('Ctrl Pts',(0.0586864453268738,-0.476171978247222,
-0.259791273035561));
#57576=CARTESIAN_POINT('Ctrl Pts',(0.430136573097502,-0.212515682316106,
-0.236173884577782));
#57577=CARTESIAN_POINT('Ctrl Pts',(0.413861933598501,0.242703054136536,
-0.212556496120004));
#57578=CARTESIAN_POINT('Ctrl Pts',(0.0245048656306335,0.479151271800793,
-0.188939107662225));
#57579=CARTESIAN_POINT('Ctrl Pts',(-0.337466212584372,0.30715981471096,
-0.168159853319762));
#57580=CARTESIAN_POINT('Ctrl Pts',(-0.406088922555631,0.0857892325717066,
-0.155253061796556));
#57581=CARTESIAN_POINT('Ctrl Pts',(-0.406616604541039,-0.000261014205145928,
-0.150218733092611));
#57582=CARTESIAN_POINT('Origin',(0.,0.,-1.90478126690739));
#57583=CARTESIAN_POINT('',(-0.406504802176995,-0.000194726252129646,-0.479781266907387));
#57584=CARTESIAN_POINT('',(-0.407626434063896,-0.000146564568675844,-0.450218733092611));
#57585=CARTESIAN_POINT('',(-0.40705,-2.29167262861955E-14,-1.90478126690739));
#57586=CARTESIAN_POINT('Ctrl Pts',(-0.406504802176995,-0.000194726252129608,
-0.479781266907387));
#57587=CARTESIAN_POINT('Ctrl Pts',(-0.406744024500403,-0.0545463867461071,
-0.476603499794547));
#57588=CARTESIAN_POINT('Ctrl Pts',(-0.371438645317141,-0.243248509798392,
-0.465553269862447));
#57589=CARTESIAN_POINT('Ctrl Pts',(-0.0869242056007438,-0.471834073964581,
-0.446630577111089));
#57590=CARTESIAN_POINT('Ctrl Pts',(0.346533251782296,-0.331810065779944,
-0.423013188653311));
#57591=CARTESIAN_POINT('Ctrl Pts',(0.467618186217581,0.1073146582275,-0.399395800195533));
#57592=CARTESIAN_POINT('Ctrl Pts',(0.167182082036718,0.449703640764164,
-0.375778411737755));
#57593=CARTESIAN_POINT('Ctrl Pts',(-0.276075204840169,0.387820308034648,
-0.352573567308372));
#57594=CARTESIAN_POINT('Ctrl Pts',(-0.407135857820417,0.126551853617785,
-0.33724118569825));
#57595=CARTESIAN_POINT('Ctrl Pts',(-0.407646466546998,-0.000123197708628555,
-0.329781266907387));
#57596=CARTESIAN_POINT('Ctrl Pts',(-0.407626434063896,-0.000146564568675865,
-0.450218733092611));
#57597=CARTESIAN_POINT('Ctrl Pts',(-0.407665958859733,-0.00857211527255664,
-0.449722615627669));
#57598=CARTESIAN_POINT('Ctrl Pts',(-0.403634411612907,-0.150656998330975,
-0.441354035343468));
#57599=CARTESIAN_POINT('Ctrl Pts',(-0.238044360971215,-0.416554973675746,
-0.425112992240007));
#57600=CARTESIAN_POINT('Ctrl Pts',(0.217331606272519,-0.427726730571028,
-0.40149560378223));
#57601=CARTESIAN_POINT('Ctrl Pts',(0.476800102102078,-0.0533363964720061,
-0.377878215324451));
#57602=CARTESIAN_POINT('Ctrl Pts',(0.306470944705725,0.369132435561808,
-0.354260826866673));
#57603=CARTESIAN_POINT('Ctrl Pts',(-0.140118061818574,0.458857512735786,
-0.330643438408895));
#57604=CARTESIAN_POINT('Ctrl Pts',(-0.38441204095114,0.211805201682357,
-0.312629407150874));
#57605=CARTESIAN_POINT('Ctrl Pts',(-0.407156013069039,0.039070971449013,
-0.302487838712113));
#57606=CARTESIAN_POINT('Ctrl Pts',(-0.406839154933536,0.000341318579049298,
-0.300218733092611));
#57607=CARTESIAN_POINT('Origin',(0.,0.,-1.90478126690739));
#57608=CARTESIAN_POINT('',(-0.407002844200305,0.000356182830250053,-0.629781266907387));
#57609=CARTESIAN_POINT('',(-0.406484904749669,-0.000175274386724683,-0.600218733092611));
#57610=CARTESIAN_POINT('',(-0.40705,-2.29167262861955E-14,-1.90478126690739));
#57611=CARTESIAN_POINT('Ctrl Pts',(-0.407002844200305,0.000356182830250049,
-0.629781266907387));
#57612=CARTESIAN_POINT('Ctrl Pts',(-0.406106728250001,-0.100976338795125,
-0.623838276710104));
#57613=CARTESIAN_POINT('Ctrl Pts',(-0.316870064410776,-0.337949636189232,
-0.61002282369356));
#57614=CARTESIAN_POINT('Ctrl Pts',(0.0789482169998913,-0.473233969566154,
-0.588334907857759));
#57615=CARTESIAN_POINT('Ctrl Pts',(0.438814986437033,-0.193970664507679,
-0.56471751939998));
#57616=CARTESIAN_POINT('Ctrl Pts',(0.40312451145329,0.260141959498729,-0.541100130942203));
#57617=CARTESIAN_POINT('Ctrl Pts',(0.00404895281978514,0.479757039402292,
-0.517482742484423));
#57618=CARTESIAN_POINT('Ctrl Pts',(-0.344488911026044,0.295547984959571,
-0.497043121139486));
#57619=CARTESIAN_POINT('Ctrl Pts',(-0.40615138546183,0.0801020664633769,
-0.484475962613807));
#57620=CARTESIAN_POINT('Ctrl Pts',(-0.406504802176995,-0.000194726252129608,
-0.479781266907387));
#57621=CARTESIAN_POINT('Ctrl Pts',(-0.406484904749669,-0.000175274386724725,
-0.600218733092611));
#57622=CARTESIAN_POINT('Ctrl Pts',(-0.406705235629013,-0.0559631820000021,
-0.596957392543226));
#57623=CARTESIAN_POINT('Ctrl Pts',(-0.370130649226088,-0.246139588399615,
-0.585823589174581));
#57624=CARTESIAN_POINT('Ctrl Pts',(-0.0819642213078552,-0.472720877576032,
-0.566817322986677));
#57625=CARTESIAN_POINT('Ctrl Pts',(0.349998754832881,-0.328152455226764,
-0.543199934528899));
#57626=CARTESIAN_POINT('Ctrl Pts',(0.466465341731633,0.112219631976251,
-0.51958254607112));
#57627=CARTESIAN_POINT('Ctrl Pts',(0.162450064697528,0.451434533625857,
-0.495965157613343));
#57628=CARTESIAN_POINT('Ctrl Pts',(-0.278538812073554,0.385139175342376,
-0.472843886620505));
#57629=CARTESIAN_POINT('Ctrl Pts',(-0.407038773752055,0.125125727144453,
-0.457595078446929));
#57630=CARTESIAN_POINT('Ctrl Pts',(-0.407626434063896,-0.000146564568675865,
-0.450218733092611));
#57631=CARTESIAN_POINT('Origin',(0.,0.,-1.90478126690739));
#57632=CARTESIAN_POINT('',(-0.407517210131742,-0.000231984110039767,-0.779781266907388));
#57633=CARTESIAN_POINT('',(-0.407044529006025,0.000355972576201596,-0.750218733092611));
#57634=CARTESIAN_POINT('',(-0.40705,-2.29167262861955E-14,-1.90478126690739));
#57635=CARTESIAN_POINT('Ctrl Pts',(-0.407517210131742,-0.000231984110039793,
-0.779781266907388));
#57636=CARTESIAN_POINT('Ctrl Pts',(-0.407614613871175,-0.0144355929662029,
-0.77894551644492));
#57637=CARTESIAN_POINT('Ctrl Pts',(-0.400535787639923,-0.16233387099766,
-0.770237303163193));
#57638=CARTESIAN_POINT('Ctrl Pts',(-0.220054620371515,-0.42633223545369,
-0.753656627062206));
#57639=CARTESIAN_POINT('Ctrl Pts',(0.235383332820519,-0.418064465798881,
-0.730039238604428));
#57640=CARTESIAN_POINT('Ctrl Pts',(0.478641699347353,-0.0329444165423497,
-0.70642185014665));
#57641=CARTESIAN_POINT('Ctrl Pts',(0.290442168180321,0.381872436653063,
-0.682804461688872));
#57642=CARTESIAN_POINT('Ctrl Pts',(-0.159568165198072,0.452461281864222,
-0.659187073231093));
#57643=CARTESIAN_POINT('Ctrl Pts',(-0.388696326414372,0.200061029798759,
-0.641512674970599));
#57644=CARTESIAN_POINT('Ctrl Pts',(-0.407293780435236,0.0332551646056748,
-0.631710739529363));
#57645=CARTESIAN_POINT('Ctrl Pts',(-0.407002844200305,0.000356182830250049,
-0.629781266907387));
#57646=CARTESIAN_POINT('Ctrl Pts',(-0.407044529006025,0.000355972576201576,
-0.750218733092611));
#57647=CARTESIAN_POINT('Ctrl Pts',(-0.406127620987465,-0.102374557696288,
-0.744192169458782));
#57648=CARTESIAN_POINT('Ctrl Pts',(-0.314834083697359,-0.340753452688454,
-0.730293143005694));
#57649=CARTESIAN_POINT('Ctrl Pts',(0.0839137360252065,-0.472378711028833,
-0.708521653733346));
#57650=CARTESIAN_POINT('Ctrl Pts',(0.440827811035869,-0.189351532231765,
-0.684904265275568));
#57651=CARTESIAN_POINT('Ctrl Pts',(0.400370238591211,0.264361180523987,
-0.66128687681779));
#57652=CARTESIAN_POINT('Ctrl Pts',(-0.000989657323522311,0.479773052904378,
-0.637669488360011));
#57653=CARTESIAN_POINT('Ctrl Pts',(-0.346156596104652,0.292681966063216,
-0.617313440451619));
#57654=CARTESIAN_POINT('Ctrl Pts',(-0.406173384805922,0.0787017577078716,
-0.604829855362485));
#57655=CARTESIAN_POINT('Ctrl Pts',(-0.406484904749669,-0.000175274386724725,
-0.600218733092611));
#57656=CARTESIAN_POINT('Origin',(0.,0.,-1.90478126690739));
#57657=CARTESIAN_POINT('',(-0.406427115799581,-8.9948673345385E-5,-0.929781266907387));
#57658=CARTESIAN_POINT('',(-0.407484518933728,-0.00025017497073776,-0.900218733092611));
#57659=CARTESIAN_POINT('',(-0.40705,-2.29167262861955E-14,-1.90478126690739));
#57660=CARTESIAN_POINT('Ctrl Pts',(-0.406427115799581,-8.99486733453581E-5,
-0.929781266907387));
#57661=CARTESIAN_POINT('Ctrl Pts',(-0.406550907978516,-0.0617095280149024,
-0.926180293360476));
#57662=CARTESIAN_POINT('Ctrl Pts',(-0.364609160678107,-0.257882177620295,
-0.914706856994306));
#57663=CARTESIAN_POINT('Ctrl Pts',(-0.0617202026280809,-0.475787586555369,
-0.895360957808874));
#57664=CARTESIAN_POINT('Ctrl Pts',(0.363681217312252,-0.31292041018399,
-0.871743569351098));
#57665=CARTESIAN_POINT('Ctrl Pts',(0.461252584696539,0.132019938055431,
-0.848126180893318));
#57666=CARTESIAN_POINT('Ctrl Pts',(0.14304097544786,0.4579546814661,-0.824508792435541));
#57667=CARTESIAN_POINT('Ctrl Pts',(-0.288287440300272,0.374153517030152,
-0.80172715444023));
#57668=CARTESIAN_POINT('Ctrl Pts',(-0.406697106371536,0.119357192848475,
-0.786817979264179));
#57669=CARTESIAN_POINT('Ctrl Pts',(-0.407517210131742,-0.000231984110039793,
-0.779781266907388));
#57670=CARTESIAN_POINT('Ctrl Pts',(-0.407484518933728,-0.000250174970737722,
-0.900218733092611));
#57671=CARTESIAN_POINT('Ctrl Pts',(-0.407598097974698,-0.0158774087335492,
-0.899299409193598));
#57672=CARTESIAN_POINT('Ctrl Pts',(-0.399732457373963,-0.16521027632643,
-0.890507622475326));
#57673=CARTESIAN_POINT('Ctrl Pts',(-0.215565140139133,-0.428619682337017,
-0.873843372937795));
#57674=CARTESIAN_POINT('Ctrl Pts',(0.239760820588477,-0.415569381260058,
-0.850225984480015));
#57675=CARTESIAN_POINT('Ctrl Pts',(0.478961233248966,-0.0279159233190857,
-0.826608596022238));
#57676=CARTESIAN_POINT('Ctrl Pts',(0.286415713505782,0.384901546875125,
-0.802991207564458));
#57677=CARTESIAN_POINT('Ctrl Pts',(-0.164311075821679,0.450760504139189,
-0.779373819106682));
#57678=CARTESIAN_POINT('Ctrl Pts',(-0.389705041663024,0.197172692304488,
-0.761782994282732));
#57679=CARTESIAN_POINT('Ctrl Pts',(-0.407325372263877,0.0318216989288424,
-0.752064632278042));
#57680=CARTESIAN_POINT('Ctrl Pts',(-0.407044529006025,0.000355972576201576,
-0.750218733092611));
#57681=CARTESIAN_POINT('Origin',(0.,0.,-1.90478126690739));
#57682=CARTESIAN_POINT('',(-0.407215026014371,0.000338947040179602,-1.07978126690739));
#57683=CARTESIAN_POINT('',(-0.406418685883609,-6.78377527379426E-5,-1.05021873309261));
#57684=CARTESIAN_POINT('',(-0.40705,-2.29167262861955E-14,-1.90478126690739));
#57685=CARTESIAN_POINT('Ctrl Pts',(-0.407215026014371,0.000338947040179598,
-1.07978126690739));
#57686=CARTESIAN_POINT('Ctrl Pts',(-0.40625104068007,-0.108064226981459,
-1.07341507027603));
#57687=CARTESIAN_POINT('Ctrl Pts',(-0.306311001088235,-0.352090017898099,
-1.05917641082542));
#57688=CARTESIAN_POINT('Ctrl Pts',(0.103992118918514,-0.468368284610657,
-1.03706528855554));
#57689=CARTESIAN_POINT('Ctrl Pts',(0.448505409809192,-0.170370503266186,
-1.01344790009777));
#57690=CARTESIAN_POINT('Ctrl Pts',(0.388726300769665,0.281202905405924,
-0.989830511639989));
#57691=CARTESIAN_POINT('Ctrl Pts',(-0.0214590362974804,0.479293981479854,
-0.96621312318221));
#57692=CARTESIAN_POINT('Ctrl Pts',(-0.35270860156304,0.281010568000828,
-0.946196708271343));
#57693=CARTESIAN_POINT('Ctrl Pts',(-0.40628027302014,0.0730034436260336,
-0.934052756179736));
#57694=CARTESIAN_POINT('Ctrl Pts',(-0.406427115799581,-8.99486733453581E-5,
-0.929781266907387));
#57695=CARTESIAN_POINT('Ctrl Pts',(-0.406418685883609,-6.78377527379634E-5,
-1.05021873309261));
#57696=CARTESIAN_POINT('Ctrl Pts',(-0.406514099565618,-0.0631207687989047,
-1.04653418610915));
#57697=CARTESIAN_POINT('Ctrl Pts',(-0.36319902856371,-0.260769488780026,
-1.03497717630644));
#57698=CARTESIAN_POINT('Ctrl Pts',(-0.0567200932042535,-0.476409480116128,
-1.01554770368446));
#57699=CARTESIAN_POINT('Ctrl Pts',(0.366947398132722,-0.309083756844029,
-0.991930315226685));
#57700=CARTESIAN_POINT('Ctrl Pts',(0.459840631415877,0.136856696679471,
-0.968312926768907));
#57701=CARTESIAN_POINT('Ctrl Pts',(0.138223653062154,0.459431587358633,
-0.944695538311129));
#57702=CARTESIAN_POINT('Ctrl Pts',(-0.290621860797603,0.371429283499432,
-0.921997473752364));
#57703=CARTESIAN_POINT('Ctrl Pts',(-0.40662548453775,0.11794356219702,-0.907171872012857));
#57704=CARTESIAN_POINT('Ctrl Pts',(-0.407484518933728,-0.000250174970737722,
-0.900218733092611));
#57705=CARTESIAN_POINT('Origin',(0.,0.,-1.90478126690739));
#57706=CARTESIAN_POINT('',(-0.407335136724506,-0.000310347641450006,-1.22978126690739));
#57707=CARTESIAN_POINT('',(-0.407256252750017,0.00033078647732554,-1.20021873309261));
#57708=CARTESIAN_POINT('',(-0.40705,-2.29167262861955E-14,-1.90478126690739));
#57709=CARTESIAN_POINT('Ctrl Pts',(-0.407335136724506,-0.000310347641449972,
-1.22978126690739));
#57710=CARTESIAN_POINT('Ctrl Pts',(-0.407516487490046,-0.0217313980275844,
-1.22852231001085));
#57711=CARTESIAN_POINT('Ctrl Pts',(-0.3962986870886,-0.176911566770959,
-1.21939089029505));
#57712=CARTESIAN_POINT('Ctrl Pts',(-0.19708110914224,-0.437426850444666,
-1.20238700775999));
#57713=CARTESIAN_POINT('Ctrl Pts',(0.257273433552846,-0.404961213377078,
-1.17876961930221));
#57714=CARTESIAN_POINT('Ctrl Pts',(0.47971620707788,-0.00745486488903116,
-1.15515223084444));
#57715=CARTESIAN_POINT('Ctrl Pts',(0.269732486126293,0.396771466717889,
-1.13153484238666));
#57716=CARTESIAN_POINT('Ctrl Pts',(-0.183393878810481,0.443339480829272,
-1.10791745392888));
#57717=CARTESIAN_POINT('Ctrl Pts',(-0.393623984240889,0.185443113339493,
-1.09066626210246));
#57718=CARTESIAN_POINT('Ctrl Pts',(-0.407443108588437,0.0259875477896631,
-1.08128753309529));
#57719=CARTESIAN_POINT('Ctrl Pts',(-0.407215026014371,0.000338947040179598,
-1.07978126690739));
#57720=CARTESIAN_POINT('Ctrl Pts',(-0.407256252750017,0.00033078647732554,
-1.20021873309261));
#57721=CARTESIAN_POINT('Ctrl Pts',(-0.406291321061865,-0.10946667159376,
-1.19376896302471));
#57722=CARTESIAN_POINT('Ctrl Pts',(-0.304151795041626,-0.354864242487783,
-1.17944673013755));
#57723=CARTESIAN_POINT('Ctrl Pts',(0.108905154226429,-0.467250284345138,
-1.15725203443113));
#57724=CARTESIAN_POINT('Ctrl Pts',(0.450269851614892,-0.165650906977965,
-1.13363464597335));
#57725=CARTESIAN_POINT('Ctrl Pts',(0.385751642062305,0.285269753596648,
-1.11001725751558));
#57726=CARTESIAN_POINT('Ctrl Pts',(-0.0264913736532199,0.479042136709866,
-1.0863998690578));
#57727=CARTESIAN_POINT('Ctrl Pts',(-0.354265995702489,0.278133272522654,
-1.06646702758348));
#57728=CARTESIAN_POINT('Ctrl Pts',(-0.406310237145777,0.0715991458975248,
-1.05440664892841));
#57729=CARTESIAN_POINT('Ctrl Pts',(-0.406418685883609,-6.78377527379634E-5,
-1.05021873309261));
#57730=CARTESIAN_POINT('Origin',(0.,0.,-1.90478126690739));
#57731=CARTESIAN_POINT('',(-0.406408689871578,2.35123281448032E-5,-1.37978126690739));
#57732=CARTESIAN_POINT('',(-0.407295256592268,-0.000321495865622912,-1.35021873309261));
#57733=CARTESIAN_POINT('',(-0.40705,-2.29167262861955E-14,-1.90478126690739));
#57734=CARTESIAN_POINT('Ctrl Pts',(-0.406408689871578,2.35123281448202E-5,
-1.37978126690739));
#57735=CARTESIAN_POINT('Ctrl Pts',(-0.406372411151293,-0.0688453689981078,
-1.37575708692641));
#57736=CARTESIAN_POINT('Ctrl Pts',(-0.357256431910931,-0.272490465756646,
-1.36386044412616));
#57737=CARTESIAN_POINT('Ctrl Pts',(-0.0363410200831963,-0.478396170765624,
-1.34409133850666));
#57738=CARTESIAN_POINT('Ctrl Pts',(0.379800489517723,-0.293145714789055,
-1.32047395004888));
#57739=CARTESIAN_POINT('Ctrl Pts',(0.453582904114614,0.156351802812663,
-1.2968565615911));
#57740=CARTESIAN_POINT('Ctrl Pts',(0.118495324937651,0.464910853754055,
-1.27323917313333));
#57741=CARTESIAN_POINT('Ctrl Pts',(-0.299849997018574,0.360280589402105,
-1.25088074157209));
#57742=CARTESIAN_POINT('Ctrl Pts',(-0.40638247157347,0.112217923969001,
-1.23639477283011));
#57743=CARTESIAN_POINT('Ctrl Pts',(-0.407335136724506,-0.000310347641449972,
-1.22978126690739));
#57744=CARTESIAN_POINT('Ctrl Pts',(-0.407295256592268,-0.000321495865622943,
-1.35021873309261));
#57745=CARTESIAN_POINT('Ctrl Pts',(-0.407492918321581,-0.0231703370026054,
-1.34887620275953));
#57746=CARTESIAN_POINT('Ctrl Pts',(-0.395411489547801,-0.179793560026876,
-1.33966120960718));
#57747=CARTESIAN_POINT('Ctrl Pts',(-0.192476314157182,-0.439472483121615,
-1.32257375363558));
#57748=CARTESIAN_POINT('Ctrl Pts',(0.26151206617616,-0.402236929927433,
-1.2989563651778));
#57749=CARTESIAN_POINT('Ctrl Pts',(0.479768010181106,-0.00241651336352132,
-1.27533897672002));
#57750=CARTESIAN_POINT('Ctrl Pts',(0.265550697114187,0.399582270810862,
-1.25172158826225));
#57751=CARTESIAN_POINT('Ctrl Pts',(-0.188039671187417,0.44138898578519,
-1.22810419980447));
#57752=CARTESIAN_POINT('Ctrl Pts',(-0.394544467466406,0.182559052872597,
-1.21093658141459));
#57753=CARTESIAN_POINT('Ctrl Pts',(-0.407469097751286,0.0245499518228972,
-1.20164142584397));
#57754=CARTESIAN_POINT('Ctrl Pts',(-0.407256252750017,0.00033078647732554,
-1.20021873309261));
#57755=CARTESIAN_POINT('Origin',(0.,0.,-1.90478126690739));
#57756=CARTESIAN_POINT('',(-0.407376298364278,0.000257087447545755,-1.52978126690739));
#57757=CARTESIAN_POINT('',(-0.406409642899809,4.34815695103397E-5,-1.50021873309261));
#57758=CARTESIAN_POINT('',(-0.40705,-2.29167262861955E-14,-1.90478126690739));
#57759=CARTESIAN_POINT('Ctrl Pts',(-0.407376298364278,0.00025708744754576,
-1.52978126690739));
#57760=CARTESIAN_POINT('Ctrl Pts',(-0.406454140896361,-0.115208344033967,
-1.52299186384196));
#57761=CARTESIAN_POINT('Ctrl Pts',(-0.295182303803987,-0.366031497986206,
-1.50832999795728));
#57762=CARTESIAN_POINT('Ctrl Pts',(0.128775427374938,-0.462199578908625,
-1.48579566925333));
#57763=CARTESIAN_POINT('Ctrl Pts',(0.456910236919244,-0.146277500967067,
-1.46217828079555));
#57764=CARTESIAN_POINT('Ctrl Pts',(0.373237957669861,0.301462946406964,
-1.43856089233778));
#57765=CARTESIAN_POINT('Ctrl Pts',(-0.046911046254029,0.477478658159383,
-1.41494350387999));
#57766=CARTESIAN_POINT('Ctrl Pts',(-0.360375435904293,0.266422351665797,
-1.3953502954032));
#57767=CARTESIAN_POINT('Ctrl Pts',(-0.406443382846875,0.0658821308172752,
-1.38362954974566));
#57768=CARTESIAN_POINT('Ctrl Pts',(-0.406408689871578,2.35123281448202E-5,
-1.37978126690739));
#57769=CARTESIAN_POINT('Ctrl Pts',(-0.406409642899809,4.34815695103258E-5,
-1.50021873309261));
#57770=CARTESIAN_POINT('Ctrl Pts',(-0.406338718852544,-0.0702526545189025,
-1.49611097967508));
#57771=CARTESIAN_POINT('Ctrl Pts',(-0.355745821427167,-0.275366303807096,
-1.4841307634383));
#57772=CARTESIAN_POINT('Ctrl Pts',(-0.0313114294066901,-0.478754704371251,
-1.46427808438225));
#57773=CARTESIAN_POINT('Ctrl Pts',(0.382856292689895,-0.28913914624985,
-1.44066069592447));
#57774=CARTESIAN_POINT('Ctrl Pts',(0.451916785881922,0.161105773860312,
-1.41704330746669));
#57775=CARTESIAN_POINT('Ctrl Pts',(0.113605814801219,0.466130064220589,
-1.39342591900891));
#57776=CARTESIAN_POINT('Ctrl Pts',(-0.302057329836814,0.357518966974991,
-1.37115106088422));
#57777=CARTESIAN_POINT('Ctrl Pts',(-0.406333849824981,0.110812968909595,
-1.35674866557879));
#57778=CARTESIAN_POINT('Ctrl Pts',(-0.407295256592268,-0.000321495865622943,
-1.35021873309261));
#57779=CARTESIAN_POINT('Origin',(0.,0.,2.85));
#57780=CARTESIAN_POINT('',(-9.49101269339199E-17,-0.458257569495584,1.3));
#57781=CARTESIAN_POINT('',(-1.53080849893419E-16,-6.12323399573677E-17,
1.6));
#57782=CARTESIAN_POINT('Origin',(-2.14313189850787E-16,0.,1.1));
#57783=CARTESIAN_POINT('',(0.367006645104718,-0.474664220738176,1.3));
#57784=CARTESIAN_POINT('Ctrl Pts',(0.367006645104718,-0.474664220738176,
1.3));
#57785=CARTESIAN_POINT('Ctrl Pts',(0.338138729685014,-0.47246220371005,
1.3));
#57786=CARTESIAN_POINT('Ctrl Pts',(0.309024935784566,-0.470333761200034,
1.3));
#57787=CARTESIAN_POINT('Ctrl Pts',(0.183814615587507,-0.462023903676248,
1.3));
#57788=CARTESIAN_POINT('Ctrl Pts',(0.0876016538044517,-0.458257569495584,
1.3));
#57789=CARTESIAN_POINT('Ctrl Pts',(0.,-0.458257569495584,1.3));
#57790=CARTESIAN_POINT('',(0.827500847770699,-0.194273896699414,0.8));
#57791=CARTESIAN_POINT('Ctrl Pts',(0.827500847770699,-0.194273896699415,
0.8));
#57792=CARTESIAN_POINT('Ctrl Pts',(0.806825653221766,-0.247573683077793,
0.815891726644921));
#57793=CARTESIAN_POINT('Ctrl Pts',(0.77844058049192,-0.295313715449721,
0.837983964638171));
#57794=CARTESIAN_POINT('Ctrl Pts',(0.70695573897281,-0.382945194539716,
0.896201780082199));
#57795=CARTESIAN_POINT('Ctrl Pts',(0.66279406000339,-0.420213839249111,
0.933475334456469));
#57796=CARTESIAN_POINT('Ctrl Pts',(0.568627272529482,-0.476124483335569,
1.02033912838166));
#57797=CARTESIAN_POINT('Ctrl Pts',(0.520183006714955,-0.492461401650283,
1.06898944325634));
#57798=CARTESIAN_POINT('Ctrl Pts',(0.448389981387326,-0.501794096344547,
1.15498482706113));
#57799=CARTESIAN_POINT('Ctrl Pts',(0.420349703511602,-0.500357460127172,
1.19326140983976));
#57800=CARTESIAN_POINT('Ctrl Pts',(0.385715038223485,-0.488539976457829,
1.25517036827747));
#57801=CARTESIAN_POINT('Ctrl Pts',(0.375253631229262,-0.482576530120786,
1.27739203707623));
#57802=CARTESIAN_POINT('Ctrl Pts',(0.367006645104718,-0.474664220738176,
1.3));
#57803=CARTESIAN_POINT('',(0.827500847770699,0.194273896699414,0.8));
#57804=CARTESIAN_POINT('Ctrl Pts',(0.827500847770699,0.194273896699414,
0.8));
#57805=CARTESIAN_POINT('Ctrl Pts',(0.832240686457716,0.190066469416246,
0.8));
#57806=CARTESIAN_POINT('Ctrl Pts',(0.83681804160594,0.185810667739891,0.8));
#57807=CARTESIAN_POINT('Ctrl Pts',(0.86737452556169,0.15603927066178,0.8));
#57808=CARTESIAN_POINT('Ctrl Pts',(0.893751654888157,0.121036696804236,
0.8));
#57809=CARTESIAN_POINT('Ctrl Pts',(0.919853574042595,0.0616080446153948,
0.8));
#57810=CARTESIAN_POINT('Ctrl Pts',(0.92736184954957,0.0283844942503903,
0.8));
#57811=CARTESIAN_POINT('Ctrl Pts',(0.92736184954957,-0.0283844942503903,
0.8));
#57812=CARTESIAN_POINT('Ctrl Pts',(0.919853574042595,-0.0616080446153948,
0.8));
#57813=CARTESIAN_POINT('Ctrl Pts',(0.893751654888157,-0.121036696804236,
0.8));
#57814=CARTESIAN_POINT('Ctrl Pts',(0.86737452556169,-0.15603927066178,0.8));
#57815=CARTESIAN_POINT('Ctrl Pts',(0.83681804160594,-0.185810667739891,
0.8));
#57816=CARTESIAN_POINT('Ctrl Pts',(0.832240686457716,-0.190066469416246,
0.8));
#57817=CARTESIAN_POINT('Ctrl Pts',(0.827500847770699,-0.194273896699414,
0.8));
#57818=CARTESIAN_POINT('',(0.367006645104718,0.474664220738176,1.3));
#57819=CARTESIAN_POINT('Ctrl Pts',(0.367006645104718,0.474664220738176,
1.3));
#57820=CARTESIAN_POINT('Ctrl Pts',(0.386844565037868,0.49369708409554,1.24561710768513));
#57821=CARTESIAN_POINT('Ctrl Pts',(0.416544185701006,0.498879203778029,
1.20057273466721));
#57822=CARTESIAN_POINT('Ctrl Pts',(0.471907063756615,0.501218135446952,
1.12399758848168));
#57823=CARTESIAN_POINT('Ctrl Pts',(0.51158524080212,0.49437132413065,1.07934345321278));
#57824=CARTESIAN_POINT('Ctrl Pts',(0.6046391383893,0.458711546216609,0.985187921540669));
#57825=CARTESIAN_POINT('Ctrl Pts',(0.657180998804381,0.425900587285382,
0.938631347135963));
#57826=CARTESIAN_POINT('Ctrl Pts',(0.728744413965246,0.357037429469063,
0.878319677166941));
#57827=CARTESIAN_POINT('Ctrl Pts',(0.751978600292447,0.32968521463109,0.859423759568972));
#57828=CARTESIAN_POINT('Ctrl Pts',(0.794210469526027,0.267260154796302,
0.825735732037567));
#57829=CARTESIAN_POINT('Ctrl Pts',(0.812815008506796,0.232133375781979,
0.811288084500528));
#57830=CARTESIAN_POINT('Ctrl Pts',(0.827500847770699,0.194273896699415,
0.8));
#57831=CARTESIAN_POINT('',(-6.7154551318291E-17,0.458257569495584,1.3));
#57832=CARTESIAN_POINT('Ctrl Pts',(5.55111512312578E-17,0.458257569495584,
1.3));
#57833=CARTESIAN_POINT('Ctrl Pts',(0.0876016538044517,0.458257569495584,
1.3));
#57834=CARTESIAN_POINT('Ctrl Pts',(0.183814615587507,0.462023903676248,
1.3));
#57835=CARTESIAN_POINT('Ctrl Pts',(0.309024935784565,0.470333761200034,
1.3));
#57836=CARTESIAN_POINT('Ctrl Pts',(0.338138729685014,0.47246220371005,1.3));
#57837=CARTESIAN_POINT('Ctrl Pts',(0.367006645104718,0.474664220738176,
1.3));
#57838=CARTESIAN_POINT('Origin',(-2.14313189850787E-16,0.,1.1));
#57839=CARTESIAN_POINT('Origin',(0.,-6.12323399573677E-17,2.85));
#57840=CARTESIAN_POINT('',(-0.367006645104718,0.474664220738176,1.3));
#57841=CARTESIAN_POINT('Ctrl Pts',(-0.367006645104718,0.474664220738176,
1.3));
#57842=CARTESIAN_POINT('Ctrl Pts',(-0.338138729685014,0.47246220371005,
1.3));
#57843=CARTESIAN_POINT('Ctrl Pts',(-0.309024935784565,0.470333761200034,
1.3));
#57844=CARTESIAN_POINT('Ctrl Pts',(-0.183814615587506,0.462023903676248,
1.3));
#57845=CARTESIAN_POINT('Ctrl Pts',(-0.0876016538044515,0.458257569495584,
1.3));
#57846=CARTESIAN_POINT('Ctrl Pts',(5.55111512312578E-17,0.458257569495584,
1.3));
#57847=CARTESIAN_POINT('',(-0.827500847770699,0.194273896699414,0.8));
#57848=CARTESIAN_POINT('Ctrl Pts',(-0.827500847770699,0.194273896699414,
0.8));
#57849=CARTESIAN_POINT('Ctrl Pts',(-0.806825653221767,0.247573683077793,
0.815891726644921));
#57850=CARTESIAN_POINT('Ctrl Pts',(-0.77844058049192,0.295313715449721,
0.837983964638171));
#57851=CARTESIAN_POINT('Ctrl Pts',(-0.706955738972811,0.382945194539717,
0.896201780082199));
#57852=CARTESIAN_POINT('Ctrl Pts',(-0.66279406000339,0.420213839249111,
0.933475334456469));
#57853=CARTESIAN_POINT('Ctrl Pts',(-0.56862727252948,0.476124483335571,
1.02033912838166));
#57854=CARTESIAN_POINT('Ctrl Pts',(-0.520183006714953,0.492461401650283,
1.06898944325634));
#57855=CARTESIAN_POINT('Ctrl Pts',(-0.448389981387328,0.501794096344547,
1.15498482706113));
#57856=CARTESIAN_POINT('Ctrl Pts',(-0.420349703511603,0.500357460127172,
1.19326140983976));
#57857=CARTESIAN_POINT('Ctrl Pts',(-0.385715038223483,0.488539976457828,
1.25517036827748));
#57858=CARTESIAN_POINT('Ctrl Pts',(-0.375253631229262,0.482576530120786,
1.27739203707623));
#57859=CARTESIAN_POINT('Ctrl Pts',(-0.367006645104718,0.474664220738176,
1.3));
#57860=CARTESIAN_POINT('',(-0.827500847770699,-0.194273896699414,0.8));
#57861=CARTESIAN_POINT('Ctrl Pts',(-0.827500847770699,-0.194273896699414,
0.8));
#57862=CARTESIAN_POINT('Ctrl Pts',(-0.832240686457716,-0.190066469416245,
0.8));
#57863=CARTESIAN_POINT('Ctrl Pts',(-0.83681804160594,-0.185810667739891,
0.8));
#57864=CARTESIAN_POINT('Ctrl Pts',(-0.86737452556169,-0.15603927066178,
0.8));
#57865=CARTESIAN_POINT('Ctrl Pts',(-0.893751654888157,-0.121036696804236,
0.8));
#57866=CARTESIAN_POINT('Ctrl Pts',(-0.919853574042595,-0.0616080446153948,
0.8));
#57867=CARTESIAN_POINT('Ctrl Pts',(-0.92736184954957,-0.0283844942503903,
0.8));
#57868=CARTESIAN_POINT('Ctrl Pts',(-0.92736184954957,0.0283844942503903,
0.8));
#57869=CARTESIAN_POINT('Ctrl Pts',(-0.919853574042595,0.0616080446153948,
0.8));
#57870=CARTESIAN_POINT('Ctrl Pts',(-0.893751654888157,0.121036696804236,
0.8));
#57871=CARTESIAN_POINT('Ctrl Pts',(-0.86737452556169,0.15603927066178,0.8));
#57872=CARTESIAN_POINT('Ctrl Pts',(-0.83681804160594,0.185810667739891,
0.8));
#57873=CARTESIAN_POINT('Ctrl Pts',(-0.832240686457716,0.190066469416246,
0.8));
#57874=CARTESIAN_POINT('Ctrl Pts',(-0.827500847770699,0.194273896699414,
0.8));
#57875=CARTESIAN_POINT('',(-0.367006645104718,-0.474664220738176,1.3));
#57876=CARTESIAN_POINT('Ctrl Pts',(-0.367006645104718,-0.474664220738176,
1.3));
#57877=CARTESIAN_POINT('Ctrl Pts',(-0.386844565037811,-0.493697084095486,
1.24561710768529));
#57878=CARTESIAN_POINT('Ctrl Pts',(-0.416544185700876,-0.498879203778024,
1.20057273466739));
#57879=CARTESIAN_POINT('Ctrl Pts',(-0.471907063756621,-0.501218135446952,
1.12399758848167));
#57880=CARTESIAN_POINT('Ctrl Pts',(-0.511585240802128,-0.494371324130647,
1.07934345321277));
#57881=CARTESIAN_POINT('Ctrl Pts',(-0.6046391383893,-0.458711546216609,
0.98518792154067));
#57882=CARTESIAN_POINT('Ctrl Pts',(-0.657180998804382,-0.425900587285382,
0.938631347135963));
#57883=CARTESIAN_POINT('Ctrl Pts',(-0.728744413965246,-0.357037429469062,
0.878319677166941));
#57884=CARTESIAN_POINT('Ctrl Pts',(-0.751978600292447,-0.32968521463109,
0.859423759568971));
#57885=CARTESIAN_POINT('Ctrl Pts',(-0.794210469526026,-0.267260154796303,
0.825735732037568));
#57886=CARTESIAN_POINT('Ctrl Pts',(-0.812815008506795,-0.232133375781979,
0.811288084500528));
#57887=CARTESIAN_POINT('Ctrl Pts',(-0.827500847770699,-0.194273896699414,
0.8));
#57888=CARTESIAN_POINT('Ctrl Pts',(0.,-0.458257569495584,1.3));
#57889=CARTESIAN_POINT('Ctrl Pts',(-0.0876016538044516,-0.458257569495584,
1.3));
#57890=CARTESIAN_POINT('Ctrl Pts',(-0.183814615587506,-0.462023903676248,
1.3));
#57891=CARTESIAN_POINT('Ctrl Pts',(-0.309024935784565,-0.470333761200034,
1.3));
#57892=CARTESIAN_POINT('Ctrl Pts',(-0.338138729685014,-0.47246220371005,
1.3));
#57893=CARTESIAN_POINT('Ctrl Pts',(-0.367006645104718,-0.474664220738176,
1.3));
#57894=CARTESIAN_POINT('Origin',(0.,0.,0.8));
#57895=CARTESIAN_POINT('',(-1.05,-1.28587913910472E-16,0.8));
#57896=CARTESIAN_POINT('Origin',(0.,0.,0.8));
#57897=CARTESIAN_POINT('Origin',(0.,0.,0.8));
#57898=CARTESIAN_POINT('Origin',(0.,0.,0.8));
#57899=CARTESIAN_POINT('Origin',(0.,0.,1.3));
#57900=CARTESIAN_POINT('Origin',(0.,0.,1.3));
#57901=CARTESIAN_POINT('Origin',(0.,0.,1.));
#57902=CARTESIAN_POINT('Origin',(0.,0.,1.));
#57903=CARTESIAN_POINT('Origin',(0.,0.,1.3));
#57904=CARTESIAN_POINT('Origin',(0.,0.,1.3));
#57905=CARTESIAN_POINT('Origin',(1.25,0.,0.));
#57906=CARTESIAN_POINT('',(-1.25,-1.53080849893419E-16,0.));
#57907=CARTESIAN_POINT('Origin',(0.,0.,0.));
#57908=CARTESIAN_POINT('',(0.230288547470477,0.435342893480459,0.));
#57909=CARTESIAN_POINT('Ctrl Pts',(-0.407032914766026,-0.00372944996921218,
2.22044604925031E-16));
#57910=CARTESIAN_POINT('Ctrl Pts',(-0.409502406107154,0.0185484342735974,
1.33393110592597E-16));
#57911=CARTESIAN_POINT('Ctrl Pts',(-0.410064146186531,0.0409298249901961,
6.41710304853556E-17));
#57912=CARTESIAN_POINT('Ctrl Pts',(-0.408816203516182,0.0632211419519473,
-2.58907478789538E-16));
#57913=CARTESIAN_POINT('Ctrl Pts',(-0.408113237416965,0.0757778406716244,
-4.40897601254181E-16));
#57914=CARTESIAN_POINT('Ctrl Pts',(-0.406835127950302,0.0883063527932494,
-1.57466213752448E-16));
#57915=CARTESIAN_POINT('Ctrl Pts',(-0.404992377388169,0.100773692152307,
-6.07153216591882E-18));
#57916=CARTESIAN_POINT('Ctrl Pts',(-0.404012526054069,0.107402988246245,
7.44300201204056E-17));
#57917=CARTESIAN_POINT('Ctrl Pts',(-0.402873550921039,0.114009987474989,
-1.14344253592689E-16));
#57918=CARTESIAN_POINT('Ctrl Pts',(-0.401579163263675,0.120581758409531,
-1.8474805019153E-16));
#57919=CARTESIAN_POINT('Ctrl Pts',(-0.397116077809508,0.143241411488897,
-4.2750234310436E-16));
#57920=CARTESIAN_POINT('Ctrl Pts',(-0.390805198236086,0.165510695939246,
-2.33788451815087E-16));
#57921=CARTESIAN_POINT('Ctrl Pts',(-0.38271795691015,0.187189446898724,
-2.74086309204336E-16));
#57922=CARTESIAN_POINT('Ctrl Pts',(-0.381208311546034,0.191236219409497,
-2.81608710371759E-16));
#57923=CARTESIAN_POINT('Ctrl Pts',(-0.379636621493342,0.195262415265924,
-3.76247800759317E-16));
#57924=CARTESIAN_POINT('Ctrl Pts',(-0.378003151308578,0.199266719882105,
-4.02455846426619E-16));
#57925=CARTESIAN_POINT('Ctrl Pts',(-0.374957182270889,0.206733637853503,
-4.54796032731822E-16));
#57926=CARTESIAN_POINT('Ctrl Pts',(-0.371694472063554,0.214127904294756,
-6.04095780210171E-16));
#57927=CARTESIAN_POINT('Ctrl Pts',(-0.368232811861738,0.221415799627647,
-6.38378239159465E-16));
#57928=CARTESIAN_POINT('Ctrl Pts',(-0.358129974694566,0.242685483983424,
-7.38431416034905E-16));
#57929=CARTESIAN_POINT('Ctrl Pts',(-0.346322064408441,0.263089787169291,
-3.51612244000906E-16));
#57930=CARTESIAN_POINT('Ctrl Pts',(-0.332976726379132,0.282417007099477,
-3.19189119579733E-16));
#57931=CARTESIAN_POINT('Ctrl Pts',(-0.321328421888677,0.299286519299645,
-2.90889017704434E-16));
#57932=CARTESIAN_POINT('Ctrl Pts',(-0.308507716760313,0.315336147391315,
-2.43035058606971E-16));
#57933=CARTESIAN_POINT('Ctrl Pts',(-0.294595609651327,0.330416226174529,
-5.55111512312578E-17));
#57934=CARTESIAN_POINT('Ctrl Pts',(-0.289438034934074,0.33600679793028,
1.40087680724686E-17));
#57935=CARTESIAN_POINT('Ctrl Pts',(-0.28413020536853,0.341463974937307,
-3.4552926784595E-16));
#57936=CARTESIAN_POINT('Ctrl Pts',(-0.278675394220103,0.346779509590223,
-3.78169717762944E-16));
#57937=CARTESIAN_POINT('Ctrl Pts',(-0.2742428149802,0.351098912757517,-4.04693345574494E-16));
#57938=CARTESIAN_POINT('Ctrl Pts',(-0.269718867723713,0.355319082487331,
-7.06198858179791E-16));
#57939=CARTESIAN_POINT('Ctrl Pts',(-0.265111332520466,0.359431662343205,
-7.11236625150491E-16));
#57940=CARTESIAN_POINT('Ctrl Pts',(-0.260094342853417,0.363909711827728,
-7.16722079677064E-16));
#57941=CARTESIAN_POINT('Ctrl Pts',(-0.254976429475008,0.368261987646387,
-1.0019210278739E-16));
#57942=CARTESIAN_POINT('Ctrl Pts',(-0.249761050372628,0.372483785414168,
-1.2490009027033E-16));
#57943=CARTESIAN_POINT('Ctrl Pts',(-0.231304668403533,0.387424043958917,
-2.15807103259361E-16));
#57944=CARTESIAN_POINT('Ctrl Pts',(-0.211631027480377,0.40073306681961,
-3.74687250457173E-16));
#57945=CARTESIAN_POINT('Ctrl Pts',(-0.190986132226159,0.412423252290443,
-5.72458747072346E-16));
#57946=CARTESIAN_POINT('Ctrl Pts',(-0.176606675051318,0.420565629341712,
-7.10209349870931E-16));
#57947=CARTESIAN_POINT('Ctrl Pts',(-0.161754960911602,0.427921985785738,
-3.10111003734457E-16));
#57948=CARTESIAN_POINT('Ctrl Pts',(-0.146504136099264,0.434485677558816,
-2.32452945780892E-16));
#57949=CARTESIAN_POINT('Ctrl Pts',(-0.141356939441595,0.436700942160703,
-2.06243130819525E-16));
#57950=CARTESIAN_POINT('Ctrl Pts',(-0.136164227967783,0.438825835570468,
-2.69285390156797E-16));
#57951=CARTESIAN_POINT('Ctrl Pts',(-0.130928672659677,0.440859850121791,
-2.81025203108243E-16));
#57952=CARTESIAN_POINT('Ctrl Pts',(-0.12556463322452,0.442943780788724,
-2.93053119141415E-16));
#57953=CARTESIAN_POINT('Ctrl Pts',(-0.120163646959754,0.444929160518309,
1.39490241327531E-16));
#57954=CARTESIAN_POINT('Ctrl Pts',(-0.114731899809621,0.446815240591704,
8.32667268468867E-17));
#57955=CARTESIAN_POINT('Ctrl Pts',(-0.090250938166801,0.455315830301767,
-1.70133452392181E-16));
#57956=CARTESIAN_POINT('Ctrl Pts',(-0.0651300509740424,0.461810294150359,
-3.06185542203807E-16));
#57957=CARTESIAN_POINT('Ctrl Pts',(-0.0396563962731094,0.466299278577248,
-1.45716771982052E-16));
#57958=CARTESIAN_POINT('Ctrl Pts',(-0.0205511552474096,0.469666016897415,
-2.53651943157355E-17));
#57959=CARTESIAN_POINT('Ctrl Pts',(-0.00124630488774171,0.471903779543234,
2.41706311978087E-16));
#57960=CARTESIAN_POINT('Ctrl Pts',(0.0181468923706612,0.472993406137991,
3.2612801348364E-16));
#57961=CARTESIAN_POINT('Ctrl Pts',(0.0255821880205217,0.473411165817946,
3.58495049284613E-16));
#57962=CARTESIAN_POINT('Ctrl Pts',(0.0330305209702806,0.473659971890404,
-9.54367323080526E-17));
#57963=CARTESIAN_POINT('Ctrl Pts',(0.040485736875469,0.473738030558778,
-8.32667268468867E-17));
#57964=CARTESIAN_POINT('Ctrl Pts',(0.0468700728995737,0.473804876747384,
-7.28448416503496E-17));
#57965=CARTESIAN_POINT('Ctrl Pts',(0.0532608144088334,0.473746273409567,
-2.22757456392369E-16));
#57966=CARTESIAN_POINT('Ctrl Pts',(0.0596358754189341,0.473561936641337,
-2.08166817117217E-16));
#57967=CARTESIAN_POINT('Ctrl Pts',(0.0853914116867899,0.47281720771841,
-1.49219971208295E-16));
#57968=CARTESIAN_POINT('Ctrl Pts',(0.110956177502877,0.470026036127248,
2.37366919974466E-16));
#57969=CARTESIAN_POINT('Ctrl Pts',(0.136073147414297,0.465167209120457,
-2.08166817117217E-17));
#57970=CARTESIAN_POINT('Ctrl Pts',(0.15428584587622,0.461643999455222,-2.08029554200206E-16));
#57971=CARTESIAN_POINT('Ctrl Pts',(0.172263718537645,0.457032689199025,
-3.38570523553356E-16));
#57972=CARTESIAN_POINT('Ctrl Pts',(0.18991046284926,0.451308070908747,-3.05311331771918E-16));
#57973=CARTESIAN_POINT('Ctrl Pts',(0.203544498658142,0.446885178539278,
-2.79614976471743E-16));
#57974=CARTESIAN_POINT('Ctrl Pts',(0.216980922989279,0.44179740741506,-4.64126606240054E-17));
#57975=CARTESIAN_POINT('Ctrl Pts',(0.230193623813293,0.436078300125993,
-2.08166817117217E-17));
#57976=CARTESIAN_POINT('',(0.485198770445679,0.0844890712341007,0.));
#57977=CARTESIAN_POINT('Ctrl Pts',(0.485198770445679,0.0844890712341024,
0.));
#57978=CARTESIAN_POINT('Ctrl Pts',(0.487483556903401,0.0587811609303886,
-3.6403309418082E-17));
#57979=CARTESIAN_POINT('Ctrl Pts',(0.487669957905918,0.032999272007226,
-2.16332978629155E-16));
#57980=CARTESIAN_POINT('Ctrl Pts',(0.48581703237745,0.0073557324105081,
2.10335221462188E-16));
#57981=CARTESIAN_POINT('Ctrl Pts',(0.484978594933728,-0.00424781206935033,
4.03399966647938E-16));
#57982=CARTESIAN_POINT('Ctrl Pts',(0.483721893431401,-0.0158229198346243,
2.67290005872947E-16));
#57983=CARTESIAN_POINT('Ctrl Pts',(0.482049056063943,-0.0273488775086491,
3.18321757841744E-16));
#57984=CARTESIAN_POINT('Ctrl Pts',(0.480594436537202,-0.0373713001440821,
3.62696533502297E-16));
#57985=CARTESIAN_POINT('Ctrl Pts',(0.478823707565005,-0.0473618152739592,
2.79537773708781E-16));
#57986=CARTESIAN_POINT('Ctrl Pts',(0.476744474029188,-0.0572755363954163,
2.58473797920544E-16));
#57987=CARTESIAN_POINT('Ctrl Pts',(0.471567675914175,-0.0819583495235461,
2.06029496558142E-16));
#57988=CARTESIAN_POINT('Ctrl Pts',(0.464479206920196,-0.106198761077193,
1.05439529942102E-16));
#57989=CARTESIAN_POINT('Ctrl Pts',(0.455507744329332,-0.129784129861741,
-2.60208521396521E-17));
#57990=CARTESIAN_POINT('Ctrl Pts',(0.453016977318907,-0.136332187985184,
-6.25184889018675E-17));
#57991=CARTESIAN_POINT('Ctrl Pts',(0.450380803012963,-0.142829602956097,
3.48322078259034E-16));
#57992=CARTESIAN_POINT('Ctrl Pts',(0.447599240832732,-0.149271416802534,
3.17454396103756E-16));
#57993=CARTESIAN_POINT('Ctrl Pts',(0.444098051027165,-0.157379814712454,
2.80213370992714E-16));
#57994=CARTESIAN_POINT('Ctrl Pts',(0.440363895277044,-0.16540477046754,
8.12677602785049E-16));
#57995=CARTESIAN_POINT('Ctrl Pts',(0.436415237431444,-0.173307069589165,
7.52869988573934E-16));
#57996=CARTESIAN_POINT('Ctrl Pts',(0.425357271841625,-0.195436956549305,
5.8538256225953E-16));
#57997=CARTESIAN_POINT('Ctrl Pts',(0.412606104374067,-0.216645497952098,
-5.94784681012512E-16));
#57998=CARTESIAN_POINT('Ctrl Pts',(0.398278421228196,-0.236702761090162,
-3.67761376907083E-16));
#57999=CARTESIAN_POINT('Ctrl Pts',(0.385785090947335,-0.25419212139795,
-1.69803543057391E-16));
#58000=CARTESIAN_POINT('Ctrl Pts',(0.372092020529464,-0.270806277051948,
4.79495696309758E-17));
#58001=CARTESIAN_POINT('Ctrl Pts',(0.357255291902388,-0.286367384027322,
-3.46944695195361E-17));
#58002=CARTESIAN_POINT('Ctrl Pts',(0.351948789708481,-0.291932967275489,
-6.42529244922329E-17));
#58003=CARTESIAN_POINT('Ctrl Pts',(0.346495839949595,-0.297363574914842,
-1.69058141018443E-18));
#58004=CARTESIAN_POINT('Ctrl Pts',(0.340898563514322,-0.302650088761903,
4.16333634234434E-17));
#58005=CARTESIAN_POINT('Ctrl Pts',(0.336804911074738,-0.3065164603012,7.33189831192914E-17));
#58006=CARTESIAN_POINT('Ctrl Pts',(0.332634530931966,-0.31030506503389,
6.30416444442976E-17));
#58007=CARTESIAN_POINT('Ctrl Pts',(0.32839819773127,-0.314004190957375,
1.73472347597681E-17));
#58008=CARTESIAN_POINT('Ctrl Pts',(0.322231718417059,-0.319388702138902,
-4.91663322203621E-17));
#58009=CARTESIAN_POINT('Ctrl Pts',(0.315920306588548,-0.324588673796501,
-6.16839946309463E-17));
#58010=CARTESIAN_POINT('Ctrl Pts',(0.309467897502568,-0.329595262505712,
-4.16333634234434E-17));
#58011=CARTESIAN_POINT('Ctrl Pts',(0.2903984307146,-0.34439174794845,1.29797962091697E-17));
#58012=CARTESIAN_POINT('Ctrl Pts',(0.270098895473702,-0.357502851052604,
2.59113934393091E-17));
#58013=CARTESIAN_POINT('Ctrl Pts',(0.248817934772457,-0.368892164122873,
7.97972798949331E-17));
#58014=CARTESIAN_POINT('Ctrl Pts',(0.235636505678278,-0.375946705728147,
1.131742031205E-16));
#58015=CARTESIAN_POINT('Ctrl Pts',(0.222078033344231,-0.382339701258627,
2.48960342182608E-16));
#58016=CARTESIAN_POINT('Ctrl Pts',(0.208199770326819,-0.388052725523839,
1.73472347597681E-16));
#58017=CARTESIAN_POINT('Ctrl Pts',(0.202217607700804,-0.390515298844289,
1.40933588290973E-16));
#58018=CARTESIAN_POINT('Ctrl Pts',(0.196176028138775,-0.392851437390717,
7.6873750064169E-17));
#58019=CARTESIAN_POINT('Ctrl Pts',(0.190079662327023,-0.395059224742947,
6.93889390390723E-17));
#58020=CARTESIAN_POINT('Ctrl Pts',(0.184991168671714,-0.39690201309932,
6.31415427068228E-17));
#58021=CARTESIAN_POINT('Ctrl Pts',(0.179873425524456,-0.398652142795515,
3.22125190683935E-16));
#58022=CARTESIAN_POINT('Ctrl Pts',(0.174729796135838,-0.400309233186663,
3.2612801348364E-16));
#58023=CARTESIAN_POINT('Ctrl Pts',(0.152320431852445,-0.407528715661023,
3.43567200389085E-16));
#58024=CARTESIAN_POINT('Ctrl Pts',(0.129416852758522,-0.412987388760869,
3.861200852693E-16));
#58025=CARTESIAN_POINT('Ctrl Pts',(0.106249389798624,-0.41663803834582,
1.94289029309402E-16));
#58026=CARTESIAN_POINT('Ctrl Pts',(0.0893279915812928,-0.419304454408977,
5.41765925714067E-17));
#58027=CARTESIAN_POINT('Ctrl Pts',(0.0722654389196746,-0.421005297656241,
-2.92341994274838E-16));
#58028=CARTESIAN_POINT('Ctrl Pts',(0.0551537264920908,-0.421704837827871,
-4.02455846426619E-16));
#58029=CARTESIAN_POINT('Ctrl Pts',(0.0458345023082366,-0.422085814992642,
-4.62425044617213E-16));
#58030=CARTESIAN_POINT('Ctrl Pts',(0.0365007667942034,-0.422169548039371,
2.12962436588982E-16));
#58031=CARTESIAN_POINT('Ctrl Pts',(0.0271681775545658,-0.42194840310141,
2.0122792321331E-16));
#58032=CARTESIAN_POINT('Ctrl Pts',(0.021361805766906,-0.421810815375669,
1.93927168229147E-16));
#58033=CARTESIAN_POINT('Ctrl Pts',(0.0155642672926311,-0.421555318758217,
9.02804926475444E-17));
#58034=CARTESIAN_POINT('Ctrl Pts',(0.00978415844817893,-0.421181351844719,
5.55111512312578E-17));
#58035=CARTESIAN_POINT('Ctrl Pts',(-0.0123651918621571,-0.419748312364936,
-7.77248039753947E-17));
#58036=CARTESIAN_POINT('Ctrl Pts',(-0.0342836622346571,-0.416578763165458,
1.73036456657562E-16));
#58037=CARTESIAN_POINT('Ctrl Pts',(-0.0557672279919517,-0.411605196435151,
9.71445146547012E-17));
#58038=CARTESIAN_POINT('Ctrl Pts',(-0.069304109276844,-0.408471332012863,
4.93246964281187E-17));
#58039=CARTESIAN_POINT('Ctrl Pts',(-0.0826681142898227,-0.404620280484352,
7.89361148452016E-17));
#58040=CARTESIAN_POINT('Ctrl Pts',(-0.0958034133885173,-0.400025521834758,
1.38777878078145E-17));
#58041=CARTESIAN_POINT('Ctrl Pts',(-0.107098233124042,-0.396074567213513,
-4.9003652258222E-17));
#58042=CARTESIAN_POINT('Ctrl Pts',(-0.118223898010513,-0.39157345838643,
5.62305508459485E-18));
#58043=CARTESIAN_POINT('Ctrl Pts',(-0.129150719006634,-0.38654594480115,
-6.93889390390723E-18));
#58044=CARTESIAN_POINT('Origin',(0.,0.,0.));
#58045=CARTESIAN_POINT('Origin',(0.,0.,0.3));
#58046=CARTESIAN_POINT('',(-1.25,-1.53080849893419E-16,0.6));
#58047=CARTESIAN_POINT('Origin',(0.,0.,0.6));
#58048=CARTESIAN_POINT('',(-1.25,-1.53080849893419E-16,0.3));
#58049=CARTESIAN_POINT('Origin',(0.,0.,0.7));
#58050=CARTESIAN_POINT('',(-1.15,-1.40834381901946E-16,0.7));
#58051=CARTESIAN_POINT('Ctrl Pts',(0.285821514250011,-0.40107644158169,
-1.67683458050225));
#58052=CARTESIAN_POINT('Ctrl Pts',(0.351951188739807,-0.35395005433991,
-1.67289834909262));
#58053=CARTESIAN_POINT('Ctrl Pts',(0.459413146959217,-0.226542587597284,
-1.66502588627336));
#58054=CARTESIAN_POINT('Ctrl Pts',(0.532521434237499,0.101635635160784,
-1.64928096063485));
#58055=CARTESIAN_POINT('Ctrl Pts',(0.300949767170296,0.496361842456049,
-1.6295998035867));
#58056=CARTESIAN_POINT('Ctrl Pts',(-0.250382990617479,0.524039845133421,
-1.60598241512892));
#58057=CARTESIAN_POINT('Ctrl Pts',(-0.574972636888615,0.078666076090792,
-1.58236502667114));
#58058=CARTESIAN_POINT('Ctrl Pts',(-0.381802551317379,-0.437278299044204,
-1.55874763821336));
#58059=CARTESIAN_POINT('Ctrl Pts',(0.155808618062042,-0.559226858156241,
-1.53513024975558));
#58060=CARTESIAN_POINT('Ctrl Pts',(0.552827150676151,-0.176984815689186,
-1.51151286129781));
#58061=CARTESIAN_POINT('Ctrl Pts',(0.45158996229556,0.364747576723814,-1.48789547284003));
#58062=CARTESIAN_POINT('Ctrl Pts',(-0.0567588509522337,0.577713399197876,
-1.46427808438225));
#58063=CARTESIAN_POINT('Ctrl Pts',(-0.513923878567292,0.269903117161945,
-1.44066069592447));
#58064=CARTESIAN_POINT('Ctrl Pts',(-0.507837364089479,-0.281196945664769,
-1.41704330746669));
#58065=CARTESIAN_POINT('Ctrl Pts',(-0.0439699112909389,-0.578823520702787,
-1.39342591900891));
#58066=CARTESIAN_POINT('Ctrl Pts',(0.459530134105091,-0.354684349671076,
-1.36980853055114));
#58067=CARTESIAN_POINT('Ctrl Pts',(0.548801327297502,0.189173966061256,
-1.34619114209336));
#58068=CARTESIAN_POINT('Ctrl Pts',(0.143370464394534,0.562507297565094,
-1.32257375363558));
#58069=CARTESIAN_POINT('Ctrl Pts',(-0.391297213964002,0.428784228150806,
-1.2989563651778));
#58070=CARTESIAN_POINT('Ctrl Pts',(-0.57324139440495,-0.0914540128567207,
-1.27533897672002));
#58071=CARTESIAN_POINT('Ctrl Pts',(-0.238453374898797,-0.529253712919782,
-1.25172158826224));
#58072=CARTESIAN_POINT('Ctrl Pts',(0.311281577262681,-0.489972724697733,
-1.22810419980447));
#58073=CARTESIAN_POINT('Ctrl Pts',(0.58042066573113,-0.00901982792740492,
-1.20448681134669));
#58074=CARTESIAN_POINT('Ctrl Pts',(0.326356097327604,0.480063744892664,
-1.18086942288891));
#58075=CARTESIAN_POINT('Ctrl Pts',(-0.221892851772901,0.53640755265549,
-1.15725203443113));
#58076=CARTESIAN_POINT('Ctrl Pts',(-0.570122827353299,0.109222085715003,
-1.13363464597335));
#58077=CARTESIAN_POINT('Ctrl Pts',(-0.404431851492691,-0.416418514146393,
-1.11001725751558));
#58078=CARTESIAN_POINT('Ctrl Pts',(0.125822671827455,-0.566690529838469,
-1.0863998690578));
#58079=CARTESIAN_POINT('Ctrl Pts',(0.542657939641386,-0.206135543197639,
-1.06278248060002));
#58080=CARTESIAN_POINT('Ctrl Pts',(0.470329696914535,0.34023444518466,-1.03916509214224));
#58081=CARTESIAN_POINT('Ctrl Pts',(-0.025963826007878,0.579909804394615,
-1.01554770368446));
#58082=CARTESIAN_POINT('Ctrl Pts',(-0.498852999158645,0.296842023235613,
-0.991930315226685));
#58083=CARTESIAN_POINT('Ctrl Pts',(-0.52206537526902,-0.253805526836494,
-0.968312926768907));
#58084=CARTESIAN_POINT('Ctrl Pts',(-0.0746768205240931,-0.57566732926795,
-0.944695538311129));
#58085=CARTESIAN_POINT('Ctrl Pts',(0.440027022543379,-0.378610249393483,
-0.921078149853351));
#58086=CARTESIAN_POINT('Ctrl Pts',(0.558081066117299,0.1597342328763,-0.897460761395573));
#58087=CARTESIAN_POINT('Ctrl Pts',(0.173068862321762,0.554090850318274,
-0.873843372937794));
#58088=CARTESIAN_POINT('Ctrl Pts',(-0.367951327395403,0.448978086525479,
-0.850225984480016));
#58089=CARTESIAN_POINT('Ctrl Pts',(-0.577292295711129,-0.060853157885975,
-0.826608596022237));
#58090=CARTESIAN_POINT('Ctrl Pts',(-0.2662496020955,-0.515830060093211,
-0.802991207564461));
#58091=CARTESIAN_POINT('Ctrl Pts',(0.28479619558802,-0.505826678309667,
-0.77937381910668));
#58092=CARTESIAN_POINT('Ctrl Pts',(0.579120591889377,-0.039860275511877,
-0.755756430648904));
#58093=CARTESIAN_POINT('Ctrl Pts',(0.351413260849551,0.462037034889159,
-0.732139042191124));
#58094=CARTESIAN_POINT('Ctrl Pts',(-0.193065523547594,0.547444248416976,
-0.708521653733348));
#58095=CARTESIAN_POINT('Ctrl Pts',(-0.563510902565598,0.139373470280007,
-0.684904265275568));
#58096=CARTESIAN_POINT('Ctrl Pts',(-0.425995463083871,-0.394331544421604,
-0.661286876817791));
#58097=CARTESIAN_POINT('Ctrl Pts',(0.095521427029711,-0.572577644051913,
-0.637669488360011));
#58098=CARTESIAN_POINT('Ctrl Pts',(0.530933253458391,-0.234689969954635,
-0.614052099902234));
#58099=CARTESIAN_POINT('Ctrl Pts',(0.487750452992866,0.314752278720359,
-0.590434711444455));
#58100=CARTESIAN_POINT('Ctrl Pts',(0.00489892952646269,0.580470069784127,
-0.566817322986678));
#58101=CARTESIAN_POINT('Ctrl Pts',(-0.482368595405421,0.322939685458225,
-0.543199934528898));
#58102=CARTESIAN_POINT('Ctrl Pts',(-0.534818716119646,-0.225695460968752,
-0.519582546071121));
#58103=CARTESIAN_POINT('Ctrl Pts',(-0.105171775600954,-0.570883875267303,
-0.495965157613343));
#58104=CARTESIAN_POINT('Ctrl Pts',(0.419279269138383,-0.401465317274596,
-0.472347769155565));
#58105=CARTESIAN_POINT('Ctrl Pts',(0.565782966987249,0.129842695435552,
-0.448730380697786));
#58106=CARTESIAN_POINT('Ctrl Pts',(0.202277792416376,0.544107709314211,
-0.425112992240008));
#58107=CARTESIAN_POINT('Ctrl Pts',(-0.343564989114983,0.467902373344431,
-0.40149560378223));
#58108=CARTESIAN_POINT('Ctrl Pts',(-0.579710793277147,-0.0300802281383343,
-0.377878215324452));
#58109=CARTESIAN_POINT('Ctrl Pts',(-0.293293089483625,-0.500947815182221,
-0.354260826866673));
#58110=CARTESIAN_POINT('Ctrl Pts',(0.257505759040535,-0.520250391965063,
-0.330643438408895));
#58111=CARTESIAN_POINT('Ctrl Pts',(0.576182504633862,-0.0705879126061006,
-0.307026049951117));
#58112=CARTESIAN_POINT('Ctrl Pts',(0.375477683372268,0.442703659920605,
-0.283408661493339));
#58113=CARTESIAN_POINT('Ctrl Pts',(-0.163694059152507,0.556933358324603,
-0.259791273035561));
#58114=CARTESIAN_POINT('Ctrl Pts',(-0.555302152523182,0.169130024000774,
-0.236173884577782));
#58115=CARTESIAN_POINT('Ctrl Pts',(-0.446361113399504,-0.371128138543734,
-0.212556496120004));
#58116=CARTESIAN_POINT('Ctrl Pts',(0.0649627696741521,-0.576848443985302,
-0.188939107662226));
#58117=CARTESIAN_POINT('Ctrl Pts',(0.517682881343619,-0.262575546982227,
-0.165321719204448));
#58118=CARTESIAN_POINT('Ctrl Pts',(0.503838986030669,0.288370040921889,
-0.141704330746669));
#58119=CARTESIAN_POINT('Ctrl Pts',(0.0356574830697532,0.579408355918849,
-0.118086942288891));
#58120=CARTESIAN_POINT('Ctrl Pts',(-0.464346188869441,0.348086916704139,
-0.0944695538311128));
#58121=CARTESIAN_POINT('Ctrl Pts',(-0.54639681349325,-0.196875400907364,
-0.0708521653733346));
#58122=CARTESIAN_POINT('Ctrl Pts',(-0.134700387395815,-0.564625226713823,
-0.0472347769155564));
#58123=CARTESIAN_POINT('Ctrl Pts',(0.307439751116493,-0.44653071528208,
-0.0275536198674081));
#58124=CARTESIAN_POINT('Ctrl Pts',(0.486049448357886,-0.161672252861274,
-0.0118086942288891));
#58125=CARTESIAN_POINT('Ctrl Pts',(0.499129368704262,0.0044892671421744,
-0.00393623140962979));
#58126=CARTESIAN_POINT('Ctrl Pts',(0.485198770445679,0.0844890712341024,
0.));
#58127=CARTESIAN_POINT('Ctrl Pts',(0.269291261530782,-0.377880514723377,
-1.66038972033484));
#58128=CARTESIAN_POINT('Ctrl Pts',(0.331596380565313,-0.333479643413787,
-1.65645348892521));
#58129=CARTESIAN_POINT('Ctrl Pts',(0.432843364619005,-0.213440682954178,
-1.64858102610595));
#58130=CARTESIAN_POINT('Ctrl Pts',(0.501723494098348,0.0957576216078316,
-1.63283610046743));
#58131=CARTESIAN_POINT('Ctrl Pts',(0.283544584358314,0.467655162633464,
-1.61315494341928));
#58132=CARTESIAN_POINT('Ctrl Pts',(-0.235902295830161,0.493732430739748,
-1.5895375549615));
#58133=CARTESIAN_POINT('Ctrl Pts',(-0.541719566281419,0.0741164881368422,
-1.56592016650372));
#58134=CARTESIAN_POINT('Ctrl Pts',(-0.359721314085519,-0.411988667468349,
-1.54230277804595));
#58135=CARTESIAN_POINT('Ctrl Pts',(0.146797554499674,-0.526884431740369,
-1.51868538958817));
#58136=CARTESIAN_POINT('Ctrl Pts',(0.520854846090516,-0.166749044115146,
-1.49506800113039));
#58137=CARTESIAN_POINT('Ctrl Pts',(0.425472627420327,0.34365269995153,-1.47145061267261));
#58138=CARTESIAN_POINT('Ctrl Pts',(-0.0534762493861652,0.544301818851712,
-1.44783322421483));
#58139=CARTESIAN_POINT('Ctrl Pts',(-0.484201512798375,0.25429349187498,
-1.42421583575705));
#58140=CARTESIAN_POINT('Ctrl Pts',(-0.47846700689053,-0.264934151074547,
-1.40059844729927));
#58141=CARTESIAN_POINT('Ctrl Pts',(-0.0414269475550245,-0.5453477373904,
-1.3769810588415));
#58142=CARTESIAN_POINT('Ctrl Pts',(0.432953585909302,-0.334171471377069,
-1.35336367038372));
#58143=CARTESIAN_POINT('Ctrl Pts',(0.517061852903206,0.178233244978392,
-1.32974628192594));
#58144=CARTESIAN_POINT('Ctrl Pts',(0.13507875124224,0.529975149628081,-1.30612889346816));
#58145=CARTESIAN_POINT('Ctrl Pts',(-0.368666860709707,0.40398584419447,
-1.28251150501038));
#58146=CARTESIAN_POINT('Ctrl Pts',(-0.540088448786064,-0.0861648450742474,
-1.25889411655261));
#58147=CARTESIAN_POINT('Ctrl Pts',(-0.224662619646612,-0.49864475876141,
-1.23527672809483));
#58148=CARTESIAN_POINT('Ctrl Pts',(0.293278862692737,-0.461635554257514,
-1.21165933963705));
#58149=CARTESIAN_POINT('Ctrl Pts',(0.546852512846713,-0.00849817358128052,
-1.18804195117927));
#58150=CARTESIAN_POINT('Ctrl Pts',(0.3074815602605,0.452299652167739,-1.16442456272149));
#58151=CARTESIAN_POINT('Ctrl Pts',(-0.209059860785428,0.505384862046751,
-1.14080717426371));
#58152=CARTESIAN_POINT('Ctrl Pts',(-0.537150241500616,0.102905316020012,
-1.11718978580594));
#58153=CARTESIAN_POINT('Ctrl Pts',(-0.381041867255769,-0.392335291111666,
-1.09357239734816));
#58154=CARTESIAN_POINT('Ctrl Pts',(0.118545820857808,-0.533916448095865,
-1.06995500889038));
#58155=CARTESIAN_POINT('Ctrl Pts',(0.511273763030655,-0.194213863220489,
-1.0463376204326));
#58156=CARTESIAN_POINT('Ctrl Pts',(0.443128564866245,0.320557265258415,
-1.02272023197482));
#58157=CARTESIAN_POINT('Ctrl Pts',(-0.0244622294377454,0.546371196756361,
-0.999102843517045));
#58158=CARTESIAN_POINT('Ctrl Pts',(-0.470002245332516,0.279674408423102,
-0.975485455059269));
#58159=CARTESIAN_POINT('Ctrl Pts',(-0.49187215271962,-0.239126892475631,
-0.951868066601488));
#58160=CARTESIAN_POINT('Ctrl Pts',(-0.0703579478920888,-0.542374081697089,
-0.928250678143711));
#58161=CARTESIAN_POINT('Ctrl Pts',(0.41457842079967,-0.356713636323652,
-0.904633289685933));
#58162=CARTESIAN_POINT('Ctrl Pts',(0.525804905643713,0.150496134602677,
-0.881015901228154));
#58163=CARTESIAN_POINT('Ctrl Pts',(0.163059566697128,0.522045460700883,
-0.857398512770376));
#58164=CARTESIAN_POINT('Ctrl Pts',(-0.346671164332164,0.423011807341991,
-0.833781124312598));
#58165=CARTESIAN_POINT('Ctrl Pts',(-0.543905069539545,-0.0573337654383577,
-0.810163735854821));
#58166=CARTESIAN_POINT('Ctrl Pts',(-0.250851274854172,-0.485997451880037,
-0.786546347397042));
#58167=CARTESIAN_POINT('Ctrl Pts',(0.268325241332186,-0.476572607472738,
-0.762928958939263));
#58168=CARTESIAN_POINT('Ctrl Pts',(0.545627627708702,-0.0375549891887017,
-0.739311570481486));
#58169=CARTESIAN_POINT('Ctrl Pts',(0.331089563293141,0.435315502143794,
-0.715694182023707));
#58170=CARTESIAN_POINT('Ctrl Pts',(-0.181899737431087,0.515783259566058,
-0.692076793565929));
#58171=CARTESIAN_POINT('Ctrl Pts',(-0.530920711956982,0.131312920002222,
-0.66845940510815));
#58172=CARTESIAN_POINT('Ctrl Pts',(-0.4013583650666,-0.371525703155395,
-0.644842016650373));
#58173=CARTESIAN_POINT('Ctrl Pts',(0.0899970236864376,-0.539463085889993,
-0.621224628192594));
#58174=CARTESIAN_POINT('Ctrl Pts',(0.500227164451271,-0.221116868138983,
-0.597607239734816));
#58175=CARTESIAN_POINT('Ctrl Pts',(0.459541805813008,0.296548838979816,
-0.573989851277038));
#58176=CARTESIAN_POINT('Ctrl Pts',(0.00461560395756986,0.546899059656848,
-0.550372462819259));
#58177=CARTESIAN_POINT('Ctrl Pts',(-0.45447120354255,0.304262733767933,
-0.526755074361482));
#58178=CARTESIAN_POINT('Ctrl Pts',(-0.503887914568089,-0.212642549199021,
-0.503137685903703));
#58179=CARTESIAN_POINT('Ctrl Pts',(-0.0990892522675508,-0.537867274833063,
-0.479520297445925));
#58180=CARTESIAN_POINT('Ctrl Pts',(0.395030596686354,-0.378246900109711,
-0.455902908988147));
#58181=CARTESIAN_POINT('Ctrl Pts',(0.53306137339736,0.122333349699535,-0.432285520530368));
#58182=CARTESIAN_POINT('Ctrl Pts',(0.190579222289824,0.512639686464196,
-0.408668132072591));
#58183=CARTESIAN_POINT('Ctrl Pts',(-0.323695189913716,0.440841623562851,
-0.385050743614812));
#58184=CARTESIAN_POINT('Ctrl Pts',(-0.546183695283555,-0.0283405628290827,
-0.361433355157034));
#58185=CARTESIAN_POINT('Ctrl Pts',(-0.276330724342253,-0.471975909390466,
-0.337815966699255));
#58186=CARTESIAN_POINT('Ctrl Pts',(0.24261312478672,-0.490162137485593,
-0.314198578241477));
#58187=CARTESIAN_POINT('Ctrl Pts',(0.542859462318489,-0.0665055186080004,
-0.290581189783699));
#58188=CARTESIAN_POINT('Ctrl Pts',(0.353762239687556,0.417100257050748,
-0.266963801325921));
#58189=CARTESIAN_POINT('Ctrl Pts',(-0.154226947575804,0.524723574589349,
-0.243346412868143));
#58190=CARTESIAN_POINT('Ctrl Pts',(-0.523186708236817,0.159348527858055,
-0.219729024410364));
#58191=CARTESIAN_POINT('Ctrl Pts',(-0.420546184709156,-0.34966424721476,
-0.196111635952586));
#58192=CARTESIAN_POINT('Ctrl Pts',(0.0612057012012895,-0.543486887614036,
-0.172494247494808));
#58193=CARTESIAN_POINT('Ctrl Pts',(0.487743116733933,-0.247389705703288,
-0.14887685903703));
#58194=CARTESIAN_POINT('Ctrl Pts',(0.47469987174551,0.271692396254022,-0.125259470579251));
#58195=CARTESIAN_POINT('Ctrl Pts',(0.0335952617984759,0.545898749141681,
-0.101642082121473));
#58196=CARTESIAN_POINT('Ctrl Pts',(-0.437491108098618,0.327955595531638,
-0.0780246936636949));
#58197=CARTESIAN_POINT('Ctrl Pts',(-0.514796402181575,-0.185489273660303,
-0.0544073052059169));
#58198=CARTESIAN_POINT('Ctrl Pts',(-0.126910101031704,-0.531970590082557,
-0.0307899167481385));
#58199=CARTESIAN_POINT('Ctrl Pts',(0.289659225408945,-0.420705977806036,
-0.0111087596999904));
#58200=CARTESIAN_POINT('Ctrl Pts',(0.457939177385175,-0.15232207079224,
0.0046361659385287));
#58201=CARTESIAN_POINT('Ctrl Pts',(0.470262631272262,0.00422963406109354,
0.012508628757788));
#58202=CARTESIAN_POINT('Ctrl Pts',(0.457137697731917,0.0796027151346424,
0.0164448601674178));
#58203=CARTESIAN_POINT('Ctrl Pts',(0.252761008811552,-0.354684587865065,
-1.64394486016742));
#58204=CARTESIAN_POINT('Ctrl Pts',(0.311241572390819,-0.313009232487664,
-1.64000862875779));
#58205=CARTESIAN_POINT('Ctrl Pts',(0.406273582278792,-0.200338778311071,
-1.63213616593853));
#58206=CARTESIAN_POINT('Ctrl Pts',(0.470925553959198,0.0898796080548794,
-1.61639124030001));
#58207=CARTESIAN_POINT('Ctrl Pts',(0.266139401546332,0.43894848281088,-1.59671008325186));
#58208=CARTESIAN_POINT('Ctrl Pts',(-0.221421601042844,0.463425016346075,
-1.57309269479408));
#58209=CARTESIAN_POINT('Ctrl Pts',(-0.508466495674223,0.0695669001828929,
-1.54947530633631));
#58210=CARTESIAN_POINT('Ctrl Pts',(-0.337640076853661,-0.386699035892494,
-1.52585791787853));
#58211=CARTESIAN_POINT('Ctrl Pts',(0.137786490937306,-0.494542005324496,
-1.50224052942075));
#58212=CARTESIAN_POINT('Ctrl Pts',(0.48888254150488,-0.156513272541107,
-1.47862314096297));
#58213=CARTESIAN_POINT('Ctrl Pts',(0.399355292545094,0.322557823179248,
-1.45500575250519));
#58214=CARTESIAN_POINT('Ctrl Pts',(-0.0501936478200969,0.510890238505547,
-1.43138836404742));
#58215=CARTESIAN_POINT('Ctrl Pts',(-0.454479147029459,0.238683866588015,
-1.40777097558963));
#58216=CARTESIAN_POINT('Ctrl Pts',(-0.449096649691581,-0.248671356484325,
-1.38415358713186));
#58217=CARTESIAN_POINT('Ctrl Pts',(-0.0388839838191108,-0.511871954078012,
-1.36053619867408));
#58218=CARTESIAN_POINT('Ctrl Pts',(0.406377037713513,-0.313658593083062,
-1.3369188102163));
#58219=CARTESIAN_POINT('Ctrl Pts',(0.48532237850891,0.167292523895527,-1.31330142175852));
#58220=CARTESIAN_POINT('Ctrl Pts',(0.126787038089945,0.497443001691069,
-1.28968403330074));
#58221=CARTESIAN_POINT('Ctrl Pts',(-0.34603650745541,0.379187460238132,
-1.26606664484297));
#58222=CARTESIAN_POINT('Ctrl Pts',(-0.506935503167179,-0.0808756772917736,
-1.24244925638519));
#58223=CARTESIAN_POINT('Ctrl Pts',(-0.210871864394426,-0.468035804603038,
-1.21883186792741));
#58224=CARTESIAN_POINT('Ctrl Pts',(0.275276148122791,-0.433298383817296,
-1.19521447946963));
#58225=CARTESIAN_POINT('Ctrl Pts',(0.513284359962297,-0.00797651923515602,
-1.17159709101185));
#58226=CARTESIAN_POINT('Ctrl Pts',(0.288607023193397,0.424535559442814,
-1.14797970255408));
#58227=CARTESIAN_POINT('Ctrl Pts',(-0.196226869797954,0.474362171438012,
-1.1243623140963));
#58228=CARTESIAN_POINT('Ctrl Pts',(-0.504177655647933,0.0965885463250207,
-1.10074492563852));
#58229=CARTESIAN_POINT('Ctrl Pts',(-0.357651883018847,-0.36825206807694,
-1.07712753718074));
#58230=CARTESIAN_POINT('Ctrl Pts',(0.111268969888161,-0.501142366353261,
-1.05351014872296));
#58231=CARTESIAN_POINT('Ctrl Pts',(0.479889586419924,-0.182292183243338,
-1.02989276026518));
#58232=CARTESIAN_POINT('Ctrl Pts',(0.415927432817955,0.30088008533217,-1.00627537180741));
#58233=CARTESIAN_POINT('Ctrl Pts',(-0.0229606328676126,0.512832589118107,
-0.982657983349627));
#58234=CARTESIAN_POINT('Ctrl Pts',(-0.441151491506388,0.262506793610591,
-0.95904059489185));
#58235=CARTESIAN_POINT('Ctrl Pts',(-0.46167893017022,-0.224448258114767,
-0.935423206434071));
#58236=CARTESIAN_POINT('Ctrl Pts',(-0.0660390752600854,-0.509080834126229,
-0.911805817976294));
#58237=CARTESIAN_POINT('Ctrl Pts',(0.389129819055961,-0.334817023253821,
-0.888188429518514));
#58238=CARTESIAN_POINT('Ctrl Pts',(0.493528745170126,0.141258036329054,
-0.864571041060737));
#58239=CARTESIAN_POINT('Ctrl Pts',(0.153050271072494,0.490000071083492,
-0.840953652602958));
#58240=CARTESIAN_POINT('Ctrl Pts',(-0.325391001268926,0.397045528158503,
-0.81733626414518));
#58241=CARTESIAN_POINT('Ctrl Pts',(-0.51051784336796,-0.0538143729907405,
-0.793718875687403));
#58242=CARTESIAN_POINT('Ctrl Pts',(-0.235452947612843,-0.456164843666864,
-0.770101487229624));
#58243=CARTESIAN_POINT('Ctrl Pts',(0.251854287076352,-0.44731853663581,
-0.746484098771846));
#58244=CARTESIAN_POINT('Ctrl Pts',(0.512134663528028,-0.0352497028655255,
-0.722866710314067));
#58245=CARTESIAN_POINT('Ctrl Pts',(0.310765865736731,0.408593969398428,
-0.699249321856289));
#58246=CARTESIAN_POINT('Ctrl Pts',(-0.170733951314579,0.48412227071514,
-0.675631933398512));
#58247=CARTESIAN_POINT('Ctrl Pts',(-0.498330521348366,0.123252369724435,
-0.652014544940732));
#58248=CARTESIAN_POINT('Ctrl Pts',(-0.376721267049329,-0.348719861889185,
-0.628397156482956));
#58249=CARTESIAN_POINT('Ctrl Pts',(0.0844726203431644,-0.506348527728073,
-0.604779768025176));
#58250=CARTESIAN_POINT('Ctrl Pts',(0.469521075444152,-0.207543766323331,
-0.581162379567398));
#58251=CARTESIAN_POINT('Ctrl Pts',(0.431333158633148,0.278345399239273,
-0.55754499110962));
#58252=CARTESIAN_POINT('Ctrl Pts',(0.00433227838867778,0.51332804952957,
-0.533927602651842));
#58253=CARTESIAN_POINT('Ctrl Pts',(-0.426573811679679,0.28558578207764,
-0.510310214194063));
#58254=CARTESIAN_POINT('Ctrl Pts',(-0.472957113016533,-0.19958963742929,
-0.486692825736286));
#58255=CARTESIAN_POINT('Ctrl Pts',(-0.0930067289341476,-0.504850674398822,
-0.463075437278507));
#58256=CARTESIAN_POINT('Ctrl Pts',(0.370781924234325,-0.355028482944828,
-0.43945804882073));
#58257=CARTESIAN_POINT('Ctrl Pts',(0.50033977980747,0.114824003963517,-0.41584066036295));
#58258=CARTESIAN_POINT('Ctrl Pts',(0.178880652163271,0.48117166361418,-0.392223271905173));
#58259=CARTESIAN_POINT('Ctrl Pts',(-0.303825390712448,0.413780873781272,
-0.368605883447394));
#58260=CARTESIAN_POINT('Ctrl Pts',(-0.512656597289963,-0.0266008975198317,
-0.344988494989616));
#58261=CARTESIAN_POINT('Ctrl Pts',(-0.25936835920088,-0.44300400359871,
-0.321371106531837));
#58262=CARTESIAN_POINT('Ctrl Pts',(0.227720490532905,-0.460073883006124,
-0.29775371807406));
#58263=CARTESIAN_POINT('Ctrl Pts',(0.509536420003117,-0.0624231246098999,
-0.274136329616282));
#58264=CARTESIAN_POINT('Ctrl Pts',(0.332046796002844,0.391496854180891,
-0.250518941158503));
#58265=CARTESIAN_POINT('Ctrl Pts',(-0.1447598359991,0.492513790854095,-0.226901552700725));
#58266=CARTESIAN_POINT('Ctrl Pts',(-0.491071263950452,0.149567031715335,
-0.203284164242946));
#58267=CARTESIAN_POINT('Ctrl Pts',(-0.394731256018808,-0.328200355885785,
-0.179666775785168));
#58268=CARTESIAN_POINT('Ctrl Pts',(0.0574486327284271,-0.510125331242771,
-0.15604938732739));
#58269=CARTESIAN_POINT('Ctrl Pts',(0.457803352124247,-0.232203864424348,
-0.132431998869612));
#58270=CARTESIAN_POINT('Ctrl Pts',(0.445560757460351,0.255014751586155,
-0.108814610411834));
#58271=CARTESIAN_POINT('Ctrl Pts',(0.0315330405271981,0.512389142364513,
-0.0851972219540556));
#58272=CARTESIAN_POINT('Ctrl Pts',(-0.410636027327794,0.307824274359137,
-0.0615798334962771));
#58273=CARTESIAN_POINT('Ctrl Pts',(-0.483195990869901,-0.174103146413242,
-0.0379624450384991));
#58274=CARTESIAN_POINT('Ctrl Pts',(-0.119119814667592,-0.499315953451291,
-0.0143450565807207));
#58275=CARTESIAN_POINT('Ctrl Pts',(0.271878699701397,-0.394881240329992,
0.00533610046742732));
#58276=CARTESIAN_POINT('Ctrl Pts',(0.429828906412464,-0.142971888723207,
0.0210810261059466));
#58277=CARTESIAN_POINT('Ctrl Pts',(0.441395893840263,0.00397000098001296,
0.0289534889252056));
#58278=CARTESIAN_POINT('Ctrl Pts',(0.429076625018155,0.0747163590351825,
0.0328897203348354));
#58279=CARTESIAN_POINT('Ctrl Pts',(0.236230756092322,-0.331488661006753,
-1.6275));
#58280=CARTESIAN_POINT('Ctrl Pts',(0.290886764216325,-0.292538821561541,
-1.62356376859037));
#58281=CARTESIAN_POINT('Ctrl Pts',(0.37970379993858,-0.187236873667965,
-1.61569130577111));
#58282=CARTESIAN_POINT('Ctrl Pts',(0.440127613820048,0.0840015945019269,
-1.59994638013259));
#58283=CARTESIAN_POINT('Ctrl Pts',(0.24873421873435,0.410241802988297,-1.58026522308444));
#58284=CARTESIAN_POINT('Ctrl Pts',(-0.206940906255527,0.433117601952402,
-1.55664783462667));
#58285=CARTESIAN_POINT('Ctrl Pts',(-0.475213425067027,0.0650173122289433,
-1.53303044616889));
#58286=CARTESIAN_POINT('Ctrl Pts',(-0.315558839621802,-0.361409404316639,
-1.50941305771111));
#58287=CARTESIAN_POINT('Ctrl Pts',(0.128775427374938,-0.462199578908625,
-1.48579566925333));
#58288=CARTESIAN_POINT('Ctrl Pts',(0.456910236919244,-0.146277500967067,
-1.46217828079555));
#58289=CARTESIAN_POINT('Ctrl Pts',(0.373237957669861,0.301462946406964,
-1.43856089233778));
#58290=CARTESIAN_POINT('Ctrl Pts',(-0.046911046254029,0.477478658159383,
-1.41494350387999));
#58291=CARTESIAN_POINT('Ctrl Pts',(-0.424756781260542,0.22307424130105,
-1.39132611542222));
#58292=CARTESIAN_POINT('Ctrl Pts',(-0.419726292492632,-0.232408561894103,
-1.36770872696444));
#58293=CARTESIAN_POINT('Ctrl Pts',(-0.0363410200831963,-0.478396170765624,
-1.34409133850666));
#58294=CARTESIAN_POINT('Ctrl Pts',(0.379800489517723,-0.293145714789055,
-1.32047395004888));
#58295=CARTESIAN_POINT('Ctrl Pts',(0.453582904114614,0.156351802812663,
-1.2968565615911));
#58296=CARTESIAN_POINT('Ctrl Pts',(0.118495324937651,0.464910853754055,
-1.27323917313333));
#58297=CARTESIAN_POINT('Ctrl Pts',(-0.323406154201114,0.354389076281796,
-1.24962178467555));
#58298=CARTESIAN_POINT('Ctrl Pts',(-0.473782557548294,-0.0755865095093006,
-1.22600439621777));
#58299=CARTESIAN_POINT('Ctrl Pts',(-0.19708110914224,-0.437426850444666,
-1.20238700775999));
#58300=CARTESIAN_POINT('Ctrl Pts',(0.257273433552846,-0.404961213377078,
-1.17876961930221));
#58301=CARTESIAN_POINT('Ctrl Pts',(0.47971620707788,-0.00745486488903116,
-1.15515223084444));
#58302=CARTESIAN_POINT('Ctrl Pts',(0.269732486126293,0.396771466717889,
-1.13153484238666));
#58303=CARTESIAN_POINT('Ctrl Pts',(-0.183393878810481,0.443339480829272,
-1.10791745392888));
#58304=CARTESIAN_POINT('Ctrl Pts',(-0.47120506979525,0.0902717766300294,
-1.0843000654711));
#58305=CARTESIAN_POINT('Ctrl Pts',(-0.334261898781925,-0.344168845042214,
-1.06068267701332));
#58306=CARTESIAN_POINT('Ctrl Pts',(0.103992118918514,-0.468368284610657,
-1.03706528855554));
#58307=CARTESIAN_POINT('Ctrl Pts',(0.448505409809192,-0.170370503266186,
-1.01344790009777));
#58308=CARTESIAN_POINT('Ctrl Pts',(0.388726300769665,0.281202905405924,
-0.989830511639989));
#58309=CARTESIAN_POINT('Ctrl Pts',(-0.0214590362974804,0.479293981479854,
-0.96621312318221));
#58310=CARTESIAN_POINT('Ctrl Pts',(-0.412300737680259,0.245339178798079,
-0.942595734724431));
#58311=CARTESIAN_POINT('Ctrl Pts',(-0.43148570762082,-0.209769623753902,
-0.918978346266655));
#58312=CARTESIAN_POINT('Ctrl Pts',(-0.0617202026280809,-0.475787586555369,
-0.895360957808874));
#58313=CARTESIAN_POINT('Ctrl Pts',(0.363681217312252,-0.31292041018399,
-0.871743569351098));
#58314=CARTESIAN_POINT('Ctrl Pts',(0.461252584696539,0.132019938055431,
-0.848126180893318));
#58315=CARTESIAN_POINT('Ctrl Pts',(0.14304097544786,0.4579546814661,-0.824508792435541));
#58316=CARTESIAN_POINT('Ctrl Pts',(-0.304110838205687,0.371079248975015,
-0.800891403977763));
#58317=CARTESIAN_POINT('Ctrl Pts',(-0.477130617196376,-0.0502949805431236,
-0.777274015519985));
#58318=CARTESIAN_POINT('Ctrl Pts',(-0.220054620371515,-0.42633223545369,
-0.753656627062206));
#58319=CARTESIAN_POINT('Ctrl Pts',(0.235383332820519,-0.418064465798881,
-0.730039238604428));
#58320=CARTESIAN_POINT('Ctrl Pts',(0.478641699347353,-0.0329444165423497,
-0.70642185014665));
#58321=CARTESIAN_POINT('Ctrl Pts',(0.290442168180321,0.381872436653063,
-0.682804461688872));
#58322=CARTESIAN_POINT('Ctrl Pts',(-0.159568165198072,0.452461281864222,
-0.659187073231093));
#58323=CARTESIAN_POINT('Ctrl Pts',(-0.46574033073975,0.115191819446649,
-0.635569684773316));
#58324=CARTESIAN_POINT('Ctrl Pts',(-0.352084169032058,-0.325914020622976,
-0.611952296315536));
#58325=CARTESIAN_POINT('Ctrl Pts',(0.0789482169998913,-0.473233969566154,
-0.588334907857759));
#58326=CARTESIAN_POINT('Ctrl Pts',(0.438814986437033,-0.193970664507679,
-0.56471751939998));
#58327=CARTESIAN_POINT('Ctrl Pts',(0.40312451145329,0.260141959498729,-0.541100130942203));
#58328=CARTESIAN_POINT('Ctrl Pts',(0.00404895281978514,0.479757039402292,
-0.517482742484423));
#58329=CARTESIAN_POINT('Ctrl Pts',(-0.398676419816808,0.266908830387348,
-0.493865354026646));
#58330=CARTESIAN_POINT('Ctrl Pts',(-0.442026311464977,-0.186536725659559,
-0.470247965568867));
#58331=CARTESIAN_POINT('Ctrl Pts',(-0.0869242056007438,-0.471834073964581,
-0.446630577111089));
#58332=CARTESIAN_POINT('Ctrl Pts',(0.346533251782296,-0.331810065779944,
-0.423013188653311));
#58333=CARTESIAN_POINT('Ctrl Pts',(0.467618186217581,0.1073146582275,-0.399395800195533));
#58334=CARTESIAN_POINT('Ctrl Pts',(0.167182082036718,0.449703640764164,
-0.375778411737755));
#58335=CARTESIAN_POINT('Ctrl Pts',(-0.283955591511179,0.386720123999693,
-0.352161023279976));
#58336=CARTESIAN_POINT('Ctrl Pts',(-0.479129499296371,-0.0248612322105807,
-0.328543634822198));
#58337=CARTESIAN_POINT('Ctrl Pts',(-0.242405994059508,-0.414032097806954,
-0.30492624636442));
#58338=CARTESIAN_POINT('Ctrl Pts',(0.21282785627909,-0.429985628526655,
-0.281308857906642));
#58339=CARTESIAN_POINT('Ctrl Pts',(0.476213377687744,-0.0583407306117992,
-0.257691469448864));
#58340=CARTESIAN_POINT('Ctrl Pts',(0.310331352318132,0.365893451311033,
-0.234074080991085));
#58341=CARTESIAN_POINT('Ctrl Pts',(-0.135292724422396,0.460304007118841,
-0.210456692533307));
#58342=CARTESIAN_POINT('Ctrl Pts',(-0.458955819664086,0.139785535572616,
-0.186839304075529));
#58343=CARTESIAN_POINT('Ctrl Pts',(-0.36891632732846,-0.30673646455681,
-0.163221915617751));
#58344=CARTESIAN_POINT('Ctrl Pts',(0.053691564255565,-0.476763774871506,
-0.139604527159972));
#58345=CARTESIAN_POINT('Ctrl Pts',(0.427863587514561,-0.217018023145409,
-0.115987138702194));
#58346=CARTESIAN_POINT('Ctrl Pts',(0.416421643175193,0.238337106918288,
-0.0923697502444159));
#58347=CARTESIAN_POINT('Ctrl Pts',(0.0294708192559207,0.478879535587345,
-0.0687523617866379));
#58348=CARTESIAN_POINT('Ctrl Pts',(-0.38378094655697,0.287692953186636,
-0.0451349733288593));
#58349=CARTESIAN_POINT('Ctrl Pts',(-0.451595579558226,-0.162717019166182,
-0.0215175848710814));
#58350=CARTESIAN_POINT('Ctrl Pts',(-0.111329528303481,-0.466661316820024,
0.00209980358669715));
#58351=CARTESIAN_POINT('Ctrl Pts',(0.254098173993848,-0.369056502853948,
0.0217809606348451));
#58352=CARTESIAN_POINT('Ctrl Pts',(0.401718635439753,-0.133621706654172,
0.0375258862733644));
#58353=CARTESIAN_POINT('Ctrl Pts',(0.412529156408264,0.00371036789893213,
0.0453983490926234));
#58354=CARTESIAN_POINT('Ctrl Pts',(0.401015552304393,0.0698300029357225,
0.0493345805022531));
#58355=CARTESIAN_POINT('',(0.236230756092323,-0.331488661006752,-1.6275));
#58356=CARTESIAN_POINT('Ctrl Pts',(0.236230756092322,-0.331488661006753,
-1.6275));
#58357=CARTESIAN_POINT('Ctrl Pts',(0.290886764216325,-0.292538821561541,
-1.62356376859037));
#58358=CARTESIAN_POINT('Ctrl Pts',(0.37970379993858,-0.187236873667965,
-1.61569130577111));
#58359=CARTESIAN_POINT('Ctrl Pts',(0.440127613820048,0.0840015945019269,
-1.59994638013259));
#58360=CARTESIAN_POINT('Ctrl Pts',(0.24873421873435,0.410241802988297,-1.58026522308444));
#58361=CARTESIAN_POINT('Ctrl Pts',(-0.206940906255527,0.433117601952402,
-1.55664783462667));
#58362=CARTESIAN_POINT('Ctrl Pts',(-0.398091847258176,0.170836854465825,
-1.53981984923431));
#58363=CARTESIAN_POINT('Ctrl Pts',(-0.407523402849101,0.0186763741788699,
-1.53086432666122));
#58364=CARTESIAN_POINT('Ctrl Pts',(-0.407376298364278,0.00025708744754576,
-1.52978126690739));
#58365=CARTESIAN_POINT('Ctrl Pts',(0.217490523462168,0.442550970777086,
-1.6275));
#58366=CARTESIAN_POINT('Ctrl Pts',(0.229873785936919,0.435229072478121,
-1.6275));
#58367=CARTESIAN_POINT('Ctrl Pts',(0.241888345109027,0.427350072398723,
-1.6275));
#58368=CARTESIAN_POINT('Ctrl Pts',(0.253489436678505,0.418913037947499,
-1.6275));
#58369=CARTESIAN_POINT('Ctrl Pts',(0.26909400111095,0.40756442933387,-1.6275));
#58370=CARTESIAN_POINT('Ctrl Pts',(0.283951058071679,0.395206382965558,
-1.6275));
#58371=CARTESIAN_POINT('Ctrl Pts',(0.29801362485445,0.38193863087979,-1.6275));
#58372=CARTESIAN_POINT('Ctrl Pts',(0.304179723820256,0.37612103913581,-1.6275));
#58373=CARTESIAN_POINT('Ctrl Pts',(0.310192895551237,0.370128419510018,
-1.6275));
#58374=CARTESIAN_POINT('Ctrl Pts',(0.316048301481397,0.363968703364519,
-1.6275));
#58375=CARTESIAN_POINT('Ctrl Pts',(0.321171057221113,0.358579713836594,
-1.6275));
#58376=CARTESIAN_POINT('Ctrl Pts',(0.326166199023329,0.353069987265224,
-1.6275));
#58377=CARTESIAN_POINT('Ctrl Pts',(0.331029922274408,0.347447220488589,
-1.6275));
#58378=CARTESIAN_POINT('Ctrl Pts',(0.347707626437665,0.328166756523267,
-1.6275));
#58379=CARTESIAN_POINT('Ctrl Pts',(0.362849782089381,0.307552414743918,
-1.6275));
#58380=CARTESIAN_POINT('Ctrl Pts',(0.376336339682191,0.285831520294907,
-1.6275));
#58381=CARTESIAN_POINT('Ctrl Pts',(0.380637168863404,0.278904781870704,
-1.6275));
#58382=CARTESIAN_POINT('Ctrl Pts',(0.384769260466003,0.271865370017674,
-1.6275));
#58383=CARTESIAN_POINT('Ctrl Pts',(0.38872763572935,0.264720378190483,-1.6275));
#58384=CARTESIAN_POINT('Ctrl Pts',(0.392044668436885,0.25873302984448,-1.6275));
#58385=CARTESIAN_POINT('Ctrl Pts',(0.39523614201862,0.252677756188667,-1.6275));
#58386=CARTESIAN_POINT('Ctrl Pts',(0.398296493420852,0.246566077761106,
-1.6275));
#58387=CARTESIAN_POINT('Ctrl Pts',(0.409424515402449,0.224342848155274,
-1.6275));
#58388=CARTESIAN_POINT('Ctrl Pts',(0.418838518533126,0.201346395773246,
-1.6275));
#58389=CARTESIAN_POINT('Ctrl Pts',(0.426426057057826,0.177786853885461,
-1.6275));
#58390=CARTESIAN_POINT('Ctrl Pts',(0.43120915988183,0.162935171621331,-1.6275));
#58391=CARTESIAN_POINT('Ctrl Pts',(0.435265495789154,0.147859358365366,
-1.6275));
#58392=CARTESIAN_POINT('Ctrl Pts',(0.438556181607127,0.132611327460787,
-1.6275));
#58393=CARTESIAN_POINT('Ctrl Pts',(0.441238679389305,0.120181453766761,
-1.6275));
#58394=CARTESIAN_POINT('Ctrl Pts',(0.443412244707011,0.10763710396386,-1.6275));
#58395=CARTESIAN_POINT('Ctrl Pts',(0.445051357081788,0.0950072324793357,
-1.6275));
#58396=CARTESIAN_POINT('Ctrl Pts',(0.445788460122358,0.0893276239201484,
-1.6275));
#58397=CARTESIAN_POINT('Ctrl Pts',(0.446416615420648,0.0836362528176917,
-1.6275));
#58398=CARTESIAN_POINT('Ctrl Pts',(0.446933498575069,0.0779430764704747,
-1.6275));
#58399=CARTESIAN_POINT('Ctrl Pts',(0.448780347169872,0.0576010810951417,
-1.6275));
#58400=CARTESIAN_POINT('Ctrl Pts',(0.449212658849586,0.0372069469719805,
-1.6275));
#58401=CARTESIAN_POINT('Ctrl Pts',(0.448151065409431,0.0168795242984948,
-1.6275));
#58402=CARTESIAN_POINT('Ctrl Pts',(0.447138952308652,-0.00250044736930644,
-1.6275));
#58403=CARTESIAN_POINT('Ctrl Pts',(0.444768459778025,-0.0218202753828828,
-1.6275));
#58404=CARTESIAN_POINT('Ctrl Pts',(0.441093000560412,-0.0409472522530066,
-1.6275));
#58405=CARTESIAN_POINT('Ctrl Pts',(0.439301856685364,-0.0502683099605581,
-1.6275));
#58406=CARTESIAN_POINT('Ctrl Pts',(0.437200494232106,-0.059543425004239,
-1.6275));
#58407=CARTESIAN_POINT('Ctrl Pts',(0.434793501026647,-0.0687561428327804,
-1.6275));
#58408=CARTESIAN_POINT('Ctrl Pts',(0.432942862506225,-0.0758394243529009,
-1.6275));
#58409=CARTESIAN_POINT('Ctrl Pts',(0.430910134545771,-0.0828893859763431,
-1.6275));
#58410=CARTESIAN_POINT('Ctrl Pts',(0.42870580678396,-0.089872919404206,
-1.6275));
#58411=CARTESIAN_POINT('Ctrl Pts',(0.421643420461461,-0.112247273988906,
-1.6275));
#58412=CARTESIAN_POINT('Ctrl Pts',(0.412811785079023,-0.133992695543228,
-1.6275));
#58413=CARTESIAN_POINT('Ctrl Pts',(0.402317198650698,-0.154877686132675,
-1.6275));
#58414=CARTESIAN_POINT('Ctrl Pts',(0.396514879481031,-0.166424723463121,
-1.6275));
#58415=CARTESIAN_POINT('Ctrl Pts',(0.390203399917708,-0.177708329366564,
-1.6275));
#58416=CARTESIAN_POINT('Ctrl Pts',(0.383395506236066,-0.188684900928916,
-1.6275));
#58417=CARTESIAN_POINT('Ctrl Pts',(0.376698831746601,-0.199482150445549,
-1.6275));
#58418=CARTESIAN_POINT('Ctrl Pts',(0.369521760837345,-0.2099823271372,-1.6275));
#58419=CARTESIAN_POINT('Ctrl Pts',(0.361881405765658,-0.220153922075274,
-1.6275));
#58420=CARTESIAN_POINT('Ctrl Pts',(0.357855430998159,-0.225513697135685,
-1.6275));
#58421=CARTESIAN_POINT('Ctrl Pts',(0.35369907565792,-0.230783846841213,
-1.6275));
#58422=CARTESIAN_POINT('Ctrl Pts',(0.349429698861994,-0.235942223748248,
-1.6275));
#58423=CARTESIAN_POINT('Ctrl Pts',(0.334930822084277,-0.253460160141096,
-1.6275));
#58424=CARTESIAN_POINT('Ctrl Pts',(0.319098064470797,-0.269738417169507,
-1.6275));
#58425=CARTESIAN_POINT('Ctrl Pts',(0.302054477316776,-0.284621826293324,
-1.6275));
#58426=CARTESIAN_POINT('Ctrl Pts',(0.285433046055008,-0.299136585390496,
-1.6275));
#58427=CARTESIAN_POINT('Ctrl Pts',(0.267659006720295,-0.312325323179623,
-1.6275));
#58428=CARTESIAN_POINT('Ctrl Pts',(0.248825326281718,-0.323999848365032,
-1.6275));
#58429=CARTESIAN_POINT('Ctrl Pts',(0.244678256323088,-0.326570512810337,
-1.6275));
#58430=CARTESIAN_POINT('Ctrl Pts',(0.24047975853273,-0.329067566916157,
-1.6275));
#58431=CARTESIAN_POINT('Ctrl Pts',(0.236230756092326,-0.33148866100675,
-1.6275));
#58432=CARTESIAN_POINT('Ctrl Pts',(0.485198770445679,0.0844890712341024,
3.15686374347968E-17));
#58433=CARTESIAN_POINT('Ctrl Pts',(0.499129368704262,0.00448926714217439,
-0.00393623140962976));
#58434=CARTESIAN_POINT('Ctrl Pts',(0.492589408531074,-0.0785914928595512,
-0.00787246281925949));
#58435=CARTESIAN_POINT('Ctrl Pts',(0.466993216289305,-0.155739180663015,
-0.0118086942288893));
#58436=CARTESIAN_POINT('Ctrl Pts',(0.441397024047537,-0.232886868466477,
-0.0157449256385189));
#58437=CARTESIAN_POINT('Ctrl Pts',(0.396744599737189,-0.304101484071678,
-0.0196811570481487));
#58438=CARTESIAN_POINT('Ctrl Pts',(0.33750030762947,-0.359450861903929,
-0.0236173884577784));
#58439=CARTESIAN_POINT('Ctrl Pts',(0.219011723414032,-0.470149617568429,
-0.0314898512770378));
#58440=CARTESIAN_POINT('Ctrl Pts',(0.0421556680091084,-0.517387422141126,
-0.039362314096297));
#58441=CARTESIAN_POINT('Ctrl Pts',(-0.114888430709592,-0.479714686793065,
-0.0472347769155564));
#58442=CARTESIAN_POINT('Ctrl Pts',(-0.271932529428293,-0.442041951445003,
-0.0551072397348157));
#58443=CARTESIAN_POINT('Ctrl Pts',(-0.40916467146077,-0.319458676176184,
-0.0629797025540751));
#58444=CARTESIAN_POINT('Ctrl Pts',(-0.464105638373042,-0.167339985606525,
-0.0708521653733345));
#58445=CARTESIAN_POINT('Ctrl Pts',(-0.483329384560808,-0.11411392748862,
-0.073606726052103));
#58446=CARTESIAN_POINT('Ctrl Pts',(-0.492478324217231,-0.057271885098475,
-0.0763612867308716));
#58447=CARTESIAN_POINT('Ctrl Pts',(-0.492093596265288,-0.000318355522334279,
-0.0791158474096402));
#58448=CARTESIAN_POINT('Origin',(0.,0.,-1.90478126690739));
#58449=CARTESIAN_POINT('',(-0.236230756092322,-0.331488661006753,-1.6275));
#58450=CARTESIAN_POINT('Ctrl Pts',(-0.236809196450266,-0.331691137924159,
-1.6275));
#58451=CARTESIAN_POINT('Ctrl Pts',(-0.13719578617953,-0.401752132096373,
-1.62032747170964));
#58452=CARTESIAN_POINT('Ctrl Pts',(0.143417983013933,-0.451519069382718,
-1.60528248060002));
#58453=CARTESIAN_POINT('Ctrl Pts',(0.458329322630197,-0.141383602456536,
-1.58236502667114));
#58454=CARTESIAN_POINT('Ctrl Pts',(0.37009909626306,0.305320664636155,-1.55874763821336));
#58455=CARTESIAN_POINT('Ctrl Pts',(-0.0519477178791621,0.476983193860142,
-1.53513024975558));
#58456=CARTESIAN_POINT('Ctrl Pts',(-0.361819606070115,0.263531195926594,
-1.51562061471533));
#58457=CARTESIAN_POINT('Ctrl Pts',(-0.406474643984443,0.0644690927340416,
-1.50398344249434));
#58458=CARTESIAN_POINT('Ctrl Pts',(-0.406409642899809,4.34815695103258E-5,
-1.50021873309261));
#58459=CARTESIAN_POINT('Origin',(0.,0.,-1.6275));
#58460=CARTESIAN_POINT('Ctrl Pts',(-0.179217368492188,0.365473442716068,
-1.67683458050225));
#58461=CARTESIAN_POINT('Ctrl Pts',(-0.239476803591809,0.33592399774102,
-1.67289834909262));
#58462=CARTESIAN_POINT('Ctrl Pts',(-0.344225195791861,0.246456180713373,
-1.66502588627336));
#58463=CARTESIAN_POINT('Ctrl Pts',(-0.447929722889861,-0.0113560346107791,
-1.64928096063485));
#58464=CARTESIAN_POINT('Ctrl Pts',(-0.312098364353949,-0.364364201240606,
-1.6295998035867));
#58465=CARTESIAN_POINT('Ctrl Pts',(0.133800103086114,-0.460991086763511,
-1.60598241512892));
#58466=CARTESIAN_POINT('Ctrl Pts',(0.458329322630197,-0.141383602456536,
-1.58236502667114));
#58467=CARTESIAN_POINT('Ctrl Pts',(0.37009909626306,0.305320664636155,-1.55874763821336));
#58468=CARTESIAN_POINT('Ctrl Pts',(-0.0519477178791621,0.476983193860142,
-1.53513024975558));
#58469=CARTESIAN_POINT('Ctrl Pts',(-0.427063128313673,0.218588880389641,
-1.51151286129781));
#58470=CARTESIAN_POINT('Ctrl Pts',(-0.417269064836094,-0.236797291451368,
-1.48789547284003));
#58471=CARTESIAN_POINT('Ctrl Pts',(-0.0313114294066901,-0.478754704371251,
-1.46427808438225));
#58472=CARTESIAN_POINT('Ctrl Pts',(0.382856292689895,-0.28913914624985,
-1.44066069592447));
#58473=CARTESIAN_POINT('Ctrl Pts',(0.451916785881922,0.161105773860312,
-1.41704330746669));
#58474=CARTESIAN_POINT('Ctrl Pts',(0.113605814801219,0.466130064220589,
-1.39342591900891));
#58475=CARTESIAN_POINT('Ctrl Pts',(-0.327109807248698,0.350972856030287,
-1.36980853055114));
#58476=CARTESIAN_POINT('Ctrl Pts',(-0.472962705865375,-0.0805578494149952,
-1.34619114209336));
#58477=CARTESIAN_POINT('Ctrl Pts',(-0.192476314157182,-0.439472483121615,
-1.32257375363558));
#58478=CARTESIAN_POINT('Ctrl Pts',(0.26151206617616,-0.402236929927433,
-1.2989563651778));
#58479=CARTESIAN_POINT('Ctrl Pts',(0.479768010181106,-0.00241651336352132,
-1.27533897672002));
#58480=CARTESIAN_POINT('Ctrl Pts',(0.265550697114187,0.399582270810862,
-1.25172158826225));
#58481=CARTESIAN_POINT('Ctrl Pts',(-0.188039671187417,0.44138898578519,
-1.22810419980447));
#58482=CARTESIAN_POINT('Ctrl Pts',(-0.472127066500839,0.0853182174774826,
-1.20448681134669));
#58483=CARTESIAN_POINT('Ctrl Pts',(-0.330628982897472,-0.347660232609956,
-1.18086942288891));
#58484=CARTESIAN_POINT('Ctrl Pts',(0.108905154226429,-0.467250284345138,
-1.15725203443113));
#58485=CARTESIAN_POINT('Ctrl Pts',(0.450269851614892,-0.165650906977965,
-1.13363464597335));
#58486=CARTESIAN_POINT('Ctrl Pts',(0.385751642062305,0.285269753596648,
-1.11001725751558));
#58487=CARTESIAN_POINT('Ctrl Pts',(-0.0264913736532199,0.479042136709866,
-1.0863998690578));
#58488=CARTESIAN_POINT('Ctrl Pts',(-0.414854497170337,0.240995659681838,
-1.06278248060002));
#58489=CARTESIAN_POINT('Ctrl Pts',(-0.429258875462494,-0.214289476063294,
-1.03916509214224));
#58490=CARTESIAN_POINT('Ctrl Pts',(-0.0567200932042535,-0.476409480116128,
-1.01554770368446));
#58491=CARTESIAN_POINT('Ctrl Pts',(0.366947398132722,-0.309083756844029,
-0.991930315226685));
#58492=CARTESIAN_POINT('Ctrl Pts',(0.459840631415877,0.136856696679471,
-0.968312926768907));
#58493=CARTESIAN_POINT('Ctrl Pts',(0.138223653062154,0.459431587358633,
-0.944695538311129));
#58494=CARTESIAN_POINT('Ctrl Pts',(-0.307991091943065,0.367864987482187,
-0.92107814985335));
#58495=CARTESIAN_POINT('Ctrl Pts',(-0.476576058306532,-0.0553030051489224,
-0.897460761395572));
#58496=CARTESIAN_POINT('Ctrl Pts',(-0.215565140139133,-0.428619682337017,
-0.873843372937795));
#58497=CARTESIAN_POINT('Ctrl Pts',(0.239760820588477,-0.415569381260058,
-0.850225984480015));
#58498=CARTESIAN_POINT('Ctrl Pts',(0.478961233248966,-0.0279159233190857,
-0.826608596022238));
#58499=CARTESIAN_POINT('Ctrl Pts',(0.286415713505782,0.384901546875125,
-0.802991207564458));
#58500=CARTESIAN_POINT('Ctrl Pts',(-0.164311075821679,0.450760504139189,
-0.779373819106682));
#58501=CARTESIAN_POINT('Ctrl Pts',(-0.466924335892738,0.110294271304891,
-0.755756430648903));
#58502=CARTESIAN_POINT('Ctrl Pts',(-0.348641981099809,-0.329593584196537,
-0.732139042191125));
#58503=CARTESIAN_POINT('Ctrl Pts',(0.0839137360252065,-0.472378711028833,
-0.708521653733346));
#58504=CARTESIAN_POINT('Ctrl Pts',(0.440827811035869,-0.189351532231765,
-0.684904265275568));
#58505=CARTESIAN_POINT('Ctrl Pts',(0.400370238591211,0.264361180523987,
-0.66128687681779));
#58506=CARTESIAN_POINT('Ctrl Pts',(-0.000989657323522311,0.479773052904378,
-0.637669488360011));
#58507=CARTESIAN_POINT('Ctrl Pts',(-0.401457455034637,0.262707201281293,
-0.614052099902234));
#58508=CARTESIAN_POINT('Ctrl Pts',(-0.440042888698431,-0.191168558417772,
-0.590434711444455));
#58509=CARTESIAN_POINT('Ctrl Pts',(-0.0819642213078552,-0.472720877576032,
-0.566817322986677));
#58510=CARTESIAN_POINT('Ctrl Pts',(0.349998754832881,-0.328152455226764,
-0.543199934528899));
#58511=CARTESIAN_POINT('Ctrl Pts',(0.466465341731633,0.112219631976251,
-0.51958254607112));
#58512=CARTESIAN_POINT('Ctrl Pts',(0.162450064697528,0.451434533625857,
-0.495965157613343));
#58513=CARTESIAN_POINT('Ctrl Pts',(-0.288001193431347,0.383716663357668,
-0.472347769155564));
#58514=CARTESIAN_POINT('Ctrl Pts',(-0.47884198251775,-0.0298916458432992,
-0.448730380697786));
#58515=CARTESIAN_POINT('Ctrl Pts',(-0.238044360971215,-0.416554973675746,
-0.425112992240007));
#58516=CARTESIAN_POINT('Ctrl Pts',(0.217331606272519,-0.427726730571028,
-0.40149560378223));
#58517=CARTESIAN_POINT('Ctrl Pts',(0.476800102102078,-0.0533363964720061,
-0.377878215324451));
#58518=CARTESIAN_POINT('Ctrl Pts',(0.306470944705725,0.369132435561808,
-0.354260826866673));
#58519=CARTESIAN_POINT('Ctrl Pts',(-0.140118061818574,0.458857512735786,
-0.330643438408895));
#58520=CARTESIAN_POINT('Ctrl Pts',(-0.460400941337906,0.134958307945479,
-0.307026049951117));
#58521=CARTESIAN_POINT('Ctrl Pts',(-0.365669879310811,-0.310594683296022,
-0.283408661493338));
#58522=CARTESIAN_POINT('Ctrl Pts',(0.0586864453268738,-0.476171978247222,
-0.259791273035561));
#58523=CARTESIAN_POINT('Ctrl Pts',(0.430136573097502,-0.212515682316106,
-0.236173884577782));
#58524=CARTESIAN_POINT('Ctrl Pts',(0.413861933598501,0.242703054136536,
-0.212556496120004));
#58525=CARTESIAN_POINT('Ctrl Pts',(0.0245048656306335,0.479151271800793,
-0.188939107662225));
#58526=CARTESIAN_POINT('Ctrl Pts',(-0.386906026396146,0.283668364350701,
-0.165321719204448));
#58527=CARTESIAN_POINT('Ctrl Pts',(-0.449619579691367,-0.167492585435993,
-0.141704330746669));
#58528=CARTESIAN_POINT('Ctrl Pts',(-0.106905499254799,-0.467723490470255,
-0.118086942288891));
#58529=CARTESIAN_POINT('Ctrl Pts',(0.331923550485991,-0.346239581300314,
-0.0944695538311125));
#58530=CARTESIAN_POINT('Ctrl Pts',(0.472036117814807,0.0871616494771883,
-0.0708521653733347));
#58531=CARTESIAN_POINT('Ctrl Pts',(0.18569067875618,0.442363687480316,-0.0472347769155563));
#58532=CARTESIAN_POINT('Ctrl Pts',(-0.190742685458467,0.405446943649056,
-0.0275536198674078));
#58533=CARTESIAN_POINT('Ctrl Pts',(-0.374661374851549,0.197130638471333,
-0.0118086942288892));
#58534=CARTESIAN_POINT('Ctrl Pts',(-0.40764782825114,0.0633823306528579,
-0.00393623140962957));
#58535=CARTESIAN_POINT('Ctrl Pts',(-0.407032914766026,-0.00372944996921217,
2.22044604925031E-16));
#58536=CARTESIAN_POINT('Ctrl Pts',(-0.19175810807181,0.391047455474607,
-1.66038972033484));
#58537=CARTESIAN_POINT('Ctrl Pts',(-0.256234198561238,0.359430287391736,
-1.65645348892521));
#58538=CARTESIAN_POINT('Ctrl Pts',(-0.368312361971621,0.263701957761204,
-1.64858102610595));
#58539=CARTESIAN_POINT('Ctrl Pts',(-0.479273615794859,-0.0121506734000261,
-1.63283610046743));
#58540=CARTESIAN_POINT('Ctrl Pts',(-0.333937454747469,-0.389860594800781,
-1.61315494341928));
#58541=CARTESIAN_POINT('Ctrl Pts',(0.14316276844967,-0.493248948913077,
-1.5895375549615));
#58542=CARTESIAN_POINT('Ctrl Pts',(0.490400927771866,-0.151276923367082,
-1.56592016650372));
#58543=CARTESIAN_POINT('Ctrl Pts',(0.395996789237453,0.326685485332349,
-1.54230277804595));
#58544=CARTESIAN_POINT('Ctrl Pts',(-0.0555827606607796,0.510360104080303,
-1.51868538958816));
#58545=CARTESIAN_POINT('Ctrl Pts',(-0.456946880771931,0.23388464244123,
-1.49506800113039));
#58546=CARTESIAN_POINT('Ctrl Pts',(-0.446467477471926,-0.253367187495685,
-1.47145061267261));
#58547=CARTESIAN_POINT('Ctrl Pts',(-0.0335024474166019,-0.512255576081133,
-1.44783322421483));
#58548=CARTESIAN_POINT('Ctrl Pts',(0.409646670784601,-0.309371664815999,
-1.42421583575705));
#58549=CARTESIAN_POINT('Ctrl Pts',(0.483539673613659,0.17237915417916,-1.40059844729927));
#58550=CARTESIAN_POINT('Ctrl Pts',(0.121555384366601,0.498747526438702,
-1.3769810588415));
#58551=CARTESIAN_POINT('Ctrl Pts',(-0.349999323712195,0.375532189894095,
-1.35336367038372));
#58552=CARTESIAN_POINT('Ctrl Pts',(-0.506058282343447,-0.0861948868244116,
-1.32974628192594));
#58553=CARTESIAN_POINT('Ctrl Pts',(-0.205944848771876,-0.470224580474718,
-1.30612889346816));
#58554=CARTESIAN_POINT('Ctrl Pts',(0.279811379163714,-0.430383468569123,
-1.28251150501038));
#58555=CARTESIAN_POINT('Ctrl Pts',(0.51333978798889,-0.00258560894302878,
-1.25889411655261));
#58556=CARTESIAN_POINT('Ctrl Pts',(0.284132613396715,0.427543049618369,
-1.23527672809483));
#58557=CARTESIAN_POINT('Ctrl Pts',(-0.201197751605845,0.472275190457298,
-1.21165933963705));
#58558=CARTESIAN_POINT('Ctrl Pts',(-0.505164169094702,0.0912883617541506,
-1.18804195117927));
#58559=CARTESIAN_POINT('Ctrl Pts',(-0.353764753759849,-0.371987765571934,
-1.16442456272149));
#58560=CARTESIAN_POINT('Ctrl Pts',(0.116525794957417,-0.499946133992841,
-1.14080717426372));
#58561=CARTESIAN_POINT('Ctrl Pts',(0.481777495082518,-0.177242333093732,
-1.11718978580594));
#58562=CARTESIAN_POINT('Ctrl Pts',(0.412744622297515,0.305231511320786,
-1.09357239734816));
#58563=CARTESIAN_POINT('Ctrl Pts',(-0.0283451081482987,0.512563121504412,
-1.06995500889038));
#58564=CARTESIAN_POINT('Ctrl Pts',(-0.443883950376908,0.257859336641929,
-1.0463376204326));
#58565=CARTESIAN_POINT('Ctrl Pts',(-0.459296275379188,-0.22928438719592,
-1.02272023197482));
#58566=CARTESIAN_POINT('Ctrl Pts',(-0.0606890830616055,-0.509746244703545,
-0.999102843517047));
#58567=CARTESIAN_POINT('Ctrl Pts',(0.39262455095624,-0.330711900006067,
-0.975485455059267));
#58568=CARTESIAN_POINT('Ctrl Pts',(0.492017990425408,0.146433247251684,
-0.95186806660149));
#58569=CARTESIAN_POINT('Ctrl Pts',(0.147895856439432,0.491580323500626,
-0.92825067814371));
#58570=CARTESIAN_POINT('Ctrl Pts',(-0.329542775852931,0.393606348642041,
-0.904633289685933));
#58571=CARTESIAN_POINT('Ctrl Pts',(-0.509924479206744,-0.059172834236236,
-0.881015901228153));
#58572=CARTESIAN_POINT('Ctrl Pts',(-0.230649315895502,-0.458612354699706,
-0.857398512770378));
#58573=CARTESIAN_POINT('Ctrl Pts',(0.256538089653934,-0.44464885849764,
-0.833781124312597));
#58574=CARTESIAN_POINT('Ctrl Pts',(0.512476556821929,-0.0298693407105762,
-0.81016373585482));
#58575=CARTESIAN_POINT('Ctrl Pts',(0.306457659801545,0.411835041679595,
-0.786546347397041));
#58576=CARTESIAN_POINT('Ctrl Pts',(-0.175808747220738,0.482302481028755,
-0.762928958939263));
#58577=CARTESIAN_POINT('Ctrl Pts',(-0.499597377289809,0.118012115536152,
-0.739311570481486));
#58578=CARTESIAN_POINT('Ctrl Pts',(-0.373038211935482,-0.352656903010436,
-0.715694182023706));
#58579=CARTESIAN_POINT('Ctrl Pts',(0.089785601679182,-0.505433422454468,
-0.692076793565929));
#58580=CARTESIAN_POINT('Ctrl Pts',(0.47167474749168,-0.20260141015766,-0.66845940510815));
#58581=CARTESIAN_POINT('Ctrl Pts',(0.428386155462701,0.282859860355108,
-0.644842016650373));
#58582=CARTESIAN_POINT('Ctrl Pts',(-0.0010589086180337,0.513345183576842,
-0.621224628192593));
#58583=CARTESIAN_POINT('Ctrl Pts',(-0.429549449902351,0.281090143875969,
-0.597607239734817));
#58584=CARTESIAN_POINT('Ctrl Pts',(-0.470834900195202,-0.204545582793808,
-0.573989851277037));
#58585=CARTESIAN_POINT('Ctrl Pts',(-0.0876996696235889,-0.505799532113863,
-0.55037246281926));
#58586=CARTESIAN_POINT('Ctrl Pts',(0.374489925942464,-0.351114931007076,
-0.526755074361481));
#58587=CARTESIAN_POINT('Ctrl Pts',(0.499106265001477,0.120072203365817,
-0.503137685903703));
#58588=CARTESIAN_POINT('Ctrl Pts',(0.173817511799362,0.483023675744621,
-0.479520297445925));
#58589=CARTESIAN_POINT('Ctrl Pts',(-0.308154083722225,0.41056724591011,
-0.455902908988146));
#58590=CARTESIAN_POINT('Ctrl Pts',(-0.512348961517989,-0.0319833144649325,
-0.432285520530369));
#58591=CARTESIAN_POINT('Ctrl Pts',(-0.254701520734547,-0.445703417765819,
-0.40866813207259));
#58592=CARTESIAN_POINT('Ctrl Pts',(0.232539390538157,-0.45765691861287,
-0.385050743614812));
#58593=CARTESIAN_POINT('Ctrl Pts',(0.510164200472157,-0.0570686120708559,
-0.361433355157034));
#58594=CARTESIAN_POINT('Ctrl Pts',(0.327916256276871,0.39496248643087,-0.337815966699255));
#58595=CARTESIAN_POINT('Ctrl Pts',(-0.149922826493179,0.490966077992531,
-0.314198578241478));
#58596=CARTESIAN_POINT('Ctrl Pts',(-0.492617508047421,0.14440201872134,
-0.290581189783699));
#58597=CARTESIAN_POINT('Ctrl Pts',(-0.391257637724691,-0.332328553572109,
-0.266963801325921));
#58598=CARTESIAN_POINT('Ctrl Pts',(0.0627930307202971,-0.509492123635771,
-0.243346412868143));
#58599=CARTESIAN_POINT('Ctrl Pts',(0.460235389926868,-0.227386472189515,
-0.219729024410364));
#58600=CARTESIAN_POINT('Ctrl Pts',(0.442821932145767,0.259686206063789,
-0.196111635952586));
#58601=CARTESIAN_POINT('Ctrl Pts',(0.0262195941800665,0.512679893325895,
-0.172494247494808));
#58602=CARTESIAN_POINT('Ctrl Pts',(-0.413979784702292,0.303518064824655,
-0.14887685903703));
#58603=CARTESIAN_POINT('Ctrl Pts',(-0.481081720365837,-0.179212883045216,
-0.125259470579251));
#58604=CARTESIAN_POINT('Ctrl Pts',(-0.114386214082072,-0.500452452727704,
-0.101642082121473));
#58605=CARTESIAN_POINT('Ctrl Pts',(0.35514990874585,-0.370467704153455,
-0.0780246936636948));
#58606=CARTESIAN_POINT('Ctrl Pts',(0.505066856272224,0.0932607879514328,
-0.0544073052059168));
#58607=CARTESIAN_POINT('Ctrl Pts',(0.198684388373932,0.473318096926487,
-0.0307899167481386));
#58608=CARTESIAN_POINT('Ctrl Pts',(-0.204089909364149,0.433818103076491,
-0.01110875969999));
#58609=CARTESIAN_POINT('Ctrl Pts',(-0.400878313377581,0.210924859539488,
0.00463616593852857));
#58610=CARTESIAN_POINT('Ctrl Pts',(-0.436172994630421,0.0678175107325275,
0.0125086287577882));
#58611=CARTESIAN_POINT('Ctrl Pts',(-0.43551505255971,-0.00399041831861005,
0.016444860167418));
#58612=CARTESIAN_POINT('Ctrl Pts',(-0.204298847651432,0.416621468233145,
-1.64394486016742));
#58613=CARTESIAN_POINT('Ctrl Pts',(-0.272991593530667,0.382936577042452,
-1.64000862875779));
#58614=CARTESIAN_POINT('Ctrl Pts',(-0.39239952815138,0.280947734809036,
-1.63213616593853));
#58615=CARTESIAN_POINT('Ctrl Pts',(-0.510617508699857,-0.0129453121892735,
-1.61639124030001));
#58616=CARTESIAN_POINT('Ctrl Pts',(-0.355776545140989,-0.415356988360956,
-1.59671008325186));
#58617=CARTESIAN_POINT('Ctrl Pts',(0.152525433813226,-0.525506811062644,
-1.57309269479408));
#58618=CARTESIAN_POINT('Ctrl Pts',(0.522472532913535,-0.161170244277627,
-1.5494753063363));
#58619=CARTESIAN_POINT('Ctrl Pts',(0.421894482211846,0.348050306028543,
-1.52585791787853));
#58620=CARTESIAN_POINT('Ctrl Pts',(-0.0592178034423973,0.543737014300464,
-1.50224052942075));
#58621=CARTESIAN_POINT('Ctrl Pts',(-0.486830633230189,0.249180404492818,
-1.47862314096297));
#58622=CARTESIAN_POINT('Ctrl Pts',(-0.475665890107758,-0.269937083540001,
-1.45500575250519));
#58623=CARTESIAN_POINT('Ctrl Pts',(-0.0356934654265134,-0.545756447791016,
-1.43138836404741));
#58624=CARTESIAN_POINT('Ctrl Pts',(0.436437048879306,-0.329604183382146,
-1.40777097558964));
#58625=CARTESIAN_POINT('Ctrl Pts',(0.515162561345397,0.183652534498008,
-1.38415358713186));
#58626=CARTESIAN_POINT('Ctrl Pts',(0.129504953931983,0.531364988656815,
-1.36053619867408));
#58627=CARTESIAN_POINT('Ctrl Pts',(-0.372888840175693,0.400091523757903,
-1.3369188102163));
#58628=CARTESIAN_POINT('Ctrl Pts',(-0.539153858821517,-0.0918319242338282,
-1.31330142175852));
#58629=CARTESIAN_POINT('Ctrl Pts',(-0.21941338338657,-0.500976677827821,
-1.28968403330075));
#58630=CARTESIAN_POINT('Ctrl Pts',(0.298110692151268,-0.458530007210813,
-1.26606664484297));
#58631=CARTESIAN_POINT('Ctrl Pts',(0.546911565796673,-0.0027547045225358,
-1.24244925638519));
#58632=CARTESIAN_POINT('Ctrl Pts',(0.302714529679244,0.455503828425875,
-1.21883186792741));
#58633=CARTESIAN_POINT('Ctrl Pts',(-0.214355832024272,0.503161395129407,
-1.19521447946963));
#58634=CARTESIAN_POINT('Ctrl Pts',(-0.538201271688565,0.0972585060308188,
-1.17159709101185));
#58635=CARTESIAN_POINT('Ctrl Pts',(-0.376900524622225,-0.396315298533912,
-1.14797970255407));
#58636=CARTESIAN_POINT('Ctrl Pts',(0.124146435688405,-0.532641983640544,
-1.1243623140963));
#58637=CARTESIAN_POINT('Ctrl Pts',(0.513285138550144,-0.1888337592095,-1.10074492563852));
#58638=CARTESIAN_POINT('Ctrl Pts',(0.439737602532723,0.325193269044925,
-1.07712753718074));
#58639=CARTESIAN_POINT('Ctrl Pts',(-0.0301988426433773,0.546084106298956,
-1.05351014872296));
#58640=CARTESIAN_POINT('Ctrl Pts',(-0.472913403583479,0.27472301360202,
-1.02989276026519));
#58641=CARTESIAN_POINT('Ctrl Pts',(-0.489333675295882,-0.244279298328546,
-1.0062753718074));
#58642=CARTESIAN_POINT('Ctrl Pts',(-0.0646580729189583,-0.54308300929096,
-0.982657983349628));
#58643=CARTESIAN_POINT('Ctrl Pts',(0.418301703779759,-0.352340043168106,
-0.959040594891849));
#58644=CARTESIAN_POINT('Ctrl Pts',(0.524195349434937,0.156009797823898,
-0.935423206434071));
#58645=CARTESIAN_POINT('Ctrl Pts',(0.157568059816711,0.523729059642619,
-0.911805817976294));
#58646=CARTESIAN_POINT('Ctrl Pts',(-0.351094459762798,0.419347709801893,
-0.888188429518514));
#58647=CARTESIAN_POINT('Ctrl Pts',(-0.543272900106956,-0.0630426633235498,
-0.864571041060736));
#58648=CARTESIAN_POINT('Ctrl Pts',(-0.245733491651872,-0.488605027062394,
-0.840953652602959));
#58649=CARTESIAN_POINT('Ctrl Pts',(0.273315358719392,-0.473728335735222,
-0.81733626414518));
#58650=CARTESIAN_POINT('Ctrl Pts',(0.545991880394893,-0.031822758102066,
-0.793718875687402));
#58651=CARTESIAN_POINT('Ctrl Pts',(0.326499606097308,0.438768536484064,
-0.770101487229623));
#58652=CARTESIAN_POINT('Ctrl Pts',(-0.187306418619796,0.513844457918322,
-0.746484098771846));
#58653=CARTESIAN_POINT('Ctrl Pts',(-0.53227041868688,0.125729959767414,
-0.722866710314067));
#58654=CARTESIAN_POINT('Ctrl Pts',(-0.397434442771153,-0.375720221824335,
-0.699249321856289));
#58655=CARTESIAN_POINT('Ctrl Pts',(0.0956574673331571,-0.538488133880103,
-0.675631933398511));
#58656=CARTESIAN_POINT('Ctrl Pts',(0.502521683947491,-0.215851288083556,
-0.652014544940732));
#58657=CARTESIAN_POINT('Ctrl Pts',(0.456402072334192,0.301358540186229,
-0.628397156482955));
#58658=CARTESIAN_POINT('Ctrl Pts',(-0.00112815991254549,0.546917314249306,
-0.604779768025176));
#58659=CARTESIAN_POINT('Ctrl Pts',(-0.457641444770064,0.299473086470645,
-0.581162379567398));
#58660=CARTESIAN_POINT('Ctrl Pts',(-0.501626911691973,-0.217922607169844,
-0.55754499110962));
#58661=CARTESIAN_POINT('Ctrl Pts',(-0.0934351179393231,-0.538878186651692,
-0.533927602651841));
#58662=CARTESIAN_POINT('Ctrl Pts',(0.398981097052048,-0.374077406787389,
-0.510310214194063));
#58663=CARTESIAN_POINT('Ctrl Pts',(0.531747188271319,0.127924774755383,
-0.486692825736285));
#58664=CARTESIAN_POINT('Ctrl Pts',(0.185184958901198,0.514612817863385,
-0.463075437278508));
#58665=CARTESIAN_POINT('Ctrl Pts',(-0.328306974013104,0.437417828462551,
-0.439458048820728));
#58666=CARTESIAN_POINT('Ctrl Pts',(-0.545855940518228,-0.0340749830865658,
-0.415840660362951));
#58667=CARTESIAN_POINT('Ctrl Pts',(-0.271358680497878,-0.474851861855891,
-0.392223271905172));
#58668=CARTESIAN_POINT('Ctrl Pts',(0.247747174803796,-0.487587106654712,
-0.368605883447394));
#58669=CARTESIAN_POINT('Ctrl Pts',(0.543528298842236,-0.0608008276697055,
-0.344988494989616));
#58670=CARTESIAN_POINT('Ctrl Pts',(0.349361567848018,0.420792537299932,
-0.321371106531837));
#58671=CARTESIAN_POINT('Ctrl Pts',(-0.159727591167785,0.523074643249275,
-0.29775371807406));
#58672=CARTESIAN_POINT('Ctrl Pts',(-0.524834074756935,0.153845729497202,
-0.274136329616281));
#58673=CARTESIAN_POINT('Ctrl Pts',(-0.416845396138572,-0.354062423848196,
-0.250518941158503));
#58674=CARTESIAN_POINT('Ctrl Pts',(0.0668996161137206,-0.542812269024319,
-0.226901552700725));
#58675=CARTESIAN_POINT('Ctrl Pts',(0.490334206756235,-0.242257262062924,
-0.203284164242946));
#58676=CARTESIAN_POINT('Ctrl Pts',(0.471781930693032,0.276669357991042,
-0.179666775785169));
#58677=CARTESIAN_POINT('Ctrl Pts',(0.0279343227294995,0.546208514850997,
-0.15604938732739));
#58678=CARTESIAN_POINT('Ctrl Pts',(-0.441053543008437,0.323367765298609,
-0.132431998869612));
#58679=CARTESIAN_POINT('Ctrl Pts',(-0.512543861040306,-0.19093318065444,
-0.108814610411833));
#58680=CARTESIAN_POINT('Ctrl Pts',(-0.121866928909346,-0.533181414985152,
-0.0851972219540557));
#58681=CARTESIAN_POINT('Ctrl Pts',(0.378376267005709,-0.394695827006596,
-0.0615798334962771));
#58682=CARTESIAN_POINT('Ctrl Pts',(0.538097594729642,0.0993599264256769,
-0.037962445038499));
#58683=CARTESIAN_POINT('Ctrl Pts',(0.211678097991684,0.504272506372659,
-0.0143450565807208));
#58684=CARTESIAN_POINT('Ctrl Pts',(-0.217437133269832,0.462189262503926,
0.00533610046742779));
#58685=CARTESIAN_POINT('Ctrl Pts',(-0.427095251903613,0.224719080607643,
0.0210810261059464));
#58686=CARTESIAN_POINT('Ctrl Pts',(-0.464698161009703,0.0722526908121974,
0.028953488925206));
#58687=CARTESIAN_POINT('Ctrl Pts',(-0.463997190353394,-0.00425138666800794,
0.0328897203348358));
#58688=CARTESIAN_POINT('Ctrl Pts',(-0.216839587231054,0.442195480991683,
-1.6275));
#58689=CARTESIAN_POINT('Ctrl Pts',(-0.289748988500096,0.406442866693167,
-1.62356376859037));
#58690=CARTESIAN_POINT('Ctrl Pts',(-0.41648669433114,0.298193511856867,
-1.61569130577111));
#58691=CARTESIAN_POINT('Ctrl Pts',(-0.541961401604855,-0.0137399509785201,
-1.59994638013259));
#58692=CARTESIAN_POINT('Ctrl Pts',(-0.377615635534509,-0.440853381921132,
-1.58026522308444));
#58693=CARTESIAN_POINT('Ctrl Pts',(0.161888099176782,-0.55776467321221,
-1.55664783462667));
#58694=CARTESIAN_POINT('Ctrl Pts',(0.554544138055205,-0.171063565188174,
-1.53303044616889));
#58695=CARTESIAN_POINT('Ctrl Pts',(0.447792175186239,0.369415126724738,
-1.50941305771111));
#58696=CARTESIAN_POINT('Ctrl Pts',(-0.0628528462240147,0.577113924520625,
-1.48579566925333));
#58697=CARTESIAN_POINT('Ctrl Pts',(-0.516714385688448,0.264476166544406,
-1.46217828079555));
#58698=CARTESIAN_POINT('Ctrl Pts',(-0.504864302743589,-0.286506979584318,
-1.43856089233777));
#58699=CARTESIAN_POINT('Ctrl Pts',(-0.0378844834364257,-0.579257319500899,
-1.41494350388));
#58700=CARTESIAN_POINT('Ctrl Pts',(0.463227426974013,-0.349836701948294,
-1.39132611542222));
#58701=CARTESIAN_POINT('Ctrl Pts',(0.546785449077134,0.194925914816856,
-1.36770872696444));
#58702=CARTESIAN_POINT('Ctrl Pts',(0.137454523497365,0.563982450874928,
-1.34409133850666));
#58703=CARTESIAN_POINT('Ctrl Pts',(-0.395778356639189,0.424650857621712,
-1.32047395004888));
#58704=CARTESIAN_POINT('Ctrl Pts',(-0.572249435299589,-0.0974689616432452,
-1.2968565615911));
#58705=CARTESIAN_POINT('Ctrl Pts',(-0.232881918001264,-0.531728775180923,
-1.27323917313333));
#58706=CARTESIAN_POINT('Ctrl Pts',(0.316410005138821,-0.486676545852504,
-1.24962178467555));
#58707=CARTESIAN_POINT('Ctrl Pts',(0.580483343604457,-0.00292380010204273,
-1.22600439621777));
#58708=CARTESIAN_POINT('Ctrl Pts',(0.321296445961772,0.483464607233382,
-1.20238700775999));
#58709=CARTESIAN_POINT('Ctrl Pts',(-0.227513912442699,0.534047599801515,
-1.17876961930221));
#58710=CARTESIAN_POINT('Ctrl Pts',(-0.571238374282429,0.103228650307487,
-1.15515223084444));
#58711=CARTESIAN_POINT('Ctrl Pts',(-0.400036295484601,-0.42064283149589,
-1.13153484238666));
#58712=CARTESIAN_POINT('Ctrl Pts',(0.131767076419393,-0.565337833288247,
-1.10791745392888));
#58713=CARTESIAN_POINT('Ctrl Pts',(0.544792782017771,-0.200425185325267,
-1.0843000654711));
#58714=CARTESIAN_POINT('Ctrl Pts',(0.466730582767932,0.345155026769063,
-1.06068267701332));
#58715=CARTESIAN_POINT('Ctrl Pts',(-0.0320525771384556,0.579605091093501,
-1.03706528855555));
#58716=CARTESIAN_POINT('Ctrl Pts',(-0.50194285679005,0.291586690562111,
-1.01344790009777));
#58717=CARTESIAN_POINT('Ctrl Pts',(-0.519371075212576,-0.259274209461172,
-0.989830511639989));
#58718=CARTESIAN_POINT('Ctrl Pts',(-0.0686270627763104,-0.576419773878377,
-0.966213123182209));
#58719=CARTESIAN_POINT('Ctrl Pts',(0.443978856603277,-0.373968186330145,
-0.942595734724432));
#58720=CARTESIAN_POINT('Ctrl Pts',(0.556372708444467,0.165586348396111,
-0.918978346266654));
#58721=CARTESIAN_POINT('Ctrl Pts',(0.167240263193989,0.555877795784612,
-0.895360957808875));
#58722=CARTESIAN_POINT('Ctrl Pts',(-0.372646143672664,0.445089070961746,
-0.871743569351098));
#58723=CARTESIAN_POINT('Ctrl Pts',(-0.576621321007168,-0.0669124924108635,
-0.848126180893318));
#58724=CARTESIAN_POINT('Ctrl Pts',(-0.260817667408242,-0.518597699425083,
-0.824508792435541));
#58725=CARTESIAN_POINT('Ctrl Pts',(0.290092627784849,-0.502807812972804,
-0.800891403977762));
#58726=CARTESIAN_POINT('Ctrl Pts',(0.579507203967856,-0.0337761754935562,
-0.777274015519984));
#58727=CARTESIAN_POINT('Ctrl Pts',(0.346541552393071,0.465702031288534,
-0.753656627062206));
#58728=CARTESIAN_POINT('Ctrl Pts',(-0.198804090018854,0.545386434807889,
-0.730039238604428));
#58729=CARTESIAN_POINT('Ctrl Pts',(-0.564943460083952,0.133447803998676,
-0.706421850146649));
#58730=CARTESIAN_POINT('Ctrl Pts',(-0.421830673606824,-0.398783540638234,
-0.682804461688872));
#58731=CARTESIAN_POINT('Ctrl Pts',(0.101529332987132,-0.571542845305737,
-0.659187073231093));
#58732=CARTESIAN_POINT('Ctrl Pts',(0.533368620403303,-0.229101166009451,
-0.635569684773314));
#58733=CARTESIAN_POINT('Ctrl Pts',(0.484417989205682,0.319857220017349,
-0.611952296315537));
#58734=CARTESIAN_POINT('Ctrl Pts',(-0.00119741120705677,0.58048944492177,
-0.588334907857758));
#58735=CARTESIAN_POINT('Ctrl Pts',(-0.485733439637777,0.317856029065321,
-0.564717519399981));
#58736=CARTESIAN_POINT('Ctrl Pts',(-0.532418923188744,-0.23129963154588,
-0.541100130942202));
#58737=CARTESIAN_POINT('Ctrl Pts',(-0.0991705662550569,-0.571956841189523,
-0.517482742484424));
#58738=CARTESIAN_POINT('Ctrl Pts',(0.423472268161632,-0.397039882567702,
-0.493865354026645));
#58739=CARTESIAN_POINT('Ctrl Pts',(0.564388111541162,0.135777346144949,
-0.470247965568867));
#58740=CARTESIAN_POINT('Ctrl Pts',(0.196552406003033,0.546201959982149,
-0.446630577111089));
#58741=CARTESIAN_POINT('Ctrl Pts',(-0.348459864303983,0.464268411014993,
-0.423013188653311));
#58742=CARTESIAN_POINT('Ctrl Pts',(-0.579362919518467,-0.0361666517081995,
-0.399395800195533));
#58743=CARTESIAN_POINT('Ctrl Pts',(-0.28801584026121,-0.504000305945962,
-0.375778411737754));
#58744=CARTESIAN_POINT('Ctrl Pts',(0.262954959069435,-0.517517294696554,
-0.352161023279976));
#58745=CARTESIAN_POINT('Ctrl Pts',(0.576892397212316,-0.0645330432685549,
-0.328543634822198));
#58746=CARTESIAN_POINT('Ctrl Pts',(0.370806879419165,0.446622588168993,
-0.30492624636442));
#58747=CARTESIAN_POINT('Ctrl Pts',(-0.169532355842391,0.55518320850602,
-0.281308857906642));
#58748=CARTESIAN_POINT('Ctrl Pts',(-0.557050641466449,0.163289440273063,
-0.257691469448863));
#58749=CARTESIAN_POINT('Ctrl Pts',(-0.442433154552453,-0.375796294124282,
-0.234074080991085));
#58750=CARTESIAN_POINT('Ctrl Pts',(0.0710062015071441,-0.576132414412867,
-0.210456692533307));
#58751=CARTESIAN_POINT('Ctrl Pts',(0.520433023585601,-0.257128051936333,
-0.186839304075529));
#58752=CARTESIAN_POINT('Ctrl Pts',(0.500741929240297,0.293652509918295,
-0.163221915617751));
#58753=CARTESIAN_POINT('Ctrl Pts',(0.0296490512789326,0.579737136376098,
-0.139604527159972));
#58754=CARTESIAN_POINT('Ctrl Pts',(-0.468127301314583,0.343217465772564,
-0.115987138702194));
#58755=CARTESIAN_POINT('Ctrl Pts',(-0.544006001714775,-0.202653478263663,
-0.0923697502444158));
#58756=CARTESIAN_POINT('Ctrl Pts',(-0.129347643736619,-0.565910377242601,
-0.0687523617866376));
#58757=CARTESIAN_POINT('Ctrl Pts',(0.401602625265567,-0.418923949859737,
-0.0451349733288594));
#58758=CARTESIAN_POINT('Ctrl Pts',(0.57112833318706,0.105459064899921,-0.0215175848710811));
#58759=CARTESIAN_POINT('Ctrl Pts',(0.224671807609435,0.53522691581883,0.00209980358669695));
#58760=CARTESIAN_POINT('Ctrl Pts',(-0.230784357175514,0.490560421931362,
0.0217809606348456));
#58761=CARTESIAN_POINT('Ctrl Pts',(-0.453312190429645,0.238513301675797,
0.0375258862733641));
#58762=CARTESIAN_POINT('Ctrl Pts',(-0.493223327388984,0.076687870891867,
0.0453983490926238));
#58763=CARTESIAN_POINT('Ctrl Pts',(-0.492479328147078,-0.00451235501740582,
0.0493345805022536));
#58764=CARTESIAN_POINT('Ctrl Pts',(-0.491975623968706,-0.000315807630563663,
-0.100884152590359));
#58765=CARTESIAN_POINT('Ctrl Pts',(-0.492335557319541,-0.0590109204422641,
-0.0980460184750444));
#58766=CARTESIAN_POINT('Ctrl Pts',(-0.48260563446014,-0.117592231258847,
-0.0952078843597301));
#58767=CARTESIAN_POINT('Ctrl Pts',(-0.462249825318384,-0.172217804087446,
-0.0923697502444159));
#58768=CARTESIAN_POINT('Ctrl Pts',(-0.40578654905539,-0.323739111256642,
-0.0844972874251564));
#58769=CARTESIAN_POINT('Ctrl Pts',(-0.267567096396004,-0.444824744249622,
-0.0766248246058969));
#58770=CARTESIAN_POINT('Ctrl Pts',(-0.109965658565945,-0.480869822848968,
-0.0687523617866375));
#58771=CARTESIAN_POINT('Ctrl Pts',(0.0476357792641106,-0.516914901448312,
-0.0608798989673781));
#58772=CARTESIAN_POINT('Ctrl Pts',(0.224619202264837,-0.467919425654025,
-0.0530074361481188));
#58773=CARTESIAN_POINT('Ctrl Pts',(0.341365198418784,-0.356024518630273,
-0.0451349733288595));
#58774=CARTESIAN_POINT('Ctrl Pts',(0.458111194572732,-0.244129611606518,
-0.0372625105096));
#58775=CARTESIAN_POINT('Ctrl Pts',(0.514619763879896,-0.0693352733532978,
-0.0293900476903405));
#58776=CARTESIAN_POINT('Ctrl Pts',(0.48513129427054,0.0896898709264652,
-0.021517584871081));
#58777=CARTESIAN_POINT('Ctrl Pts',(0.458264621493744,0.234576213664697,
-0.0143450565807208));
#58778=CARTESIAN_POINT('Ctrl Pts',(0.360012975466797,0.366372762798936,
-0.00717252829036059));
#58779=CARTESIAN_POINT('Ctrl Pts',(0.230193623813299,0.43607830012599,-3.19189119579733E-16));
#58780=CARTESIAN_POINT('Ctrl Pts',(-0.23680919645027,-0.331691137924157,
-1.6275));
#58781=CARTESIAN_POINT('Ctrl Pts',(-0.247292584852649,-0.325809951452391,
-1.6275));
#58782=CARTESIAN_POINT('Ctrl Pts',(-0.257473874870603,-0.319455449608397,
-1.6275));
#58783=CARTESIAN_POINT('Ctrl Pts',(-0.267315520773458,-0.312635691693424,
-1.6275));
#58784=CARTESIAN_POINT('Ctrl Pts',(-0.283255918048573,-0.301589810592047,
-1.6275));
#58785=CARTESIAN_POINT('Ctrl Pts',(-0.29830631137668,-0.289324966651072,
-1.6275));
#58786=CARTESIAN_POINT('Ctrl Pts',(-0.312429019847057,-0.275993569245607,
-1.6275));
#58787=CARTESIAN_POINT('Ctrl Pts',(-0.319028081099951,-0.269764260735142,
-1.6275));
#58788=CARTESIAN_POINT('Ctrl Pts',(-0.325427356265326,-0.263297962026011,
-1.6275));
#58789=CARTESIAN_POINT('Ctrl Pts',(-0.33160224299967,-0.256630917261684,
-1.6275));
#58790=CARTESIAN_POINT('Ctrl Pts',(-0.343131837484215,-0.244182377579899,
-1.6275));
#58791=CARTESIAN_POINT('Ctrl Pts',(-0.353893273503953,-0.231023434587135,
-1.6275));
#58792=CARTESIAN_POINT('Ctrl Pts',(-0.363862167909662,-0.217252793490027,
-1.6275));
#58793=CARTESIAN_POINT('Ctrl Pts',(-0.369628845525765,-0.209286930422141,
-1.6275));
#58794=CARTESIAN_POINT('Ctrl Pts',(-0.375130174240918,-0.201116096937704,
-1.6275));
#58795=CARTESIAN_POINT('Ctrl Pts',(-0.380360006918044,-0.192757432410251,
-1.6275));
#58796=CARTESIAN_POINT('Ctrl Pts',(-0.383706638921451,-0.187408623769459,
-1.6275));
#58797=CARTESIAN_POINT('Ctrl Pts',(-0.386943361934687,-0.181980584125983,
-1.6275));
#58798=CARTESIAN_POINT('Ctrl Pts',(-0.390064055273672,-0.176485097474883,
-1.6275));
#58799=CARTESIAN_POINT('Ctrl Pts',(-0.401809603024232,-0.155801392329387,
-1.6275));
#58800=CARTESIAN_POINT('Ctrl Pts',(-0.411879168607904,-0.134230471891167,
-1.6275));
#58801=CARTESIAN_POINT('Ctrl Pts',(-0.420209116630589,-0.11202262843158,
-1.6275));
#58802=CARTESIAN_POINT('Ctrl Pts',(-0.428561360146739,-0.0897553446456697,
-1.6275));
#58803=CARTESIAN_POINT('Ctrl Pts',(-0.435165490034037,-0.0668464241376505,
-1.6275));
#58804=CARTESIAN_POINT('Ctrl Pts',(-0.439917512881615,-0.0435147328928931,
-1.6275));
#58805=CARTESIAN_POINT('Ctrl Pts',(-0.441261264724132,-0.0369171208643323,
-1.6275));
#58806=CARTESIAN_POINT('Ctrl Pts',(-0.44245663271589,-0.0302855657760881,
-1.6275));
#58807=CARTESIAN_POINT('Ctrl Pts',(-0.443500544800912,-0.0236247585498435,
-1.6275));
#58808=CARTESIAN_POINT('Ctrl Pts',(-0.444360853499896,-0.0181354549186164,
-1.6275));
#58809=CARTESIAN_POINT('Ctrl Pts',(-0.445117804571293,-0.0126284577914863,
-1.6275));
#58810=CARTESIAN_POINT('Ctrl Pts',(-0.445768845006311,-0.00711771903575371,
-1.6275));
#58811=CARTESIAN_POINT('Ctrl Pts',(-0.448273775275097,0.0140852901325413,
-1.6275));
#58812=CARTESIAN_POINT('Ctrl Pts',(-0.44922037217288,0.035388346232463,
-1.6275));
#58813=CARTESIAN_POINT('Ctrl Pts',(-0.448549344096801,0.0566336200698592,
-1.6275));
#58814=CARTESIAN_POINT('Ctrl Pts',(-0.44794779188052,0.0756792338347052,
-1.6275));
#58815=CARTESIAN_POINT('Ctrl Pts',(-0.446046245694261,0.094679020300777,
-1.6275));
#58816=CARTESIAN_POINT('Ctrl Pts',(-0.442917696630645,0.113525745732605,
-1.6275));
#58817=CARTESIAN_POINT('Ctrl Pts',(-0.441365148422807,0.122878467776527,
-1.6275));
#58818=CARTESIAN_POINT('Ctrl Pts',(-0.439510089744425,0.132193541186416,
-1.6275));
#58819=CARTESIAN_POINT('Ctrl Pts',(-0.437359504525979,0.14145786706078,
-1.6275));
#58820=CARTESIAN_POINT('Ctrl Pts',(-0.435441498202038,0.149720285802278,
-1.6275));
#58821=CARTESIAN_POINT('Ctrl Pts',(-0.433286363153054,0.157948297464406,
-1.6275));
#58822=CARTESIAN_POINT('Ctrl Pts',(-0.430908919908843,0.16609904483546,
-1.6275));
#58823=CARTESIAN_POINT('Ctrl Pts',(-0.423966865940568,0.189898951844565,
-1.6275));
#58824=CARTESIAN_POINT('Ctrl Pts',(-0.415126170774039,0.213084008869322,
-1.6275));
#58825=CARTESIAN_POINT('Ctrl Pts',(-0.404550194275197,0.235430491055452,
-1.6275));
#58826=CARTESIAN_POINT('Ctrl Pts',(-0.39825831902693,0.248724892585953,
-1.6275));
#58827=CARTESIAN_POINT('Ctrl Pts',(-0.391351203164621,0.26172264764223,
-1.6275));
#58828=CARTESIAN_POINT('Ctrl Pts',(-0.383854614334943,0.274375771801172,
-1.6275));
#58829=CARTESIAN_POINT('Ctrl Pts',(-0.377157196255011,0.285680014895611,
-1.6275));
#58830=CARTESIAN_POINT('Ctrl Pts',(-0.369989182253541,0.296709222419132,
-1.6275));
#58831=CARTESIAN_POINT('Ctrl Pts',(-0.36236981407022,0.307441177344186,
-1.6275));
#58832=CARTESIAN_POINT('Ctrl Pts',(-0.35769318479098,0.314028255618716,
-1.6275));
#58833=CARTESIAN_POINT('Ctrl Pts',(-0.352843152564941,0.320507068160506,
-1.6275));
#58834=CARTESIAN_POINT('Ctrl Pts',(-0.347843186588654,0.326848425345271,
-1.6275));
#58835=CARTESIAN_POINT('Ctrl Pts',(-0.332035070403259,0.346897544004338,
-1.6275));
#58836=CARTESIAN_POINT('Ctrl Pts',(-0.314704075298522,0.365617528645167,
-1.6275));
#58837=CARTESIAN_POINT('Ctrl Pts',(-0.296024592620659,0.382867713127237,
-1.6275));
#58838=CARTESIAN_POINT('Ctrl Pts',(-0.277379319890049,0.400086305304992,
-1.6275));
#58839=CARTESIAN_POINT('Ctrl Pts',(-0.257389750250661,0.415841552587856,
-1.6275));
#58840=CARTESIAN_POINT('Ctrl Pts',(-0.236186328215152,0.429966383029456,
-1.6275));
#58841=CARTESIAN_POINT('Ctrl Pts',(-0.229845262913795,0.434190534774904,
-1.6275));
#58842=CARTESIAN_POINT('Ctrl Pts',(-0.22339538478044,0.438268623250253,
-1.6275));
#58843=CARTESIAN_POINT('Ctrl Pts',(-0.216839587231054,0.442195480991683,
-1.6275));
#58844=CARTESIAN_POINT('Origin',(-4.52129938221115E-17,0.,-1.6275));
#58845=CARTESIAN_POINT('',(-0.4925,-6.03138548580072E-17,-1.6275));
#58846=CARTESIAN_POINT('Origin',(0.,0.,-1.6275));
#58847=CARTESIAN_POINT('Origin',(0.,0.,-1.6275));
#58848=CARTESIAN_POINT('Origin',(0.42,0.,-1.7));
#58849=CARTESIAN_POINT('',(-0.42,-5.14351655641888E-17,-1.7));
#58850=CARTESIAN_POINT('Origin',(0.,0.,-1.7));
#58851=CARTESIAN_POINT('Origin',(0.,0.,-1.66));
#58852=CARTESIAN_POINT('',(-0.46,-5.63337527607782E-17,-1.66));
#58853=CARTESIAN_POINT('Origin',(0.,0.,-0.785));
#58854=CARTESIAN_POINT('',(0.,0.,0.));
#58855=CARTESIAN_POINT('Origin',(7.25,9.95,86.05));
#58856=CARTESIAN_POINT('',(0.575000000000009,9.975,86.075));
#58857=CARTESIAN_POINT('',(0.6,10.,86.1));
#58858=CARTESIAN_POINT('',(1.82500000000003,11.225,87.325));
#58859=CARTESIAN_POINT('',(9.4,10.,86.1));
#58860=CARTESIAN_POINT('',(7.25,10.,86.1));
#58861=CARTESIAN_POINT('',(9.425,9.975,86.075));
#58862=CARTESIAN_POINT('',(8.59166666666667,10.8083333333333,86.9083333333333));
#58863=CARTESIAN_POINT('',(9.35,9.9,86.));
#58864=CARTESIAN_POINT('',(5.72500000000001,6.27499999999958,82.3749999999998));
#58865=CARTESIAN_POINT('',(0.65,9.9,86.));
#58866=CARTESIAN_POINT('',(7.25,9.9,86.));
#58867=CARTESIAN_POINT('',(5.02499999999994,5.5249999999996,81.6249999999999));
#58868=CARTESIAN_POINT('Origin',(9.5,-10.,86.));
#58869=CARTESIAN_POINT('',(9.35,-9.9,86.));
#58870=CARTESIAN_POINT('',(9.35,-10.,86.));
#58871=CARTESIAN_POINT('',(0.65,-9.9,86.));
#58872=CARTESIAN_POINT('',(7.25,-9.9,86.));
#58873=CARTESIAN_POINT('',(0.65,-10.,86.));
#58874=CARTESIAN_POINT('Origin',(9.425,-10.,86.075));
#58875=CARTESIAN_POINT('',(9.5,9.9,86.15));
#58876=CARTESIAN_POINT('',(13.2499999999999,6.15000000000002,89.9000000000001));
#58877=CARTESIAN_POINT('',(9.5,-9.9,86.15));
#58878=CARTESIAN_POINT('',(9.5,-10.,86.15));
#58879=CARTESIAN_POINT('',(9.425,-9.975,86.075));
#58880=CARTESIAN_POINT('',(9.91666666666667,-9.48333333333333,86.5666666666667));
#58881=CARTESIAN_POINT('',(9.05833333333337,-9.60833333333333,85.7083333333334));
#58882=CARTESIAN_POINT('Origin',(9.45,9.95,89.));
#58883=CARTESIAN_POINT('',(9.4,10.,89.9));
#58884=CARTESIAN_POINT('',(9.4,10.,89.));
#58885=CARTESIAN_POINT('',(9.425,9.975,89.925));
#58886=CARTESIAN_POINT('',(8.67499999999999,10.725,89.175));
#58887=CARTESIAN_POINT('',(9.5,9.9,89.85));
#58888=CARTESIAN_POINT('',(12.9166666666666,6.48333333333333,86.4333333333333));
#58889=CARTESIAN_POINT('',(9.5,9.9,89.));
#58890=CARTESIAN_POINT('Origin',(5.,10.,88.));
#58891=CARTESIAN_POINT('',(0.6,10.,87.1585786437627));
#58892=CARTESIAN_POINT('',(0.6,10.,87.));
#58893=CARTESIAN_POINT('',(1.44142135623732,10.,88.));
#58894=CARTESIAN_POINT('',(2.29571067811867,10.,88.8542893218813));
#58895=CARTESIAN_POINT('',(0.600000000000003,10.,88.8414213562373));
#58896=CARTESIAN_POINT('',(1.87071067811866,10.,87.5707106781187));
#58897=CARTESIAN_POINT('',(0.6,10.,89.9));
#58898=CARTESIAN_POINT('',(0.6,10.,87.));
#58899=CARTESIAN_POINT('',(3.45857864376267,10.,89.9));
#58900=CARTESIAN_POINT('',(2.75,10.,89.9));
#58901=CARTESIAN_POINT('',(5.,10.,88.3585786437627));
#58902=CARTESIAN_POINT('',(4.30428932188134,10.,89.0542893218813));
#58903=CARTESIAN_POINT('',(6.54142135623733,10.,89.9));
#58904=CARTESIAN_POINT('',(4.94571067811866,10.,88.3042893218813));
#58905=CARTESIAN_POINT('',(5.75,10.,89.9));
#58906=CARTESIAN_POINT('Origin',(9.5,-10.,90.));
#58907=CARTESIAN_POINT('',(9.5,-9.9,89.85));
#58908=CARTESIAN_POINT('',(9.5,-10.,89.85));
#58909=CARTESIAN_POINT('',(9.5,-9.9,89.));
#58910=CARTESIAN_POINT('Origin',(4.91035533905933,9.95,88.3396446609407));
#58911=CARTESIAN_POINT('',(6.51464466094067,9.93535533905933,89.9646446609407));
#58912=CARTESIAN_POINT('',(6.58023082636872,10.0936943491397,89.8063056508603));
#58913=CARTESIAN_POINT('',(5.,9.9,88.5));
#58914=CARTESIAN_POINT('',(5.,9.81548220313558,88.6195262145876));
#58915=CARTESIAN_POINT('',(6.42928932188135,9.9,89.9292893218814));
#58916=CARTESIAN_POINT('',(4.875,9.9,88.375));
#58917=CARTESIAN_POINT('',(2.59518361520288,8.31186141672156,88.3411507386033));
#58918=CARTESIAN_POINT('Origin',(5.75,9.95,89.95));
#58919=CARTESIAN_POINT('',(6.60000000000001,9.9,90.));
#58920=CARTESIAN_POINT('',(6.60000000000001,9.9,90.));
#58921=CARTESIAN_POINT('',(9.35,9.9,90.));
#58922=CARTESIAN_POINT('',(5.75,9.9,90.));
#58923=CARTESIAN_POINT('',(5.47500000000001,6.0249999999996,93.8750000000001));
#58924=CARTESIAN_POINT('Origin',(6.51464466094068,-10.,89.9646446609407));
#58925=CARTESIAN_POINT('',(6.42928932188135,-9.9,89.9292893218814));
#58926=CARTESIAN_POINT('',(6.42928932188135,-10.,89.9292893218814));
#58927=CARTESIAN_POINT('',(6.60000000000001,-9.9,90.));
#58928=CARTESIAN_POINT('',(6.42928932188135,-9.9,89.9292893218814));
#58929=CARTESIAN_POINT('',(6.60000000000001,-10.,90.));
#58930=CARTESIAN_POINT('Origin',(3.48535533905933,-10.,89.9646446609407));
#58931=CARTESIAN_POINT('',(3.48535533905932,9.93535533905932,89.9646446609407));
#58932=CARTESIAN_POINT('',(3.4,9.9,90.));
#58933=CARTESIAN_POINT('',(0.142189545817937,8.55057072623677,91.3494292737631));
#58934=CARTESIAN_POINT('',(3.4,-9.9,90.));
#58935=CARTESIAN_POINT('',(3.4,-10.,90.));
#58936=CARTESIAN_POINT('',(3.48535533905932,-9.93535533905932,89.9646446609407));
#58937=CARTESIAN_POINT('',(3.22609583235893,-9.82796653520985,90.0720334647902));
#58938=CARTESIAN_POINT('',(3.57071067811866,-9.9,89.9292893218813));
#58939=CARTESIAN_POINT('',(3.92606829818375,-9.75280605427642,89.7820953761578));
#58940=CARTESIAN_POINT('',(3.57071067811866,9.9,89.9292893218813));
#58941=CARTESIAN_POINT('',(3.57071067811866,-10.,89.9292893218813));
#58942=CARTESIAN_POINT('',(7.00997458472428,8.47541024530379,88.504699567185));
#58943=CARTESIAN_POINT('Origin',(0.5,-10.,90.));
#58944=CARTESIAN_POINT('',(0.65,9.9,90.));
#58945=CARTESIAN_POINT('',(2.75,9.9,90.));
#58946=CARTESIAN_POINT('',(0.65,-9.9,90.));
#58947=CARTESIAN_POINT('',(0.65,-10.,90.));
#58948=CARTESIAN_POINT('',(2.75,-9.9,90.));
#58949=CARTESIAN_POINT('Origin',(2.75,9.95,89.95));
#58950=CARTESIAN_POINT('',(3.45857864376267,10.,89.9));
#58951=CARTESIAN_POINT('',(0.575000000000003,9.975,89.925));
#58952=CARTESIAN_POINT('',(1.40833333333333,10.8083333333333,89.0916666666667));
#58953=CARTESIAN_POINT('',(4.27500000000001,6.2749999999996,93.6250000000001));
#58954=CARTESIAN_POINT('Origin',(4.33964466094067,9.95,89.0896446609407));
#58955=CARTESIAN_POINT('',(4.375,9.9,89.125));
#58956=CARTESIAN_POINT('Origin',(3.5,-10.,90.));
#58957=CARTESIAN_POINT('',(5.,-9.9,88.5));
#58958=CARTESIAN_POINT('',(4.375,-9.9,89.125));
#58959=CARTESIAN_POINT('',(5.,-10.,88.5));
#58960=CARTESIAN_POINT('Origin',(0.575,-10.,89.925));
#58961=CARTESIAN_POINT('',(0.5,9.9,89.85));
#58962=CARTESIAN_POINT('',(-3.24999999999993,6.15000000000002,86.0999999999999));
#58963=CARTESIAN_POINT('',(0.5,-9.9,89.85));
#58964=CARTESIAN_POINT('',(0.5,-10.,89.85));
#58965=CARTESIAN_POINT('',(0.575000000000006,-9.975,89.925));
#58966=CARTESIAN_POINT('',(0.0833333333333344,-9.48333333333333,89.4333333333333));
#58967=CARTESIAN_POINT('',(0.941666666666637,-9.60833333333333,90.2916666666666));
#58968=CARTESIAN_POINT('Origin',(2.75,-9.95,89.95));
#58969=CARTESIAN_POINT('',(0.6,-10.,89.9));
#58970=CARTESIAN_POINT('',(1.40833333333333,-10.8083333333333,89.0916666666667));
#58971=CARTESIAN_POINT('',(3.45857864376267,-10.,89.9));
#58972=CARTESIAN_POINT('',(2.75,-10.,89.9));
#58973=CARTESIAN_POINT('',(3.45857864376267,-10.,89.9));
#58974=CARTESIAN_POINT('Origin',(4.33964466094067,-9.95,89.0896446609407));
#58975=CARTESIAN_POINT('',(5.,-10.,88.3585786437627));
#58976=CARTESIAN_POINT('',(4.30428932188134,-10.,89.0542893218813));
#58977=CARTESIAN_POINT('',(5.,-10.,88.3585786437627));
#58978=CARTESIAN_POINT('Origin',(6.54142135623733,-10.,89.9));
#58979=CARTESIAN_POINT('',(6.54142135623733,-10.,89.9));
#58980=CARTESIAN_POINT('',(6.54142135623733,-10.,89.9));
#58981=CARTESIAN_POINT('',(6.60000000000001,-9.9,90.));
#58982=CARTESIAN_POINT('Origin',(4.91035533905933,-9.95,88.3396446609407));
#58983=CARTESIAN_POINT('',(4.94571067811866,-10.,88.3042893218813));
#58984=CARTESIAN_POINT('',(4.875,-9.9,88.375));
#58985=CARTESIAN_POINT('Origin',(5.75,-9.95,89.95));
#58986=CARTESIAN_POINT('',(9.425,-9.975,89.925));
#58987=CARTESIAN_POINT('',(9.35,-9.9,90.));
#58988=CARTESIAN_POINT('',(8.80833333333339,-9.35833333333333,90.5416666666666));
#58989=CARTESIAN_POINT('',(5.75,-9.9,90.));
#58990=CARTESIAN_POINT('',(9.4,-10.,89.9));
#58991=CARTESIAN_POINT('',(5.75,-10.,89.9));
#58992=CARTESIAN_POINT('',(8.67499999999999,-10.725,89.175));
#58993=CARTESIAN_POINT('Origin',(0.55,-9.95,87.));
#58994=CARTESIAN_POINT('',(0.5,-9.9,88.9));
#58995=CARTESIAN_POINT('',(0.5,-9.9,87.));
#58996=CARTESIAN_POINT('',(0.6,-10.,88.8414213562373));
#58997=CARTESIAN_POINT('',(0.5,-9.9,88.9));
#58998=CARTESIAN_POINT('',(0.6,-10.,87.));
#58999=CARTESIAN_POINT('Origin',(5.,-10.,88.5));
#59000=CARTESIAN_POINT('Origin',(9.45,-9.95,89.));
#59001=CARTESIAN_POINT('',(9.4,-10.,86.1));
#59002=CARTESIAN_POINT('',(9.4,-10.,89.));
#59003=CARTESIAN_POINT('',(8.59166666666667,-10.8083333333333,86.9083333333333));
#59004=CARTESIAN_POINT('',(9.58333333333333,-9.81666666666667,89.7666666666667));
#59005=CARTESIAN_POINT('Origin',(7.25,-9.95,86.05));
#59006=CARTESIAN_POINT('',(0.6,-10.,86.1));
#59007=CARTESIAN_POINT('',(7.25,-10.,86.1));
#59008=CARTESIAN_POINT('',(0.575000000000001,-9.975,86.075));
#59009=CARTESIAN_POINT('',(1.82500000000003,-11.225,87.325));
#59010=CARTESIAN_POINT('',(1.69166666666657,-8.85833333333333,84.9583333333334));
#59011=CARTESIAN_POINT('Origin',(0.575,-10.,86.075));
#59012=CARTESIAN_POINT('',(0.5,-9.9,86.15));
#59013=CARTESIAN_POINT('',(0.416666666666669,-9.81666666666667,86.2333333333333));
#59014=CARTESIAN_POINT('',(0.5,9.9,86.15));
#59015=CARTESIAN_POINT('',(0.5,-10.,86.15));
#59016=CARTESIAN_POINT('',(-2.9166666666666,6.48333333333335,89.5666666666667));
#59017=CARTESIAN_POINT('Origin',(0.55,-9.95,87.));
#59018=CARTESIAN_POINT('',(0.599999999999999,-10.,87.1585786437627));
#59019=CARTESIAN_POINT('',(0.6,-10.,87.));
#59020=CARTESIAN_POINT('',(0.5,-9.9,87.1));
#59021=CARTESIAN_POINT('',(0.6,-10.,87.1585786437627));
#59022=CARTESIAN_POINT('',(0.5,-9.9,87.));
#59023=CARTESIAN_POINT('Origin',(0.6,10.,88.8414213562373));
#59024=CARTESIAN_POINT('',(0.5,9.9,88.9));
#59025=CARTESIAN_POINT('',(0.570710678118656,9.9,88.7292893218813));
#59026=CARTESIAN_POINT('',(0.5,9.9,88.9));
#59027=CARTESIAN_POINT('',(0.6,10.,88.8414213562373));
#59028=CARTESIAN_POINT('',(0.570710678118656,9.9,88.7292893218813));
#59029=CARTESIAN_POINT('Origin',(0.55,9.95,87.));
#59030=CARTESIAN_POINT('',(0.5,9.9,87.));
#59031=CARTESIAN_POINT('Origin',(0.570710678118656,-9.9,88.7292893218813));
#59032=CARTESIAN_POINT('',(0.570710678118656,-9.9,88.7292893218813));
#59033=CARTESIAN_POINT('',(0.570710678118656,-9.9,88.7292893218813));
#59034=CARTESIAN_POINT('',(0.600000000000003,-10.,88.8414213562373));
#59035=CARTESIAN_POINT('Origin',(0.535355339059328,-10.,88.8146446609407));
#59036=CARTESIAN_POINT('',(0.5,-10.,88.9));
#59037=CARTESIAN_POINT('',(0.570710678118656,-10.,88.7292893218813));
#59038=CARTESIAN_POINT('Origin',(0.599999999999999,10.,87.1585786437627));
#59039=CARTESIAN_POINT('',(0.570710678118658,9.9,87.2707106781187));
#59040=CARTESIAN_POINT('',(0.5,9.9,87.1));
#59041=CARTESIAN_POINT('',(0.570710678118656,9.9,87.2707106781187));
#59042=CARTESIAN_POINT('',(0.599999999999999,10.,87.1585786437627));
#59043=CARTESIAN_POINT('',(0.5,9.9,87.1));
#59044=CARTESIAN_POINT('Origin',(2.26035533905934,9.95,88.8896446609407));
#59045=CARTESIAN_POINT('',(1.3,9.9,88.));
#59046=CARTESIAN_POINT('',(2.22500000000001,9.9,88.925));
#59047=CARTESIAN_POINT('',(1.3,9.9,88.));
#59048=CARTESIAN_POINT('Origin',(0.55,9.95,87.));
#59049=CARTESIAN_POINT('',(0.5,9.9,87.));
#59050=CARTESIAN_POINT('Origin',(0.6,-10.,87.1585786437627));
#59051=CARTESIAN_POINT('',(0.570710678118656,-9.9,87.2707106781187));
#59052=CARTESIAN_POINT('',(0.5,-9.9,87.1));
#59053=CARTESIAN_POINT('',(0.570710678118658,-9.9,87.2707106781187));
#59054=CARTESIAN_POINT('Origin',(2.26035533905934,-9.95,88.8896446609407));
#59055=CARTESIAN_POINT('',(1.3,-9.9,88.));
#59056=CARTESIAN_POINT('',(2.22500000000001,-9.9,88.925));
#59057=CARTESIAN_POINT('',(1.44142135623732,-10.,88.));
#59058=CARTESIAN_POINT('',(2.29571067811867,-10.,88.8542893218813));
#59059=CARTESIAN_POINT('',(1.44142135623732,-10.,88.));
#59060=CARTESIAN_POINT('Origin',(0.535355339059328,-10.,87.1853553390593));
#59061=CARTESIAN_POINT('',(0.5,-10.,87.1));
#59062=CARTESIAN_POINT('',(0.570710678118656,-10.,87.2707106781187));
#59063=CARTESIAN_POINT('Origin',(1.83535533905933,-9.95,87.5353553390593));
#59064=CARTESIAN_POINT('',(1.87071067811866,-10.,87.5707106781187));
#59065=CARTESIAN_POINT('',(1.8,-9.9,87.5));
#59066=CARTESIAN_POINT('Origin',(1.83535533905933,9.95,87.5353553390593));
#59067=CARTESIAN_POINT('',(1.8,9.9,87.5));
#59068=CARTESIAN_POINT('Origin',(0.5,-10.,86.));
#59069=CARTESIAN_POINT('Origin',(5.,-10.,88.));
#59070=CARTESIAN_POINT('Origin',(1.3,-10.,88.));
#59071=CARTESIAN_POINT('',(1.3,-10.,88.));
#59072=CARTESIAN_POINT('Origin',(0.45,-10.,88.85));
#59073=CARTESIAN_POINT('Origin',(0.5,-10.,86.));
#59074=CARTESIAN_POINT('Origin',(9.425,-10.,89.925));
#59075=CARTESIAN_POINT('',(9.35,-10.,90.));
#59076=CARTESIAN_POINT('Origin',(6.5,-10.,90.));
#59077=CARTESIAN_POINT('',(0.,0.,0.));
#59078=CARTESIAN_POINT('Origin',(0.,0.,-5.925));
#59079=CARTESIAN_POINT('',(-0.792288171380763,0.000226347567109431,-11.8446668491763));
#59080=CARTESIAN_POINT('',(-0.791102747452279,4.01306674567125E-6,-11.8731331508237));
#59081=CARTESIAN_POINT('',(-0.7911,-9.68818082805471E-17,-5.925));
#59082=CARTESIAN_POINT('',(0.342278108299983,0.713534253311202,-11.9089));
#59083=CARTESIAN_POINT('Ctrl Pts',(-0.7911,-5.38458166943201E-15,-11.8446668491763));
#59084=CARTESIAN_POINT('Ctrl Pts',(-0.791100000000001,0.220167589666669,
-11.8535255927496));
#59085=CARTESIAN_POINT('Ctrl Pts',(-0.694214576672377,0.438610418338673,
-11.8623843363228));
#59086=CARTESIAN_POINT('Ctrl Pts',(-0.531017389080339,0.586395551223148,
-11.8712430798961));
#59087=CARTESIAN_POINT('Ctrl Pts',(-0.367820201488301,0.734180684107624,
-11.8801018234694));
#59088=CARTESIAN_POINT('Ctrl Pts',(-0.140868175871764,0.808992666571332,
-11.8889605670427));
#59089=CARTESIAN_POINT('Ctrl Pts',(0.0782205473247431,0.787223447298299,
-11.8978193106159));
#59090=CARTESIAN_POINT('Ctrl Pts',(0.169567364519674,0.778146992497718,
-11.901512873744));
#59091=CARTESIAN_POINT('Ctrl Pts',(0.259296389908129,0.753014751000273,
-11.905206436872));
#59092=CARTESIAN_POINT('Ctrl Pts',(0.342067962509849,0.713322310757459,
-11.9089));
#59093=CARTESIAN_POINT('',(-0.342067962509551,0.713322310757602,-11.9089));
#59094=CARTESIAN_POINT('Origin',(0.,0.,-11.9089));
#59095=CARTESIAN_POINT('Ctrl Pts',(-0.34206796250955,0.713322310757602,
-11.9089));
#59096=CARTESIAN_POINT('Ctrl Pts',(-0.46073916563555,0.656414492160488,
-11.9036044671685));
#59097=CARTESIAN_POINT('Ctrl Pts',(-0.564730701364708,0.569550653783437,
-11.8983089343371));
#59098=CARTESIAN_POINT('Ctrl Pts',(-0.641730011423605,0.462747660298155,
-11.8930134015056));
#59099=CARTESIAN_POINT('Ctrl Pts',(-0.718729321482501,0.355944666812873,
-11.8877178686741));
#59100=CARTESIAN_POINT('Ctrl Pts',(-0.768736405871138,0.229202518219359,
-11.8824223358427));
#59101=CARTESIAN_POINT('Ctrl Pts',(-0.785095797833949,0.0988017982372159,
-11.8771268030112));
#59102=CARTESIAN_POINT('Ctrl Pts',(-0.789208303196394,0.0660210163223179,
-11.8757955856154));
#59103=CARTESIAN_POINT('Ctrl Pts',(-0.791194462610664,0.0330090331603962,
-11.8744643682195));
#59104=CARTESIAN_POINT('Ctrl Pts',(-0.791102747452279,4.01306674567134E-6,
-11.8731331508237));
#59105=CARTESIAN_POINT('Origin',(0.,0.,-5.925));
#59106=CARTESIAN_POINT('',(-0.790012975131354,0.0005491902118549,-11.6446668491763));
#59107=CARTESIAN_POINT('',(-0.79040343262036,8.06582135657781E-6,-11.6731331508237));
#59108=CARTESIAN_POINT('',(-0.7911,-9.68818082805471E-17,-5.925));
#59109=CARTESIAN_POINT('Ctrl Pts',(-0.790012975131354,0.0005491902118549,
-11.6446668491763));
#59110=CARTESIAN_POINT('Ctrl Pts',(-0.790590861888083,0.105013430132942,
-11.6488501997533));
#59111=CARTESIAN_POINT('Ctrl Pts',(-0.771472741075023,0.209260755864815,
-11.6530335503304));
#59112=CARTESIAN_POINT('Ctrl Pts',(-0.731721227296555,0.304762699534902,
-11.6572169009074));
#59113=CARTESIAN_POINT('Ctrl Pts',(-0.63108158811855,0.546546728322295,
-11.6678079665704));
#59114=CARTESIAN_POINT('Ctrl Pts',(-0.398190192648554,0.732276372886272,
-11.6783990322333));
#59115=CARTESIAN_POINT('Ctrl Pts',(-0.140344232552206,0.779437657881449,
-11.6889900978962));
#59116=CARTESIAN_POINT('Ctrl Pts',(-0.0114212525040319,0.803018300379038,
-11.6942856307277));
#59117=CARTESIAN_POINT('Ctrl Pts',(0.12374036870073,0.791956852984427,-11.6995811635591));
#59118=CARTESIAN_POINT('Ctrl Pts',(0.249075376653612,0.750270516544755,
-11.7048766963906));
#59119=CARTESIAN_POINT('Ctrl Pts',(0.374410384606493,0.708584180105084,
-11.7101722292221));
#59120=CARTESIAN_POINT('Ctrl Pts',(0.489918779307494,0.636272954620351,
-11.7154677620535));
#59121=CARTESIAN_POINT('Ctrl Pts',(0.579225354855548,0.540248340915313,
-11.720763294885));
#59122=CARTESIAN_POINT('Ctrl Pts',(0.757838505951657,0.348199113505236,
-11.7313543605479));
#59123=CARTESIAN_POINT('Ctrl Pts',(0.831644380435981,0.0612963332139369,
-11.7419454262109));
#59124=CARTESIAN_POINT('Ctrl Pts',(0.768045306521618,-0.193562270365957,
-11.7525364918738));
#59125=CARTESIAN_POINT('Ctrl Pts',(0.736245769564436,-0.320991572155904,
-11.7578320247052));
#59126=CARTESIAN_POINT('Ctrl Pts',(0.670094995507583,-0.440409829767999,
-11.7631275575367));
#59127=CARTESIAN_POINT('Ctrl Pts',(0.580367540765873,-0.537139674991059,
-11.7684230903682));
#59128=CARTESIAN_POINT('Ctrl Pts',(0.490640086024162,-0.633869520214118,
-11.7737186231996));
#59129=CARTESIAN_POINT('Ctrl Pts',(0.377335950597594,-0.707910953048141,
-11.7790141560311));
#59130=CARTESIAN_POINT('Ctrl Pts',(0.253024067411846,-0.749801060819932,
-11.7843096888626));
#59131=CARTESIAN_POINT('Ctrl Pts',(0.128712184226097,-0.791691168591722,
-11.789605221694));
#59132=CARTESIAN_POINT('Ctrl Pts',(-0.00660744671883115,-0.801429951301279,
-11.7949007545255));
#59133=CARTESIAN_POINT('Ctrl Pts',(-0.136544532071595,-0.778895785431844,
-11.800196287357));
#59134=CARTESIAN_POINT('Ctrl Pts',(-0.266481617424357,-0.756361619562409,
-11.8054918201884));
#59135=CARTESIAN_POINT('Ctrl Pts',(-0.391036157184956,-0.701554505113982,
-11.8107873530199));
#59136=CARTESIAN_POINT('Ctrl Pts',(-0.49348933853164,-0.619414227979409,
-11.8160828858514));
#59137=CARTESIAN_POINT('Ctrl Pts',(-0.677828231414856,-0.471623329257867,
-11.8256108736263));
#59138=CARTESIAN_POINT('Ctrl Pts',(-0.790618379347089,-0.235346761505971,
-11.8351388614013));
#59139=CARTESIAN_POINT('Ctrl Pts',(-0.792288171380763,0.000226347567109431,
-11.8446668491763));
#59140=CARTESIAN_POINT('Ctrl Pts',(-0.791102747452279,4.01306674567134E-6,
-11.8731331508237));
#59141=CARTESIAN_POINT('Ctrl Pts',(-0.790829623153274,-0.0982836978797118,
-11.8691688353881));
#59142=CARTESIAN_POINT('Ctrl Pts',(-0.772129365994563,-0.19650965852332,
-11.8652045199524));
#59143=CARTESIAN_POINT('Ctrl Pts',(-0.736282073336785,-0.288384104892399,
-11.8612402045168));
#59144=CARTESIAN_POINT('Ctrl Pts',(-0.688397257339822,-0.411109996669098,
-11.8559446716854));
#59145=CARTESIAN_POINT('Ctrl Pts',(-0.60991592580891,-0.522502488851721,
-11.8506491388539));
#59146=CARTESIAN_POINT('Ctrl Pts',(-0.509058409110686,-0.606702005847251,
-11.8453536060224));
#59147=CARTESIAN_POINT('Ctrl Pts',(-0.307343375714237,-0.77510103983831,
-11.8347625403595));
#59148=CARTESIAN_POINT('Ctrl Pts',(-0.0161236016485408,-0.834728173080993,
-11.8241714746966));
#59149=CARTESIAN_POINT('Ctrl Pts',(0.233939335027844,-0.757220177092663,
-11.8135804090336));
#59150=CARTESIAN_POINT('Ctrl Pts',(0.484002271704228,-0.679712181104333,
-11.8029893433707));
#59151=CARTESIAN_POINT('Ctrl Pts',(0.692908370991301,-0.465069055884989,
-11.7923982777078));
#59152=CARTESIAN_POINT('Ctrl Pts',(0.763430372307437,-0.212979240313773,
-11.7818072120449));
#59153=CARTESIAN_POINT('Ctrl Pts',(0.833952373623573,0.0391105752574421,
-11.7712161463819));
#59154=CARTESIAN_POINT('Ctrl Pts',(0.766090276968773,0.328647081180532,
-11.760625080719));
#59155=CARTESIAN_POINT('Ctrl Pts',(0.592385804055834,0.525627978917452,
-11.7500340150561));
#59156=CARTESIAN_POINT('Ctrl Pts',(0.505533567599364,0.624118427785913,
-11.7447384822246));
#59157=CARTESIAN_POINT('Ctrl Pts',(0.39222073707836,0.699469974607832,-11.7394429493931));
#59158=CARTESIAN_POINT('Ctrl Pts',(0.268071565851031,0.743949386305491,
-11.7341474165617));
#59159=CARTESIAN_POINT('Ctrl Pts',(0.143922394623702,0.788428798003151,
-11.7288518837302));
#59160=CARTESIAN_POINT('Ctrl Pts',(0.0089368826900479,0.802036074576551,
-11.7235563508987));
#59161=CARTESIAN_POINT('Ctrl Pts',(-0.120716544232802,0.7820807665739,-11.7182608180673));
#59162=CARTESIAN_POINT('Ctrl Pts',(-0.250369971155652,0.762125458571248,
-11.7129652852358));
#59163=CARTESIAN_POINT('Ctrl Pts',(-0.374691313067697,0.708607565992544,
-11.7076697524044));
#59164=CARTESIAN_POINT('Ctrl Pts',(-0.479675261807679,0.628694803568363,
-11.7023742195729));
#59165=CARTESIAN_POINT('Ctrl Pts',(-0.58465921054766,0.548782041144181,
-11.6970786867414));
#59166=CARTESIAN_POINT('Ctrl Pts',(-0.670305766115577,0.442474408874522,
-11.69178315391));
#59167=CARTESIAN_POINT('Ctrl Pts',(-0.723483356181124,0.322384519957157,
-11.6864876210785));
#59168=CARTESIAN_POINT('Ctrl Pts',(-0.768185092994327,0.221435481053854,
-11.6820361309935));
#59169=CARTESIAN_POINT('Ctrl Pts',(-0.789943315386619,0.110747499155085,
-11.6775846409086));
#59170=CARTESIAN_POINT('Ctrl Pts',(-0.789527040486882,1.82139033282201E-5,
-11.6731331508237));
#59171=CARTESIAN_POINT('Origin',(0.,0.,-5.925));
#59172=CARTESIAN_POINT('',(-0.790545294603651,-0.000683398138164537,-11.4446668491763));
#59173=CARTESIAN_POINT('',(-0.7911,-5.52280443599784E-13,-11.4731331508237));
#59174=CARTESIAN_POINT('',(-0.7911,-9.68818082805471E-17,-5.925));
#59175=CARTESIAN_POINT('Ctrl Pts',(-0.790545294603651,-0.000683398138164537,
-11.4446668491763));
#59176=CARTESIAN_POINT('Ctrl Pts',(-0.788780870289845,0.180895070368877,
-11.4519704724424));
#59177=CARTESIAN_POINT('Ctrl Pts',(-0.726011118514491,0.36333336139957,
-11.4592740957086));
#59178=CARTESIAN_POINT('Ctrl Pts',(-0.611539636809332,0.503228087254033,
-11.4665777189747));
#59179=CARTESIAN_POINT('Ctrl Pts',(-0.528541449807152,0.604659539386308,
-11.4718732518062));
#59180=CARTESIAN_POINT('Ctrl Pts',(-0.418363373867963,0.68372560107528,
-11.4771687846376));
#59181=CARTESIAN_POINT('Ctrl Pts',(-0.295847636573397,0.733088687506037,
-11.4824643174691));
#59182=CARTESIAN_POINT('Ctrl Pts',(-0.173331899278832,0.782451773936795,
-11.4877598503006));
#59183=CARTESIAN_POINT('Ctrl Pts',(-0.0384785006288894,0.802111885109338,
-11.493055383132));
#59184=CARTESIAN_POINT('Ctrl Pts',(0.0917517255541586,0.786735608339574,
-11.4983509159635));
#59185=CARTESIAN_POINT('Ctrl Pts',(0.352212177920255,0.755983054800047,
-11.5089419816264));
#59186=CARTESIAN_POINT('Ctrl Pts',(0.594179940418773,0.585084949491291,
-11.5195330472894));
#59187=CARTESIAN_POINT('Ctrl Pts',(0.710697704171871,0.349664281229984,
-11.5301241129523));
#59188=CARTESIAN_POINT('Ctrl Pts',(0.76895658604842,0.231953947099331,-11.5354196457837));
#59189=CARTESIAN_POINT('Ctrl Pts',(0.795852968238614,0.0981129722305401,
-11.5407151786152));
#59190=CARTESIAN_POINT('Ctrl Pts',(0.790075348975073,-0.0336997945528526,
-11.5460107114467));
#59191=CARTESIAN_POINT('Ctrl Pts',(0.784297729711532,-0.165512561336244,
-11.5513062442781));
#59192=CARTESIAN_POINT('Ctrl Pts',(0.745846108994256,-0.295297120034238,
-11.5566017771096));
#59193=CARTESIAN_POINT('Ctrl Pts',(0.67822489890413,-0.407697544259937,
-11.5618973099411));
#59194=CARTESIAN_POINT('Ctrl Pts',(0.610603688814002,-0.520097968485637,
-11.5671928427725));
#59195=CARTESIAN_POINT('Ctrl Pts',(0.513812889351022,-0.615114258239043,
-11.572488375604));
#59196=CARTESIAN_POINT('Ctrl Pts',(0.400176763834465,-0.682055607413933,
-11.5777839084355));
#59197=CARTESIAN_POINT('Ctrl Pts',(0.286540638317908,-0.748996956588823,
-11.5830794412669));
#59198=CARTESIAN_POINT('Ctrl Pts',(0.156059186747776,-0.787863365185198,
-11.5883749740984));
#59199=CARTESIAN_POINT('Ctrl Pts',(0.0247893579774138,-0.791581102442525,
-11.5936705069299));
#59200=CARTESIAN_POINT('Ctrl Pts',(-0.237750299563309,-0.799016576957179,
-11.6042615725928));
#59201=CARTESIAN_POINT('Ctrl Pts',(-0.50344346590495,-0.665857366115643,
-11.6148526382557));
#59202=CARTESIAN_POINT('Ctrl Pts',(-0.652096107632763,-0.450358554189471,
-11.6254437039186));
#59203=CARTESIAN_POINT('Ctrl Pts',(-0.742032645208044,-0.319979323985716,
-11.6318514190045));
#59204=CARTESIAN_POINT('Ctrl Pts',(-0.789127815348344,-0.159460609050876,
-11.6382591340904));
#59205=CARTESIAN_POINT('Ctrl Pts',(-0.790012975131354,0.0005491902118549,
-11.6446668491763));
#59206=CARTESIAN_POINT('Ctrl Pts',(-0.7911,-5.48172618408671E-13,-11.6731331508237));
#59207=CARTESIAN_POINT('Ctrl Pts',(-0.791099999999848,-0.220167589667223,
-11.6642744072504));
#59208=CARTESIAN_POINT('Ctrl Pts',(-0.69421457667207,-0.43861041833916,
-11.6554156636771));
#59209=CARTESIAN_POINT('Ctrl Pts',(-0.531017389079927,-0.586395551223521,
-11.6465569201039));
#59210=CARTESIAN_POINT('Ctrl Pts',(-0.367820201487785,-0.734180684107883,
-11.6376981765306));
#59211=CARTESIAN_POINT('Ctrl Pts',(-0.140868175871194,-0.808992666571432,
-11.6288394329573));
#59212=CARTESIAN_POINT('Ctrl Pts',(0.0782205473252975,-0.787223447298244,
-11.619980689384));
#59213=CARTESIAN_POINT('Ctrl Pts',(0.297309270521789,-0.765454228025056,
-11.6111219458108));
#59214=CARTESIAN_POINT('Ctrl Pts',(0.505102072676036,-0.647444880833887,
-11.6022632022375));
#59215=CARTESIAN_POINT('Ctrl Pts',(0.636026795762051,-0.470435038100542,
-11.5934044586642));
#59216=CARTESIAN_POINT('Ctrl Pts',(0.766951518848066,-0.293425195367197,
-11.5845457150909));
#59217=CARTESIAN_POINT('Ctrl Pts',(0.818956872247111,-0.0601881960093751,
-11.5756869715177));
#59218=CARTESIAN_POINT('Ctrl Pts',(0.775631781004105,0.155674501111777,
-11.5668282279444));
#59219=CARTESIAN_POINT('Ctrl Pts',(0.732306689761099,0.37153719823293,-11.5579694843711));
#59220=CARTESIAN_POINT('Ctrl Pts',(0.594329958849832,0.566643518936898,
-11.5491107407979));
#59221=CARTESIAN_POINT('Ctrl Pts',(0.405242230243583,0.679424716085018,
-11.5402519972246));
#59222=CARTESIAN_POINT('Ctrl Pts',(0.216154501637335,0.792205913233137,
-11.5313932536513));
#59223=CARTESIAN_POINT('Ctrl Pts',(-0.021081652930565,0.820894963712988,
-11.522534510078));
#59224=CARTESIAN_POINT('Ctrl Pts',(-0.231602780753722,0.756438604215269,
-11.5136757665048));
#59225=CARTESIAN_POINT('Ctrl Pts',(-0.442123908576878,0.691982244717549,
-11.5048170229315));
#59226=CARTESIAN_POINT('Ctrl Pts',(-0.622631625634527,0.535390358803125,
-11.4959582793582));
#59227=CARTESIAN_POINT('Ctrl Pts',(-0.716163994722375,0.336077881841828,
-11.487099535785));
#59228=CARTESIAN_POINT('Ctrl Pts',(-0.765317280859639,0.231334857514026,
-11.4824440741312));
#59229=CARTESIAN_POINT('Ctrl Pts',(-0.791100000000078,0.115702837835999,
-11.4777886124774));
#59230=CARTESIAN_POINT('Ctrl Pts',(-0.7911,-5.29742916199893E-13,-11.4731331508237));
#59231=CARTESIAN_POINT('Origin',(0.,0.,-5.925));
#59232=CARTESIAN_POINT('',(-0.791998230343716,8.528260225521E-5,-11.2446668491763));
#59233=CARTESIAN_POINT('',(-0.7911,-5.52058398994859E-13,-11.2731331508237));
#59234=CARTESIAN_POINT('',(-0.7911,-9.68818082805471E-17,-5.925));
#59235=CARTESIAN_POINT('Ctrl Pts',(-0.791998230343716,8.528260225521E-5,
-11.2446668491763));
#59236=CARTESIAN_POINT('Ctrl Pts',(-0.792178295342062,0.127006680560579,
-11.2497952123001));
#59237=CARTESIAN_POINT('Ctrl Pts',(-0.759545080480787,0.253992239431632,
-11.2549235754238));
#59238=CARTESIAN_POINT('Ctrl Pts',(-0.700059092435406,0.367235780460078,
-11.2600519385476));
#59239=CARTESIAN_POINT('Ctrl Pts',(-0.638634034360461,0.484170731241736,
-11.265347471379));
#59240=CARTESIAN_POINT('Ctrl Pts',(-0.548577025685627,0.586453162772788,
-11.2706430042105));
#59241=CARTESIAN_POINT('Ctrl Pts',(-0.439362873703711,0.659038358226858,
-11.275938537042));
#59242=CARTESIAN_POINT('Ctrl Pts',(-0.22093456973988,0.804208749134998,
-11.2865296027049));
#59243=CARTESIAN_POINT('Ctrl Pts',(0.0741223074522833,0.830590195735207,
-11.2971206683678));
#59244=CARTESIAN_POINT('Ctrl Pts',(0.315331238093299,0.726582783969357,
-11.3077117340308));
#59245=CARTESIAN_POINT('Ctrl Pts',(0.435935703413807,0.674579078086432,
-11.3130072668622));
#59246=CARTESIAN_POINT('Ctrl Pts',(0.543078182096528,0.589978157611991,
-11.3183027996937));
#59247=CARTESIAN_POINT('Ctrl Pts',(0.624003832575897,0.48577151940361,-11.3235983325252));
#59248=CARTESIAN_POINT('Ctrl Pts',(0.704929483055266,0.381564881195229,
-11.3288938653566));
#59249=CARTESIAN_POINT('Ctrl Pts',(0.759638305331283,0.257752525252907,
-11.3341893981881));
#59250=CARTESIAN_POINT('Ctrl Pts',(0.78086075150283,0.128307203301138,-11.3394849310195));
#59251=CARTESIAN_POINT('Ctrl Pts',(0.802083197674377,-0.00113811865063054,
-11.344780463851));
#59252=CARTESIAN_POINT('Ctrl Pts',(0.789819267741456,-0.136216406611844,
-11.3500759966825));
#59253=CARTESIAN_POINT('Ctrl Pts',(0.746541473664785,-0.260801113101208,
-11.3553715295139));
#59254=CARTESIAN_POINT('Ctrl Pts',(0.703263679588115,-0.385385819590573,
-11.3606670623454));
#59255=CARTESIAN_POINT('Ctrl Pts',(0.628972021367694,-0.499476944608087,
-11.3659625951769));
#59256=CARTESIAN_POINT('Ctrl Pts',(0.531326032698895,-0.587288413821764,
-11.3712581280083));
#59257=CARTESIAN_POINT('Ctrl Pts',(0.336034055361296,-0.762911352249118,
-11.3818491936713));
#59258=CARTESIAN_POINT('Ctrl Pts',(0.0473247562301771,-0.833415667461127,
-11.3924402593342));
#59259=CARTESIAN_POINT('Ctrl Pts',(-0.205480744072948,-0.765395119469284,
-11.4030313249971));
#59260=CARTESIAN_POINT('Ctrl Pts',(-0.458286244376074,-0.697374571477442,
-11.41362239066));
#59261=CARTESIAN_POINT('Ctrl Pts',(-0.675187945851208,-0.490829160281748,
-11.424213456323));
#59262=CARTESIAN_POINT('Ctrl Pts',(-0.755000387460612,-0.241394221665018,
-11.4348045219859));
#59263=CARTESIAN_POINT('Ctrl Pts',(-0.779773985575188,-0.163970191019942,
-11.4380919643827));
#59264=CARTESIAN_POINT('Ctrl Pts',(-0.791339481691865,-0.0824138946279092,
-11.4413794067795));
#59265=CARTESIAN_POINT('Ctrl Pts',(-0.790545294603651,-0.000683398138164537,
-11.4446668491763));
#59266=CARTESIAN_POINT('Ctrl Pts',(-0.7911,-5.29742916199893E-13,-11.4731331508237));
#59267=CARTESIAN_POINT('Ctrl Pts',(-0.791099999999853,-0.220167589667203,
-11.4642744072504));
#59268=CARTESIAN_POINT('Ctrl Pts',(-0.694214576672081,-0.438610418339141,
-11.4554156636771));
#59269=CARTESIAN_POINT('Ctrl Pts',(-0.531017389079944,-0.586395551223506,
-11.4465569201039));
#59270=CARTESIAN_POINT('Ctrl Pts',(-0.367820201487807,-0.734180684107871,
-11.4376981765306));
#59271=CARTESIAN_POINT('Ctrl Pts',(-0.140868175871221,-0.808992666571427,
-11.4288394329573));
#59272=CARTESIAN_POINT('Ctrl Pts',(0.0782205473252707,-0.787223447298247,
-11.419980689384));
#59273=CARTESIAN_POINT('Ctrl Pts',(0.297309270521762,-0.765454228025067,
-11.4111219458108));
#59274=CARTESIAN_POINT('Ctrl Pts',(0.505102072676012,-0.647444880833905,
-11.4022632022375));
#59275=CARTESIAN_POINT('Ctrl Pts',(0.636026795762033,-0.470435038100567,
-11.3934044586642));
#59276=CARTESIAN_POINT('Ctrl Pts',(0.766951518848054,-0.293425195367228,
-11.3845457150909));
#59277=CARTESIAN_POINT('Ctrl Pts',(0.818956872247108,-0.0601881960094103,
-11.3756869715177));
#59278=CARTESIAN_POINT('Ctrl Pts',(0.775631781004112,0.155674501111743,
-11.3668282279444));
#59279=CARTESIAN_POINT('Ctrl Pts',(0.732306689761116,0.371537198232896,
-11.3579694843711));
#59280=CARTESIAN_POINT('Ctrl Pts',(0.594329958849859,0.566643518936869,
-11.3491107407979));
#59281=CARTESIAN_POINT('Ctrl Pts',(0.405242230243617,0.679424716084997,
-11.3402519972246));
#59282=CARTESIAN_POINT('Ctrl Pts',(0.216154501637376,0.792205913233126,
-11.3313932536513));
#59283=CARTESIAN_POINT('Ctrl Pts',(-0.021081652930521,0.820894963712989,
-11.322534510078));
#59284=CARTESIAN_POINT('Ctrl Pts',(-0.23160278075368,0.756438604215281,
-11.3136757665048));
#59285=CARTESIAN_POINT('Ctrl Pts',(-0.442123908576839,0.691982244717574,
-11.3048170229315));
#59286=CARTESIAN_POINT('Ctrl Pts',(-0.622631625634495,0.535390358803162,
-11.2959582793582));
#59287=CARTESIAN_POINT('Ctrl Pts',(-0.716163994722355,0.336077881841871,
-11.287099535785));
#59288=CARTESIAN_POINT('Ctrl Pts',(-0.765317280859636,0.23133485751405,
-11.2824440741312));
#59289=CARTESIAN_POINT('Ctrl Pts',(-0.791100000000082,0.115702837835997,
-11.2777886124774));
#59290=CARTESIAN_POINT('Ctrl Pts',(-0.7911,-5.57609514117985E-13,-11.2731331508237));
#59291=CARTESIAN_POINT('Origin',(0.,0.,-5.925));
#59292=CARTESIAN_POINT('',(-0.7911,2.07056594092592E-14,-11.0446668491763));
#59293=CARTESIAN_POINT('',(-0.791256742313348,0.000223351368557853,-11.0731331508237));
#59294=CARTESIAN_POINT('',(-0.7911,-9.68818082805471E-17,-5.925));
#59295=CARTESIAN_POINT('Ctrl Pts',(-0.791038879775141,0.000560250703841913,
-11.0446668491763));
#59296=CARTESIAN_POINT('Ctrl Pts',(-0.791423651940124,0.0741512003445719,
-11.0476199521577));
#59297=CARTESIAN_POINT('Ctrl Pts',(-0.78172570506452,0.14761201439333,-11.0505730551391));
#59298=CARTESIAN_POINT('Ctrl Pts',(-0.761508425370342,0.217890363424224,
-11.0535261581205));
#59299=CARTESIAN_POINT('Ctrl Pts',(-0.689000782353362,0.469937993987601,
-11.0641172237834));
#59300=CARTESIAN_POINT('Ctrl Pts',(-0.481189233708814,0.681051474651298,
-11.0747082894463));
#59301=CARTESIAN_POINT('Ctrl Pts',(-0.230012551894391,0.757925166261443,
-11.0852993551093));
#59302=CARTESIAN_POINT('Ctrl Pts',(-0.104424210987177,0.796362012066516,
-11.0905948879407));
#59303=CARTESIAN_POINT('Ctrl Pts',(0.0320054132125054,0.8012389106082,-11.0958904207722));
#59304=CARTESIAN_POINT('Ctrl Pts',(0.161144620509277,0.774200983873756,
-11.1011859536036));
#59305=CARTESIAN_POINT('Ctrl Pts',(0.290283827806048,0.747163057139313,
-11.1064814864351));
#59306=CARTESIAN_POINT('Ctrl Pts',(0.412132618199907,0.688210305128744,
-11.1117770192666));
#59307=CARTESIAN_POINT('Ctrl Pts',(0.512104914632304,0.603286671475527,
-11.117072552098));
#59308=CARTESIAN_POINT('Ctrl Pts',(0.612077211064701,0.51836303782231,-11.1223680849295));
#59309=CARTESIAN_POINT('Ctrl Pts',(0.690173013535636,0.407468522526445,
-11.127663617761));
#59310=CARTESIAN_POINT('Ctrl Pts',(0.737837287880873,0.284495218519558,
-11.1329591505924));
#59311=CARTESIAN_POINT('Ctrl Pts',(0.785501562226111,0.161521914512671,
-11.1382546834239));
#59312=CARTESIAN_POINT('Ctrl Pts',(0.802734308445651,0.0264698217947621,
-11.1435502162554));
#59313=CARTESIAN_POINT('Ctrl Pts',(0.785154399946323,-0.103670640969592,
-11.1488457490868));
#59314=CARTESIAN_POINT('Ctrl Pts',(0.749994582947666,-0.363951566498299,
-11.1594368147498));
#59315=CARTESIAN_POINT('Ctrl Pts',(0.575584147073533,-0.604585972212789,
-11.1700278804127));
#59316=CARTESIAN_POINT('Ctrl Pts',(0.338864849532643,-0.716395588408117,
-11.1806189460756));
#59317=CARTESIAN_POINT('Ctrl Pts',(0.102145551991752,-0.828205204603444,
-11.1912100117385));
#59318=CARTESIAN_POINT('Ctrl Pts',(-0.196882607215897,-0.811190031279611,
-11.2018010774015));
#59319=CARTESIAN_POINT('Ctrl Pts',(-0.419187228122118,-0.672739789110212,
-11.2123921430644));
#59320=CARTESIAN_POINT('Ctrl Pts',(-0.641491849028339,-0.534289546940814,
-11.2229832087273));
#59321=CARTESIAN_POINT('Ctrl Pts',(-0.787072931633131,-0.274404235925851,
-11.2335742743902));
#59322=CARTESIAN_POINT('Ctrl Pts',(-0.791875815867984,-0.0123258388778453,
-11.2441653400532));
#59323=CARTESIAN_POINT('Ctrl Pts',(-0.791951624741163,-0.00818918536021873,
-11.2443325097609));
#59324=CARTESIAN_POINT('Ctrl Pts',(-0.79199236074899,-0.00405198546671845,
-11.2444996794686));
#59325=CARTESIAN_POINT('Ctrl Pts',(-0.791998230343716,8.528260225521E-5,
-11.2446668491763));
#59326=CARTESIAN_POINT('Ctrl Pts',(-0.791333191223927,-2.41016881485458E-5,
-11.2731331508237));
#59327=CARTESIAN_POINT('Ctrl Pts',(-0.791326629821211,-0.128692147081735,
-11.2679385877924));
#59328=CARTESIAN_POINT('Ctrl Pts',(-0.75873374763038,-0.257269522733714,
-11.2627440247611));
#59329=CARTESIAN_POINT('Ctrl Pts',(-0.698053215585031,-0.371586410333449,
-11.2575494617299));
#59330=CARTESIAN_POINT('Ctrl Pts',(-0.636193200076023,-0.48812534302732,
-11.2522539288984));
#59331=CARTESIAN_POINT('Ctrl Pts',(-0.545143010043687,-0.589844020655748,
-11.2469583960669));
#59332=CARTESIAN_POINT('Ctrl Pts',(-0.435241086870445,-0.661756396250121,
-11.2416628632355));
#59333=CARTESIAN_POINT('Ctrl Pts',(-0.215437240523961,-0.805581147438867,
-11.2310717975725));
#59334=CARTESIAN_POINT('Ctrl Pts',(0.0797735383861531,-0.8301806904914,
-11.2204807319096));
#59335=CARTESIAN_POINT('Ctrl Pts',(0.31985801956751,-0.724611716522641,
-11.2098896662467));
#59336=CARTESIAN_POINT('Ctrl Pts',(0.439900260158188,-0.671827229538261,
-11.2045941334152));
#59337=CARTESIAN_POINT('Ctrl Pts',(0.546160926316679,-0.586500613298557,
-11.1992986005838));
#59338=CARTESIAN_POINT('Ctrl Pts',(0.626725961646807,-0.481829243974973,
-11.1940030677523));
#59339=CARTESIAN_POINT('Ctrl Pts',(0.707290996976935,-0.377157874651387,
-11.1887075349208));
#59340=CARTESIAN_POINT('Ctrl Pts',(0.762160401478703,-0.25314175224392,
-11.1834120020894));
#59341=CARTESIAN_POINT('Ctrl Pts',(0.782262440283046,-0.123631341427009,
-11.1781164692579));
#59342=CARTESIAN_POINT('Ctrl Pts',(0.822466517891732,0.135389480206813,
-11.167525403595));
#59343=CARTESIAN_POINT('Ctrl Pts',(0.723601132710717,0.416387455478408,
-11.156934337932));
#59344=CARTESIAN_POINT('Ctrl Pts',(0.528327196544448,0.590903654976208,
-11.1463432722691));
#59345=CARTESIAN_POINT('Ctrl Pts',(0.33305326037818,0.765419854474006,-11.1357522066062));
#59346=CARTESIAN_POINT('Ctrl Pts',(0.0413707732266558,0.833454278198008,
-11.1251611409433));
#59347=CARTESIAN_POINT('Ctrl Pts',(-0.211013810741115,0.763888209763645,
-11.1145700752803));
#59348=CARTESIAN_POINT('Ctrl Pts',(-0.463398394708886,0.694322141329282,
-11.1039790096174));
#59349=CARTESIAN_POINT('Ctrl Pts',(-0.676485075492905,0.487155580736554,
-11.0933879439545));
#59350=CARTESIAN_POINT('Ctrl Pts',(-0.755751859692147,0.236757597821015,
-11.0827968782915));
#59351=CARTESIAN_POINT('Ctrl Pts',(-0.779860626588515,0.160599763711617,
-11.0795756358022));
#59352=CARTESIAN_POINT('Ctrl Pts',(-0.791590318129958,0.0804427856162157,
-11.076354393313));
#59353=CARTESIAN_POINT('Ctrl Pts',(-0.791256742313348,0.000223351368557853,
-11.0731331508237));
#59354=CARTESIAN_POINT('Origin',(0.,0.,-5.925));
#59355=CARTESIAN_POINT('',(-0.7911,3.99680288865056E-15,-10.8446668491763));
#59356=CARTESIAN_POINT('',(-0.789614839096957,4.0911287493315E-5,-10.8731331508237));
#59357=CARTESIAN_POINT('',(-0.7911,-9.68818082805471E-17,-5.925));
#59358=CARTESIAN_POINT('Ctrl Pts',(-0.7911,-7.21644966006352E-15,-10.8446668491763));
#59359=CARTESIAN_POINT('Ctrl Pts',(-0.791100000000002,0.220167589666667,
-10.8535255927496));
#59360=CARTESIAN_POINT('Ctrl Pts',(-0.694214576672378,0.438610418338671,
-10.8623843363228));
#59361=CARTESIAN_POINT('Ctrl Pts',(-0.53101738908034,0.586395551223147,
-10.8712430798961));
#59362=CARTESIAN_POINT('Ctrl Pts',(-0.367820201488302,0.734180684107623,
-10.8801018234694));
#59363=CARTESIAN_POINT('Ctrl Pts',(-0.140868175871765,0.808992666571332,
-10.8889605670427));
#59364=CARTESIAN_POINT('Ctrl Pts',(0.0782205473247419,0.787223447298299,
-10.8978193106159));
#59365=CARTESIAN_POINT('Ctrl Pts',(0.297309270521249,0.765454228025266,
-10.9066780541892));
#59366=CARTESIAN_POINT('Ctrl Pts',(0.505102072675578,0.647444880834243,
-10.9155367977625));
#59367=CARTESIAN_POINT('Ctrl Pts',(0.636026795761718,0.470435038100992,
-10.9243955413357));
#59368=CARTESIAN_POINT('Ctrl Pts',(0.766951518847858,0.29342519536774,-10.933254284909));
#59369=CARTESIAN_POINT('Ctrl Pts',(0.818956872247068,0.0601881960099554,
-10.9421130284823));
#59370=CARTESIAN_POINT('Ctrl Pts',(0.775631781004215,-0.155674501111227,
-10.9509717720556));
#59371=CARTESIAN_POINT('Ctrl Pts',(0.732306689761362,-0.37153719823241,
-10.9598305156288));
#59372=CARTESIAN_POINT('Ctrl Pts',(0.594329958850234,-0.566643518936476,
-10.9686892592021));
#59373=CARTESIAN_POINT('Ctrl Pts',(0.405242230244066,-0.679424716084729,
-10.9775480027754));
#59374=CARTESIAN_POINT('Ctrl Pts',(0.216154501637899,-0.792205913232983,
-10.9864067463487));
#59375=CARTESIAN_POINT('Ctrl Pts',(-0.0210816529299804,-0.820894963713003,
-10.9952654899219));
#59376=CARTESIAN_POINT('Ctrl Pts',(-0.231602780753183,-0.756438604215434,
-11.0041242334952));
#59377=CARTESIAN_POINT('Ctrl Pts',(-0.442123908576385,-0.691982244717864,
-11.0129829770685));
#59378=CARTESIAN_POINT('Ctrl Pts',(-0.622631625634145,-0.53539035880357,
-11.0218417206417));
#59379=CARTESIAN_POINT('Ctrl Pts',(-0.716163994722135,-0.336077881842339,
-11.030700464215));
#59380=CARTESIAN_POINT('Ctrl Pts',(-0.765317280859481,-0.231334857514556,
-11.0353559258688));
#59381=CARTESIAN_POINT('Ctrl Pts',(-0.791100000000003,-0.115702837836527,
-11.0400113875225));
#59382=CARTESIAN_POINT('Ctrl Pts',(-0.7911,2.07056594092592E-14,-11.0446668491763));
#59383=CARTESIAN_POINT('Ctrl Pts',(-0.791256742313348,0.000223351368557853,
-11.0731331508237));
#59384=CARTESIAN_POINT('Ctrl Pts',(-0.791041939144359,-0.0514332371274546,
-11.0710588604815));
#59385=CARTESIAN_POINT('Ctrl Pts',(-0.785824980273388,-0.103115723698081,
-11.0689845701393));
#59386=CARTESIAN_POINT('Ctrl Pts',(-0.775690191700812,-0.153772947058482,
-11.0669102797971));
#59387=CARTESIAN_POINT('Ctrl Pts',(-0.749816713656429,-0.283097653441737,
-11.0616147469657));
#59388=CARTESIAN_POINT('Ctrl Pts',(-0.691891339614235,-0.405740219169775,
-11.0563192141342));
#59389=CARTESIAN_POINT('Ctrl Pts',(-0.607960482036218,-0.506547434948466,
-11.0510236813027));
#59390=CARTESIAN_POINT('Ctrl Pts',(-0.524029624458202,-0.607354650727156,
-11.0457281484713));
#59391=CARTESIAN_POINT('Ctrl Pts',(-0.414093283344361,-0.686326516556501,
-11.0404326156398));
#59392=CARTESIAN_POINT('Ctrl Pts',(-0.29150238721463,-0.735106189878946,
-11.0351370828084));
#59393=CARTESIAN_POINT('Ctrl Pts',(-0.1689114910849,-0.783885863201392,
-11.0298415499769));
#59394=CARTESIAN_POINT('Ctrl Pts',(-0.0336660399392779,-0.80247334401694,
-11.0245460171454));
#59395=CARTESIAN_POINT('Ctrl Pts',(0.0966528472069954,-0.786139020026476,
-11.019250484314));
#59396=CARTESIAN_POINT('Ctrl Pts',(0.357290621499545,-0.753470372045547,
-11.008659418651));
#59397=CARTESIAN_POINT('Ctrl Pts',(0.598222139794698,-0.581114504840562,
-10.9980683529881));
#59398=CARTESIAN_POINT('Ctrl Pts',(0.712871995411302,-0.345231531789129,
-10.9874772873252));
#59399=CARTESIAN_POINT('Ctrl Pts',(0.770196923219604,-0.227290045263412,
-10.9821817544937));
#59400=CARTESIAN_POINT('Ctrl Pts',(0.795951435358268,-0.0934667822760847,
-10.9768862216622));
#59401=CARTESIAN_POINT('Ctrl Pts',(0.789598100866673,0.0384667449812388,
-10.9715906888308));
#59402=CARTESIAN_POINT('Ctrl Pts',(0.783244766375078,0.170400272238561,
-10.9662951559993));
#59403=CARTESIAN_POINT('Ctrl Pts',(0.744783585253222,0.300444063765881,
-10.9609996231678));
#59404=CARTESIAN_POINT('Ctrl Pts',(0.6762662963784,0.412168813037878,-10.9557040903364));
#59405=CARTESIAN_POINT('Ctrl Pts',(0.539231718628754,0.635618311581874,
-10.9451130246735));
#59406=CARTESIAN_POINT('Ctrl Pts',(0.281972709867238,0.785791641104585,
-10.9345219590105));
#59407=CARTESIAN_POINT('Ctrl Pts',(0.0201632244658906,0.792395229952745,
-10.9239308933476));
#59408=CARTESIAN_POINT('Ctrl Pts',(-0.241646260935457,0.798998818800906,
-10.9133398276847));
#59409=CARTESIAN_POINT('Ctrl Pts',(-0.508006222976634,0.662032666974516,
-10.9027487620217));
#59410=CARTESIAN_POINT('Ctrl Pts',(-0.655337672110363,0.445628276542215,
-10.8921576963588));
#59411=CARTESIAN_POINT('Ctrl Pts',(-0.74355397164707,0.316053805920492,
-10.8858161811804));
#59412=CARTESIAN_POINT('Ctrl Pts',(-0.789096820830231,0.157999573193716,
-10.879474666002));
#59413=CARTESIAN_POINT('Ctrl Pts',(-0.789614839096957,4.0911287493315E-5,
-10.8731331508237));
#59414=CARTESIAN_POINT('Origin',(0.,0.,-5.925));
#59415=CARTESIAN_POINT('',(-0.7911,-1.38777878078145E-15,-10.6446668491763));
#59416=CARTESIAN_POINT('',(-0.792077588667444,-0.000904661696636211,-10.6731331508237));
#59417=CARTESIAN_POINT('',(-0.7911,-9.68818082805471E-17,-5.925));
#59418=CARTESIAN_POINT('Ctrl Pts',(-0.7911,9.82547376793264E-15,-10.6446668491763));
#59419=CARTESIAN_POINT('Ctrl Pts',(-0.791099999999997,0.220167589666684,
-10.6535255927496));
#59420=CARTESIAN_POINT('Ctrl Pts',(-0.694214576672368,0.438610418338686,
-10.6623843363228));
#59421=CARTESIAN_POINT('Ctrl Pts',(-0.531017389080327,0.586395551223159,
-10.6712430798961));
#59422=CARTESIAN_POINT('Ctrl Pts',(-0.367820201488286,0.734180684107631,
-10.6801018234694));
#59423=CARTESIAN_POINT('Ctrl Pts',(-0.140868175871747,0.808992666571335,
-10.6889605670427));
#59424=CARTESIAN_POINT('Ctrl Pts',(0.078220547324759,0.787223447298297,
-10.6978193106159));
#59425=CARTESIAN_POINT('Ctrl Pts',(0.297309270521265,0.76545422802526,-10.7066780541892));
#59426=CARTESIAN_POINT('Ctrl Pts',(0.505102072675592,0.647444880834232,
-10.7155367977625));
#59427=CARTESIAN_POINT('Ctrl Pts',(0.636026795761728,0.470435038100978,
-10.7243955413357));
#59428=CARTESIAN_POINT('Ctrl Pts',(0.766951518847865,0.293425195367723,
-10.733254284909));
#59429=CARTESIAN_POINT('Ctrl Pts',(0.818956872247069,0.0601881960099378,
-10.7421130284823));
#59430=CARTESIAN_POINT('Ctrl Pts',(0.775631781004212,-0.155674501111244,
-10.7509717720556));
#59431=CARTESIAN_POINT('Ctrl Pts',(0.732306689761354,-0.371537198232426,
-10.7598305156288));
#59432=CARTESIAN_POINT('Ctrl Pts',(0.594329958850222,-0.566643518936489,
-10.7686892592021));
#59433=CARTESIAN_POINT('Ctrl Pts',(0.405242230244052,-0.679424716084738,
-10.7775480027754));
#59434=CARTESIAN_POINT('Ctrl Pts',(0.216154501637882,-0.792205913232988,
-10.7864067463487));
#59435=CARTESIAN_POINT('Ctrl Pts',(-0.021081652929998,-0.820894963713003,
-10.7952654899219));
#59436=CARTESIAN_POINT('Ctrl Pts',(-0.231602780753199,-0.756438604215429,
-10.8041242334952));
#59437=CARTESIAN_POINT('Ctrl Pts',(-0.4421239085764,-0.691982244717854,
-10.8129829770685));
#59438=CARTESIAN_POINT('Ctrl Pts',(-0.622631625634156,-0.535390358803556,
-10.8218417206417));
#59439=CARTESIAN_POINT('Ctrl Pts',(-0.716163994722142,-0.336077881842324,
-10.830700464215));
#59440=CARTESIAN_POINT('Ctrl Pts',(-0.76531728085948,-0.231334857514553,
-10.8353559258688));
#59441=CARTESIAN_POINT('Ctrl Pts',(-0.791099999999999,-0.11570283783654,
-10.8400113875225));
#59442=CARTESIAN_POINT('Ctrl Pts',(-0.7911,-7.21644966006352E-15,-10.8446668491763));
#59443=CARTESIAN_POINT('Ctrl Pts',(-0.789614839096957,4.0911287493315E-5,
-10.8731331508237));
#59444=CARTESIAN_POINT('Ctrl Pts',(-0.789961971401216,-0.105809707903876,
-10.8688836003391));
#59445=CARTESIAN_POINT('Ctrl Pts',(-0.770090460703084,-0.211617410503161,
-10.8646340498546));
#59446=CARTESIAN_POINT('Ctrl Pts',(-0.729292731490852,-0.308783330747756,
-10.86038449937));
#59447=CARTESIAN_POINT('Ctrl Pts',(-0.678453068501093,-0.429865624657486,
-10.8550889665386));
#59448=CARTESIAN_POINT('Ctrl Pts',(-0.595117839959883,-0.537528408262529,
-10.8497934337071));
#59449=CARTESIAN_POINT('Ctrl Pts',(-0.491678650585443,-0.619349253092896,
-10.8444979008756));
#59450=CARTESIAN_POINT('Ctrl Pts',(-0.388239461211004,-0.701170097923264,
-10.8392023680442));
#59451=CARTESIAN_POINT('Ctrl Pts',(-0.26469631100334,-0.757149003978955,
-10.8339068352127));
#59452=CARTESIAN_POINT('Ctrl Pts',(-0.13546718676572,-0.779650494055077,
-10.8286113023812));
#59453=CARTESIAN_POINT('Ctrl Pts',(-0.00623806252809894,-0.8021519841312,
-10.8233157695498));
#59454=CARTESIAN_POINT('Ctrl Pts',(0.128677035739474,-0.79117605822775,
-10.8180202367183));
#59455=CARTESIAN_POINT('Ctrl Pts',(0.253692330652354,-0.748995963619501,
-10.8127247038868));
#59456=CARTESIAN_POINT('Ctrl Pts',(0.378707625565232,-0.706815869011252,
-10.8074291710554));
#59457=CARTESIAN_POINT('Ctrl Pts',(0.493823117123418,-0.633431605698205,
-10.8021336382239));
#59458=CARTESIAN_POINT('Ctrl Pts',(0.58257691189074,-0.536619486613459,
-10.7968381053924));
#59459=CARTESIAN_POINT('Ctrl Pts',(0.760084501425384,-0.342995248443968,
-10.7862470397295));
#59460=CARTESIAN_POINT('Ctrl Pts',(0.832145303796571,-0.0556595871876777,
-10.7756559740666));
#59461=CARTESIAN_POINT('Ctrl Pts',(0.766830956709737,0.198347110426995,
-10.7650649084037));
#59462=CARTESIAN_POINT('Ctrl Pts',(0.734173783166319,0.325350459234334,
-10.7597693755722));
#59463=CARTESIAN_POINT('Ctrl Pts',(0.667172822258395,0.444021567131268,
-10.7544738427407));
#59464=CARTESIAN_POINT('Ctrl Pts',(0.576922880519699,0.540467243498233,
-10.7491783099093));
#59465=CARTESIAN_POINT('Ctrl Pts',(0.486672938781004,0.636912919865197,
-10.7438827770778));
#59466=CARTESIAN_POINT('Ctrl Pts',(0.373174016211536,0.711133164702193,
-10.7385872442463));
#59467=CARTESIAN_POINT('Ctrl Pts',(0.248625480727413,0.751933909590113,
-10.7332917114149));
#59468=CARTESIAN_POINT('Ctrl Pts',(-0.000471590240832209,0.833535399365951,
-10.7227006457519));
#59469=CARTESIAN_POINT('Ctrl Pts',(-0.293767112867703,0.781458889345488,
-10.712109580089));
#59470=CARTESIAN_POINT('Ctrl Pts',(-0.497590747514042,0.617009079399273,
-10.7015185144261));
#59471=CARTESIAN_POINT('Ctrl Pts',(-0.679681582825412,0.470093814582901,
-10.6920567265586));
#59472=CARTESIAN_POINT('Ctrl Pts',(-0.790363295957457,0.233491399028885,
-10.6825949386912));
#59473=CARTESIAN_POINT('Ctrl Pts',(-0.792077588667444,-0.000904661696636211,
-10.6731331508237));
#59474=CARTESIAN_POINT('Origin',(0.,0.,-5.925));
#59475=CARTESIAN_POINT('',(-0.7911,-6.82787160144471E-15,-10.4446668491763));
#59476=CARTESIAN_POINT('',(-0.791602053176032,0.00100009030957082,-10.4731331508237));
#59477=CARTESIAN_POINT('',(-0.7911,-9.68818082805471E-17,-5.925));
#59478=CARTESIAN_POINT('Ctrl Pts',(-0.7911,-1.24344978758018E-14,-10.4446668491763));
#59479=CARTESIAN_POINT('Ctrl Pts',(-0.791100000000003,0.220167589666665,
-10.4535255927496));
#59480=CARTESIAN_POINT('Ctrl Pts',(-0.694214576672377,0.438610418338674,
-10.4623843363228));
#59481=CARTESIAN_POINT('Ctrl Pts',(-0.531017389080335,0.586395551223151,
-10.4712430798961));
#59482=CARTESIAN_POINT('Ctrl Pts',(-0.367820201488294,0.734180684107628,
-10.4801018234694));
#59483=CARTESIAN_POINT('Ctrl Pts',(-0.140868175871751,0.808992666571336,
-10.4889605670427));
#59484=CARTESIAN_POINT('Ctrl Pts',(0.0782205473247591,0.787223447298297,
-10.4978193106159));
#59485=CARTESIAN_POINT('Ctrl Pts',(0.297309270521269,0.765454228025259,
-10.5066780541892));
#59486=CARTESIAN_POINT('Ctrl Pts',(0.5051020726756,0.647444880834228,-10.5155367977625));
#59487=CARTESIAN_POINT('Ctrl Pts',(0.636026795761735,0.470435038100969,
-10.5243955413357));
#59488=CARTESIAN_POINT('Ctrl Pts',(0.766951518847871,0.293425195367709,
-10.533254284909));
#59489=CARTESIAN_POINT('Ctrl Pts',(0.818956872247071,0.060188196009918,
-10.5421130284823));
#59490=CARTESIAN_POINT('Ctrl Pts',(0.775631781004207,-0.155674501111266,
-10.5509717720556));
#59491=CARTESIAN_POINT('Ctrl Pts',(0.732306689761343,-0.37153719823245,
-10.5598305156288));
#59492=CARTESIAN_POINT('Ctrl Pts',(0.594329958850201,-0.566643518936512,
-10.5686892592021));
#59493=CARTESIAN_POINT('Ctrl Pts',(0.405242230244022,-0.679424716084756,
-10.5775480027754));
#59494=CARTESIAN_POINT('Ctrl Pts',(0.216154501637844,-0.792205913232999,
-10.5864067463487));
#59495=CARTESIAN_POINT('Ctrl Pts',(-0.0210816529300414,-0.820894963713003,
-10.5952654899219));
#59496=CARTESIAN_POINT('Ctrl Pts',(-0.231602780753242,-0.756438604215415,
-10.6041242334952));
#59497=CARTESIAN_POINT('Ctrl Pts',(-0.442123908576443,-0.691982244717828,
-10.6129829770685));
#59498=CARTESIAN_POINT('Ctrl Pts',(-0.622631625634193,-0.535390358803515,
-10.6218417206417));
#59499=CARTESIAN_POINT('Ctrl Pts',(-0.716163994722166,-0.336077881842273,
-10.630700464215));
#59500=CARTESIAN_POINT('Ctrl Pts',(-0.765317280859491,-0.23133485751451,
-10.6353559258688));
#59501=CARTESIAN_POINT('Ctrl Pts',(-0.791100000000001,-0.11570283783651,
-10.6400113875225));
#59502=CARTESIAN_POINT('Ctrl Pts',(-0.7911,9.82547376793264E-15,-10.6446668491763));
#59503=CARTESIAN_POINT('Ctrl Pts',(-0.792077588667444,-0.000904661696636211,
-10.6731331508237));
#59504=CARTESIAN_POINT('Ctrl Pts',(-0.792282191932643,-0.0288801638351418,
-10.6720038730282));
#59505=CARTESIAN_POINT('Ctrl Pts',(-0.790934580348652,-0.0568242369766668,
-10.6708745952328));
#59506=CARTESIAN_POINT('Ctrl Pts',(-0.787970899835483,-0.0845806499944255,
-10.6697453174373));
#59507=CARTESIAN_POINT('Ctrl Pts',(-0.760175670844775,-0.344897459569937,
-10.6591542517744));
#59508=CARTESIAN_POINT('Ctrl Pts',(-0.590233466197554,-0.588707968848993,
-10.6485631861114));
#59509=CARTESIAN_POINT('Ctrl Pts',(-0.35596858505029,-0.70746123569448,
-10.6379721204485));
#59510=CARTESIAN_POINT('Ctrl Pts',(-0.238836144476656,-0.766837869117224,
-10.632676587617));
#59511=CARTESIAN_POINT('Ctrl Pts',(-0.105623034778013,-0.794950191931574,
-10.6273810547856));
#59512=CARTESIAN_POINT('Ctrl Pts',(0.0261842875608677,-0.79035167857934,
-10.6220855219541));
#59513=CARTESIAN_POINT('Ctrl Pts',(0.157991609899747,-0.785753165227106,
-10.6167899891227));
#59514=CARTESIAN_POINT('Ctrl Pts',(0.288393144878865,-0.748443815708286,
-10.6114944562912));
#59515=CARTESIAN_POINT('Ctrl Pts',(0.401456790697708,-0.68193745810979,
-10.6061989234597));
#59516=CARTESIAN_POINT('Ctrl Pts',(0.514520436516553,-0.615431100511294,
-10.6009033906283));
#59517=CARTESIAN_POINT('Ctrl Pts',(0.610246193175124,-0.519727734833122,
-10.5956078577968));
#59518=CARTESIAN_POINT('Ctrl Pts',(0.67822631641647,-0.406649500024621,
-10.5903123249653));
#59519=CARTESIAN_POINT('Ctrl Pts',(0.746206439657815,-0.293571265216123,
-10.5850167921339));
#59520=CARTESIAN_POINT('Ctrl Pts',(0.786440929481935,-0.163118161277295,
-10.5797212593024));
#59521=CARTESIAN_POINT('Ctrl Pts',(0.791416696910816,-0.0318738691127503,
-10.5744257264709));
#59522=CARTESIAN_POINT('Ctrl Pts',(0.801368231768579,0.230614715216342,
-10.563834660808));
#59523=CARTESIAN_POINT('Ctrl Pts',(0.67028487704539,0.49626805244831,-10.5532435951451));
#59524=CARTESIAN_POINT('Ctrl Pts',(0.456071030378218,0.647588223821943,
-10.5426525294821));
#59525=CARTESIAN_POINT('Ctrl Pts',(0.348964107044634,0.723248309508759,
-10.5373569966507));
#59526=CARTESIAN_POINT('Ctrl Pts',(0.221074560725051,0.770325103730992,
-10.5320614638192));
#59527=CARTESIAN_POINT('Ctrl Pts',(0.0898525416784706,0.785411594080227,
-10.5267659309878));
#59528=CARTESIAN_POINT('Ctrl Pts',(-0.0413694773681122,0.800498084429462,
-10.5214703981563));
#59529=CARTESIAN_POINT('Ctrl Pts',(-0.175923969141694,0.783594270905701,
-10.5161748653248));
#59530=CARTESIAN_POINT('Ctrl Pts',(-0.297266180137799,0.734065427741078,
-10.5108793324933));
#59531=CARTESIAN_POINT('Ctrl Pts',(-0.539950602130008,0.635007741411831,
-10.5002882668304));
#59532=CARTESIAN_POINT('Ctrl Pts',(-0.7297859010123,0.405449936519141,-10.4896972011675));
#59533=CARTESIAN_POINT('Ctrl Pts',(-0.778681420574774,0.148162077888954,
-10.4791061355046));
#59534=CARTESIAN_POINT('Ctrl Pts',(-0.787873199085899,0.099795008036908,
-10.4771151406109));
#59535=CARTESIAN_POINT('Ctrl Pts',(-0.792084229722408,0.0504479706633907,
-10.4751241457173));
#59536=CARTESIAN_POINT('Ctrl Pts',(-0.791602053176032,0.00100009030957082,
-10.4731331508237));
#59537=CARTESIAN_POINT('Origin',(0.,0.,-5.925));
#59538=CARTESIAN_POINT('',(-0.7911,-1.2267964422108E-14,-10.2446668491763));
#59539=CARTESIAN_POINT('',(-0.789494028330408,-8.20471835821903E-5,-10.2731331508237));
#59540=CARTESIAN_POINT('',(-0.7911,-9.68818082805471E-17,-5.925));
#59541=CARTESIAN_POINT('Ctrl Pts',(-0.7911,4.55191440096314E-15,-10.2446668491763));
#59542=CARTESIAN_POINT('Ctrl Pts',(-0.791099999999999,0.220167589666681,
-10.2535255927496));
#59543=CARTESIAN_POINT('Ctrl Pts',(-0.694214576672369,0.438610418338685,
-10.2623843363228));
#59544=CARTESIAN_POINT('Ctrl Pts',(-0.531017389080327,0.586395551223159,
-10.2712430798961));
#59545=CARTESIAN_POINT('Ctrl Pts',(-0.367820201488285,0.734180684107633,
-10.2801018234694));
#59546=CARTESIAN_POINT('Ctrl Pts',(-0.140868175871743,0.808992666571336,
-10.2889605670427));
#59547=CARTESIAN_POINT('Ctrl Pts',(0.0782205473247649,0.787223447298297,
-10.2978193106159));
#59548=CARTESIAN_POINT('Ctrl Pts',(0.297309270521273,0.765454228025257,
-10.3066780541892));
#59549=CARTESIAN_POINT('Ctrl Pts',(0.505102072675601,0.647444880834227,
-10.3155367977625));
#59550=CARTESIAN_POINT('Ctrl Pts',(0.636026795761735,0.470435038100968,
-10.3243955413357));
#59551=CARTESIAN_POINT('Ctrl Pts',(0.76695151884787,0.29342519536771,-10.333254284909));
#59552=CARTESIAN_POINT('Ctrl Pts',(0.818956872247071,0.0601881960099218,
-10.3421130284823));
#59553=CARTESIAN_POINT('Ctrl Pts',(0.775631781004208,-0.155674501111261,
-10.3509717720556));
#59554=CARTESIAN_POINT('Ctrl Pts',(0.732306689761346,-0.371537198232443,
-10.3598305156288));
#59555=CARTESIAN_POINT('Ctrl Pts',(0.594329958850207,-0.566643518936505,
-10.3686892592021));
#59556=CARTESIAN_POINT('Ctrl Pts',(0.405242230244032,-0.67942471608475,
-10.3775480027754));
#59557=CARTESIAN_POINT('Ctrl Pts',(0.216154501637857,-0.792205913232995,
-10.3864067463487));
#59558=CARTESIAN_POINT('Ctrl Pts',(-0.0210816529300259,-0.820894963713002,
-10.3952654899219));
#59559=CARTESIAN_POINT('Ctrl Pts',(-0.231602780753226,-0.75643860421542,
-10.4041242334952));
#59560=CARTESIAN_POINT('Ctrl Pts',(-0.442123908576426,-0.691982244717838,
-10.4129829770685));
#59561=CARTESIAN_POINT('Ctrl Pts',(-0.622631625634179,-0.535390358803531,
-10.4218417206417));
#59562=CARTESIAN_POINT('Ctrl Pts',(-0.716163994722157,-0.336077881842293,
-10.430700464215));
#59563=CARTESIAN_POINT('Ctrl Pts',(-0.765317280859485,-0.231334857514532,
-10.4353559258688));
#59564=CARTESIAN_POINT('Ctrl Pts',(-0.791099999999998,-0.115702837836532,
-10.4400113875225));
#59565=CARTESIAN_POINT('Ctrl Pts',(-0.7911,-1.24344978758018E-14,-10.4446668491763));
#59566=CARTESIAN_POINT('Ctrl Pts',(-0.791602053176032,0.00100009030957082,
-10.4731331508237));
#59567=CARTESIAN_POINT('Ctrl Pts',(-0.789519299254671,-0.212589242236902,
-10.4645330800544));
#59568=CARTESIAN_POINT('Ctrl Pts',(-0.699870954088247,-0.428060097343416,
-10.4559330092851));
#59569=CARTESIAN_POINT('Ctrl Pts',(-0.545830694696212,-0.574561465875036,
-10.4473329385158));
#59570=CARTESIAN_POINT('Ctrl Pts',(-0.356128709012524,-0.754979238641152,
-10.4367418728528));
#59571=CARTESIAN_POINT('Ctrl Pts',(-0.0687689974024994,-0.830796871805704,
-10.4261508071899));
#59572=CARTESIAN_POINT('Ctrl Pts',(0.186660758624119,-0.769657582787913,
-10.415559741527));
#59573=CARTESIAN_POINT('Ctrl Pts',(0.314375636637429,-0.739087938279018,
-10.4102642086955));
#59574=CARTESIAN_POINT('Ctrl Pts',(0.434108025754885,-0.674279063224538,
-10.4049686758641));
#59575=CARTESIAN_POINT('Ctrl Pts',(0.531593497608413,-0.585448329102326,
-10.3996731430326));
#59576=CARTESIAN_POINT('Ctrl Pts',(0.629078969461942,-0.496617594980113,
-10.3943776102011));
#59577=CARTESIAN_POINT('Ctrl Pts',(0.70431752405154,-0.38376500179017,-10.3890820773697));
#59578=CARTESIAN_POINT('Ctrl Pts',(0.747440544825585,-0.25988244173352,
-10.3837865445382));
#59579=CARTESIAN_POINT('Ctrl Pts',(0.790563565599631,-0.135999881676871,
-10.3784910117067));
#59580=CARTESIAN_POINT('Ctrl Pts',(0.801571052558123,-0.00108735475351671,
-10.3731954788753));
#59581=CARTESIAN_POINT('Ctrl Pts',(0.780183408902627,0.129106934837772,
-10.3678999460438));
#59582=CARTESIAN_POINT('Ctrl Pts',(0.758795765247131,0.25930122442906,-10.3626044132124));
#59583=CARTESIAN_POINT('Ctrl Pts',(0.705012990977646,0.384777276688281,
-10.3573088803809));
#59584=CARTESIAN_POINT('Ctrl Pts',(0.623844164687467,0.488031545975095,
-10.3520133475494));
#59585=CARTESIAN_POINT('Ctrl Pts',(0.46150651210711,0.694540084548719,-10.3414222818865));
#59586=CARTESIAN_POINT('Ctrl Pts',(0.189624651443974,0.812161491232711,
-10.3308312162236));
#59587=CARTESIAN_POINT('Ctrl Pts',(-0.0716046547973555,0.788824483516112,
-10.3202401505606));
#59588=CARTESIAN_POINT('Ctrl Pts',(-0.202219307918021,0.777155979657812,
-10.3149446177292));
#59589=CARTESIAN_POINT('Ctrl Pts',(-0.330170822433236,0.730247872199365,
-10.3096490848977));
#59590=CARTESIAN_POINT('Ctrl Pts',(-0.439953316334173,0.656799764622589,
-10.3043535520662));
#59591=CARTESIAN_POINT('Ctrl Pts',(-0.549735810235111,0.583351657045813,
-10.2990580192348));
#59592=CARTESIAN_POINT('Ctrl Pts',(-0.641349283521772,0.483363549350709,
-10.2937624864033));
#59593=CARTESIAN_POINT('Ctrl Pts',(-0.701772585750591,0.367061945654053,
-10.2884669535718));
#59594=CARTESIAN_POINT('Ctrl Pts',(-0.760093377208675,0.254807214031685,
-10.2833556859891));
#59595=CARTESIAN_POINT('Ctrl Pts',(-0.789356841601489,0.127354534696367,
-10.2782444184064));
#59596=CARTESIAN_POINT('Ctrl Pts',(-0.789494028330408,-8.20471835821903E-5,
-10.2731331508237));
#59597=CARTESIAN_POINT('Origin',(0.,0.,-5.925));
#59598=CARTESIAN_POINT('',(-0.790401422788456,-0.000312835344477125,-10.0446668491763));
#59599=CARTESIAN_POINT('',(-0.791423880525058,-0.000561432253963593,-10.0731331508237));
#59600=CARTESIAN_POINT('',(-0.7911,-9.68818082805471E-17,-5.925));
#59601=CARTESIAN_POINT('Ctrl Pts',(-0.790401422788456,-0.000312835344477125,
-10.0446668491763));
#59602=CARTESIAN_POINT('Ctrl Pts',(-0.788697176084344,0.197685440689488,
-10.0526302499402));
#59603=CARTESIAN_POINT('Ctrl Pts',(-0.714105001319401,0.396267685858613,
-10.0605936507041));
#59604=CARTESIAN_POINT('Ctrl Pts',(-0.579842908951946,0.540216832650709,
-10.0685570514681));
#59605=CARTESIAN_POINT('Ctrl Pts',(-0.401278665048899,0.731664545882161,
-10.079148117131));
#59606=CARTESIAN_POINT('Ctrl Pts',(-0.117169433251898,0.826476467771916,
-10.0897391827939));
#59607=CARTESIAN_POINT('Ctrl Pts',(0.140581802644246,0.780085580457693,
-10.1003302484568));
#59608=CARTESIAN_POINT('Ctrl Pts',(0.398333038540391,0.733694693143469,
-10.1109213141198));
#59609=CARTESIAN_POINT('Ctrl Pts',(0.629726278535683,0.546100996625268,
-10.1215123797827));
#59610=CARTESIAN_POINT('Ctrl Pts',(0.731139569969053,0.304391463881425,
-10.1321034454456));
#59611=CARTESIAN_POINT('Ctrl Pts',(0.781846215685738,0.183536697509504,
-10.1373989782771));
#59612=CARTESIAN_POINT('Ctrl Pts',(0.800057874261942,0.0491529720811725,
-10.1426945111086));
#59613=CARTESIAN_POINT('Ctrl Pts',(0.786248331162366,-0.082209568215139,
-10.14799004394));
#59614=CARTESIAN_POINT('Ctrl Pts',(0.77243878806279,-0.21357210851145,-10.1532855767715));
#59615=CARTESIAN_POINT('Ctrl Pts',(0.726608043287434,-0.341913463675741,
-10.1585811096029));
#59616=CARTESIAN_POINT('Ctrl Pts',(0.65199323215211,-0.449751172995639,
-10.1638766424344));
#59617=CARTESIAN_POINT('Ctrl Pts',(0.502763609881462,-0.665426591635433,
-10.1744677080973));
#59618=CARTESIAN_POINT('Ctrl Pts',(0.238397722170937,-0.799087426897659,
-10.1850587737603));
#59619=CARTESIAN_POINT('Ctrl Pts',(-0.0241752336446996,-0.791689263385369,
-10.1956498394232));
#59620=CARTESIAN_POINT('Ctrl Pts',(-0.155461711552519,-0.787990181629224,
-10.2009453722547));
#59621=CARTESIAN_POINT('Ctrl Pts',(-0.286299956486616,-0.749026350179451,
-10.2062409050861));
#59622=CARTESIAN_POINT('Ctrl Pts',(-0.400034001397628,-0.682149213791184,
-10.2115364379176));
#59623=CARTESIAN_POINT('Ctrl Pts',(-0.513768046308639,-0.615272077402917,
-10.2168319707491));
#59624=CARTESIAN_POINT('Ctrl Pts',(-0.610397891196563,-0.520481636076158,
-10.2221275035805));
#59625=CARTESIAN_POINT('Ctrl Pts',(-0.678000733044698,-0.408070162547321,
-10.227423036412));
#59626=CARTESIAN_POINT('Ctrl Pts',(-0.745603574892832,-0.295658689018485,
-10.2327185692435));
#59627=CARTESIAN_POINT('Ctrl Pts',(-0.784179413701176,-0.165626183287574,
-10.2380141020749));
#59628=CARTESIAN_POINT('Ctrl Pts',(-0.79005963579369,-0.0338698189808012,
-10.2433096349064));
#59629=CARTESIAN_POINT('Ctrl Pts',(-0.790561991369495,-0.0226136889884339,
-10.243762039663));
#59630=CARTESIAN_POINT('Ctrl Pts',(-0.790825717226918,-0.0113449773741918,
-10.2442144444197));
#59631=CARTESIAN_POINT('Ctrl Pts',(-0.790851609223311,-7.45956026386718E-5,
-10.2446668491763));
#59632=CARTESIAN_POINT('Ctrl Pts',(-0.789494028330408,-8.20471835821903E-5,
-10.2731331508237));
#59633=CARTESIAN_POINT('Ctrl Pts',(-0.789641106440014,-0.136707008689031,
-10.2676533527435));
#59634=CARTESIAN_POINT('Ctrl Pts',(-0.756310388284488,-0.273313467750145,
-10.2621735546633));
#59635=CARTESIAN_POINT('Ctrl Pts',(-0.689416907730222,-0.391153529203585,
-10.2566937565831));
#59636=CARTESIAN_POINT('Ctrl Pts',(-0.560128705025943,-0.618908605268401,
-10.2461026909201));
#59637=CARTESIAN_POINT('Ctrl Pts',(-0.305466379391119,-0.776561565998511,
-10.2355116252572));
#59638=CARTESIAN_POINT('Ctrl Pts',(-0.0440833857200287,-0.791270295439225,
-10.2249205595943));
#59639=CARTESIAN_POINT('Ctrl Pts',(0.217299607951058,-0.805979024879939,
-10.2143294939313));
#59640=CARTESIAN_POINT('Ctrl Pts',(0.485403269658407,-0.677743523031253,
-10.2037384282684));
#59641=CARTESIAN_POINT('Ctrl Pts',(0.640510817041626,-0.465790646971077,
-10.1931473626055));
#59642=CARTESIAN_POINT('Ctrl Pts',(0.718064590733235,-0.359814208940989,
-10.187851829774));
#59643=CARTESIAN_POINT('Ctrl Pts',(0.767369335843814,-0.232908427358027,
-10.1825562969426));
#59644=CARTESIAN_POINT('Ctrl Pts',(0.784167076252959,-0.102095001195637,
-10.1772607641111));
#59645=CARTESIAN_POINT('Ctrl Pts',(0.800964816662105,0.0287184249667539,
-10.1719652312796));
#59646=CARTESIAN_POINT('Ctrl Pts',(0.785255552369819,0.163439495708571,
-10.1666696984482));
#59647=CARTESIAN_POINT('Ctrl Pts',(0.737927847365211,0.285777437271543,
-10.1613741656167));
#59648=CARTESIAN_POINT('Ctrl Pts',(0.690600142360604,0.408115378834514,
-10.1560786327852));
#59649=CARTESIAN_POINT('Ctrl Pts',(0.611653996643675,0.518070191218638,
-10.1507830999538));
#59650=CARTESIAN_POINT('Ctrl Pts',(0.511070942247287,0.603457740144741,
-10.1454875671223));
#59651=CARTESIAN_POINT('Ctrl Pts',(0.410487887850897,0.688845289070846,
-10.1401920342908));
#59652=CARTESIAN_POINT('Ctrl Pts',(0.288267924775049,0.749665574538929,
-10.1348965014594));
#59653=CARTESIAN_POINT('Ctrl Pts',(0.159559889402088,0.775820193972442,
-10.1296009686279));
#59654=CARTESIAN_POINT('Ctrl Pts',(-0.0978561813438297,0.828129432839467,
-10.119009902965));
#59655=CARTESIAN_POINT('Ctrl Pts',(-0.381224541278192,0.741776007568202,
-10.108418837302));
#59656=CARTESIAN_POINT('Ctrl Pts',(-0.565223850966701,0.554881330269348,
-10.0978277716391));
#59657=CARTESIAN_POINT('Ctrl Pts',(-0.657223505810957,0.461433991619919,
-10.0925322388077));
#59658=CARTESIAN_POINT('Ctrl Pts',(-0.724380898093749,0.342851339963596,
-10.0872367059762));
#59659=CARTESIAN_POINT('Ctrl Pts',(-0.760509296341098,0.215801903468189,
-10.0819411731447));
#59660=CARTESIAN_POINT('Ctrl Pts',(-0.780539999471085,0.145361760291943,
-10.0790051657044));
#59661=CARTESIAN_POINT('Ctrl Pts',(-0.791032585068395,0.072318980729004,
-10.076069158264));
#59662=CARTESIAN_POINT('Ctrl Pts',(-0.791423880525058,-0.000561432253963593,
-10.0731331508237));
#59663=CARTESIAN_POINT('Origin',(0.,0.,-5.925));
#59664=CARTESIAN_POINT('',(-0.792437169753526,-0.000127296230932911,-9.8446668491763));
#59665=CARTESIAN_POINT('',(-0.791999899124744,0.000522216889476513,-9.87313315082368));
#59666=CARTESIAN_POINT('',(-0.7911,-9.68818082805471E-17,-5.925));
#59667=CARTESIAN_POINT('Ctrl Pts',(-0.792437169753526,-0.000127296230932911,
-9.8446668491763));
#59668=CARTESIAN_POINT('Ctrl Pts',(-0.792483963508099,0.0120472072685257,
-9.84515945696638));
#59669=CARTESIAN_POINT('Ctrl Pts',(-0.792227470903532,0.0242221673588838,
-9.84565206475646));
#59670=CARTESIAN_POINT('Ctrl Pts',(-0.791661615652341,0.0363855966523024,
-9.84614467254654));
#59671=CARTESIAN_POINT('Ctrl Pts',(-0.779495729846714,0.297899281427651,
-9.85673573820947));
#59672=CARTESIAN_POINT('Ctrl Pts',(-0.624327009889845,0.554082857153437,
-9.86732680387239));
#59673=CARTESIAN_POINT('Ctrl Pts',(-0.397840131682881,0.685580035951506,
-9.87791786953532));
#59674=CARTESIAN_POINT('Ctrl Pts',(-0.171353253475907,0.817077214749582,
-9.88850893519825));
#59675=CARTESIAN_POINT('Ctrl Pts',(0.126451782981168,0.823887996619928,
-9.89910000086118));
#59676=CARTESIAN_POINT('Ctrl Pts',(0.360219314034763,0.705309350465974,
-9.90969106652411));
#59677=CARTESIAN_POINT('Ctrl Pts',(0.477103079561559,0.646020027388998,
-9.91498659935558));
#59678=CARTESIAN_POINT('Ctrl Pts',(0.577977468737485,0.555383347305948,
-9.92028213218705));
#59679=CARTESIAN_POINT('Ctrl Pts',(0.652489820552396,0.446320384294988,
-9.92557766501851));
#59680=CARTESIAN_POINT('Ctrl Pts',(0.727002172367308,0.337257421284029,
-9.93087319784997));
#59681=CARTESIAN_POINT('Ctrl Pts',(0.775152486821205,0.209768175345161,
-9.93616873068143));
#59682=CARTESIAN_POINT('Ctrl Pts',(0.788090765422098,0.0792731848705502,
-9.94146426351289));
#59683=CARTESIAN_POINT('Ctrl Pts',(0.813967322623884,-0.181716796078669,
-9.95205532917582));
#59684=CARTESIAN_POINT('Ctrl Pts',(0.698995736413652,-0.454729755170857,
-9.96264639483875));
#59685=CARTESIAN_POINT('Ctrl Pts',(0.494075821794957,-0.619068182027699,
-9.97323746050169));
#59686=CARTESIAN_POINT('Ctrl Pts',(0.391615864485609,-0.701237395456121,
-9.97853299333315));
#59687=CARTESIAN_POINT('Ctrl Pts',(0.266668825074145,-0.756237975825707,
-9.98382852616462));
#59688=CARTESIAN_POINT('Ctrl Pts',(0.136688704257258,-0.778890846190016,
-9.98912405899608));
#59689=CARTESIAN_POINT('Ctrl Pts',(0.00670858344037104,-0.801543716554325,
-9.99441959182754));
#59690=CARTESIAN_POINT('Ctrl Pts',(-0.128304618781938,-0.791848876913358,
-9.99971512465901));
#59691=CARTESIAN_POINT('Ctrl Pts',(-0.252600723751825,-0.749932747605143,
-10.0050106574905));
#59692=CARTESIAN_POINT('Ctrl Pts',(-0.376896828721711,-0.708016618296928,
-10.0103061903219));
#59693=CARTESIAN_POINT('Ctrl Pts',(-0.490475836439174,-0.633879199321465,
-10.0156017231534));
#59694=CARTESIAN_POINT('Ctrl Pts',(-0.580250489386907,-0.537262284470542,
-10.0208972559849));
#59695=CARTESIAN_POINT('Ctrl Pts',(-0.670025142334639,-0.44064536961962,
-10.0261927888163));
#59696=CARTESIAN_POINT('Ctrl Pts',(-0.735995440512639,-0.321548958893238,
-10.0314883216478));
#59697=CARTESIAN_POINT('Ctrl Pts',(-0.767805763296456,-0.194137434313457,
-10.0367838544793));
#59698=CARTESIAN_POINT('Ctrl Pts',(-0.783590174660805,-0.130915318329486,
-10.0394115193783));
#59699=CARTESIAN_POINT('Ctrl Pts',(-0.790963769124703,-0.0656458677288963,
-10.0420391842773));
#59700=CARTESIAN_POINT('Ctrl Pts',(-0.790401422788456,-0.000312835344477125,
-10.0446668491763));
#59701=CARTESIAN_POINT('Ctrl Pts',(-0.791423880525058,-0.000561432253963593,
-10.0731331508237));
#59702=CARTESIAN_POINT('Ctrl Pts',(-0.791738345520185,-0.0591318509064546,
-10.0707736254326));
#59703=CARTESIAN_POINT('Ctrl Pts',(-0.785528842062187,-0.117597404296111,
-10.0684141000415));
#59704=CARTESIAN_POINT('Ctrl Pts',(-0.772503059908576,-0.174522939725115,
-10.0660545746503));
#59705=CARTESIAN_POINT('Ctrl Pts',(-0.714034982125027,-0.430041310451943,
-10.0554635089874));
#59706=CARTESIAN_POINT('Ctrl Pts',(-0.518233131926761,-0.654531537294492,
-10.0448724433245));
#59707=CARTESIAN_POINT('Ctrl Pts',(-0.272253050837869,-0.744429333370331,
-10.0342813776615));
#59708=CARTESIAN_POINT('Ctrl Pts',(-0.0262729697489752,-0.83432712944617,
-10.0236903119986));
#59709=CARTESIAN_POINT('Ctrl Pts',(0.269885342230544,-0.7896324947553,-10.0130992463357));
#59710=CARTESIAN_POINT('Ctrl Pts',(0.478630791197635,-0.631636438988873,
-10.0025081806728));
#59711=CARTESIAN_POINT('Ctrl Pts',(0.687376240164726,-0.473640383222446,
-9.99191711500984));
#59712=CARTESIAN_POINT('Ctrl Pts',(0.808708826119385,-0.202342906380464,
-9.98132604934689));
#59713=CARTESIAN_POINT('Ctrl Pts',(0.789722166415962,0.0596148758645482,
-9.97073498368396));
#59714=CARTESIAN_POINT('Ctrl Pts',(0.78022883656425,0.190593766987052,-9.9654394508525));
#59715=CARTESIAN_POINT('Ctrl Pts',(0.735655695298016,0.319237734460317,
-9.96014391802105));
#59716=CARTESIAN_POINT('Ctrl Pts',(0.663776390394953,0.429816584489825,
-9.95484838518958));
#59717=CARTESIAN_POINT('Ctrl Pts',(0.591897085491888,0.540395434519333,
-9.94955285235812));
#59718=CARTESIAN_POINT('Ctrl Pts',(0.492711616951992,0.632909167105086,
-9.94425731952665));
#59719=CARTESIAN_POINT('Ctrl Pts',(0.377443111951363,0.695516318148622,
-9.93896178669518));
#59720=CARTESIAN_POINT('Ctrl Pts',(0.262174606950734,0.758123469192158,
-9.93366625386372));
#59721=CARTESIAN_POINT('Ctrl Pts',(0.130823065489374,0.790824038693476,
-9.92837072103225));
#59722=CARTESIAN_POINT('Ctrl Pts',(-0.00111625153724639,0.7907929603459,
-9.92307518820079));
#59723=CARTESIAN_POINT('Ctrl Pts',(-0.133055568563865,0.790761881998325,
-9.91777965536932));
#59724=CARTESIAN_POINT('Ctrl Pts',(-0.265582661155748,0.757999155801856,
-9.91248412253786));
#59725=CARTESIAN_POINT('Ctrl Pts',(-0.380613999968237,0.694614507989592,
-9.90718858970639));
#59726=CARTESIAN_POINT('Ctrl Pts',(-0.61067667759322,0.567845212365061,
-9.89659752404346));
#59727=CARTESIAN_POINT('Ctrl Pts',(-0.770756340100645,0.318588230277345,
-9.88600645838054));
#59728=CARTESIAN_POINT('Ctrl Pts',(-0.790012201976854,0.0570264246712957,
-9.87541539271761));
#59729=CARTESIAN_POINT('Ctrl Pts',(-0.791395334265783,0.0382386611730939,
-9.87465464541963));
#59730=CARTESIAN_POINT('Ctrl Pts',(-0.792051896362309,0.019387411829807,
-9.87389389812165));
#59731=CARTESIAN_POINT('Ctrl Pts',(-0.791999899124744,0.000522216889476513,
-9.87313315082368));
#59732=CARTESIAN_POINT('Origin',(0.,0.,-5.925));
#59733=CARTESIAN_POINT('',(-0.790332566743882,0.00078097778472147,-9.6446668491763));
#59734=CARTESIAN_POINT('',(-0.79049273289666,5.48490963145453E-5,-9.67313315082367));
#59735=CARTESIAN_POINT('',(-0.7911,-9.68818082805471E-17,-5.925));
#59736=CARTESIAN_POINT('Ctrl Pts',(-0.790332566743882,0.00078097778472147,
-9.6446668491763));
#59737=CARTESIAN_POINT('Ctrl Pts',(-0.791021644760839,0.0909049416404772,
-9.64827972965547));
#59738=CARTESIAN_POINT('Ctrl Pts',(-0.776890865898073,0.180795718990353,
-9.65189261013465));
#59739=CARTESIAN_POINT('Ctrl Pts',(-0.747041992130169,0.265000034088506,
-9.65550549061382));
#59740=CARTESIAN_POINT('Ctrl Pts',(-0.659540790841399,0.511842805513576,
-9.66609655627675));
#59741=CARTESIAN_POINT('Ctrl Pts',(-0.436965503137771,0.709818732819205,
-9.67668762193967));
#59742=CARTESIAN_POINT('Ctrl Pts',(-0.182027863912829,0.77076915533624,
-9.6872786876026));
#59743=CARTESIAN_POINT('Ctrl Pts',(-0.0545590443003537,0.801244366594759,
-9.69257422043406));
#59744=CARTESIAN_POINT('Ctrl Pts',(0.0810003631924518,0.797463201656127,
-9.69786975326553));
#59745=CARTESIAN_POINT('Ctrl Pts',(0.208395166807512,0.762572164331347,
-9.703165286097));
#59746=CARTESIAN_POINT('Ctrl Pts',(0.335789970422572,0.727681127006567,
-9.70846081892846));
#59747=CARTESIAN_POINT('Ctrl Pts',(0.455020170159888,0.661680217295637,
-9.71375635175992));
#59748=CARTESIAN_POINT('Ctrl Pts',(0.549357855553091,0.570593759977461,
-9.71905188459139));
#59749=CARTESIAN_POINT('Ctrl Pts',(0.738033226339499,0.388420845341107,
-9.72964295025431));
#59750=CARTESIAN_POINT('Ctrl Pts',(0.827138539749452,0.105905740275768,
-9.74023401591724));
#59751=CARTESIAN_POINT('Ctrl Pts',(0.777335341547127,-0.152006902682922,
-9.75082508158017));
#59752=CARTESIAN_POINT('Ctrl Pts',(0.752433742445964,-0.280963224162265,
-9.75612061441164));
#59753=CARTESIAN_POINT('Ctrl Pts',(0.692805015441732,-0.403768930114946,
-9.76141614724311));
#59754=CARTESIAN_POINT('Ctrl Pts',(0.608399751564134,-0.505177686014364,
-9.76671168007457));
#59755=CARTESIAN_POINT('Ctrl Pts',(0.523994487686536,-0.606586441913781,
-9.77200721290603));
#59756=CARTESIAN_POINT('Ctrl Pts',(0.414812686935571,-0.686598247759937,
-9.77730274573749));
#59757=CARTESIAN_POINT('Ctrl Pts',(0.292940829352205,-0.735113543657704,
-9.78259827856896));
#59758=CARTESIAN_POINT('Ctrl Pts',(0.17106897176884,-0.78362883955547,-9.78789381140042));
#59759=CARTESIAN_POINT('Ctrl Pts',(0.0365070573530715,-0.800647625504847,
-9.79318934423189));
#59760=CARTESIAN_POINT('Ctrl Pts',(-0.0944635525894151,-0.785122939405312,
-9.79848487706336));
#59761=CARTESIAN_POINT('Ctrl Pts',(-0.225434162531902,-0.769598253305778,
-9.80378040989482));
#59762=CARTESIAN_POINT('Ctrl Pts',(-0.352813468001109,-0.721530095157332,
-9.80907594272628));
#59763=CARTESIAN_POINT('Ctrl Pts',(-0.459539163038184,-0.645010690754216,
-9.81437147555775));
#59764=CARTESIAN_POINT('Ctrl Pts',(-0.663062579771367,-0.499089967304251,
-9.82446993343059));
#59765=CARTESIAN_POINT('Ctrl Pts',(-0.791477897958024,-0.249704572895693,
-9.83456839130345));
#59766=CARTESIAN_POINT('Ctrl Pts',(-0.792437169753526,-0.000127296230932911,
-9.8446668491763));
#59767=CARTESIAN_POINT('Ctrl Pts',(-0.791999899124744,0.000522216889476513,
-9.87313315082368));
#59768=CARTESIAN_POINT('Ctrl Pts',(-0.791689945581274,-0.111932488278983,
-9.86859836529019));
#59769=CARTESIAN_POINT('Ctrl Pts',(-0.766202707297937,-0.224882723250992,
-9.8640635797567));
#59770=CARTESIAN_POINT('Ctrl Pts',(-0.719353086501239,-0.327835306675267,
-9.85952879422322));
#59771=CARTESIAN_POINT('Ctrl Pts',(-0.664644059307214,-0.448059026536213,
-9.85423326139175));
#59772=CARTESIAN_POINT('Ctrl Pts',(-0.580804024138859,-0.554649357575498,
-9.84893772856028));
#59773=CARTESIAN_POINT('Ctrl Pts',(-0.475816889973955,-0.633101509454781,
-9.84364219572882));
#59774=CARTESIAN_POINT('Ctrl Pts',(-0.26584262164415,-0.790005813213344,
-9.83305113006589));
#59775=CARTESIAN_POINT('Ctrl Pts',(0.0287200426718578,-0.834357400331918,
-9.82246006440296));
#59776=CARTESIAN_POINT('Ctrl Pts',(0.274399357588069,-0.743640873424784,
-9.81186899874004));
#59777=CARTESIAN_POINT('Ctrl Pts',(0.520078672504281,-0.652924346517651,
-9.80127793307711));
#59778=CARTESIAN_POINT('Ctrl Pts',(0.716874638020693,-0.42713970558481,
-9.79068686741418));
#59779=CARTESIAN_POINT('Ctrl Pts',(0.773699372663501,-0.171584690695658,
-9.78009580175124));
#59780=CARTESIAN_POINT('Ctrl Pts',(0.830524107306308,0.0839703241934938,
-9.76950473608831));
#59781=CARTESIAN_POINT('Ctrl Pts',(0.747377611075511,0.369295713038955,
-9.75891367042538));
#59782=CARTESIAN_POINT('Ctrl Pts',(0.563327148374181,0.556666468774327,
-9.74832260476246));
#59783=CARTESIAN_POINT('Ctrl Pts',(0.471301917023517,0.650351846642012,
-9.743027071931));
#59784=CARTESIAN_POINT('Ctrl Pts',(0.354050694055216,0.719548566232178,
-9.73773153909954));
#59785=CARTESIAN_POINT('Ctrl Pts',(0.227681461481029,0.757299508019194,
-9.73243600626807));
#59786=CARTESIAN_POINT('Ctrl Pts',(0.101312228906838,0.795050449806211,
-9.7271404734366));
#59787=CARTESIAN_POINT('Ctrl Pts',(-0.0341750132732382,0.80135561379008,
-9.72184494060513));
#59788=CARTESIAN_POINT('Ctrl Pts',(-0.162560500119688,0.774454863353173,
-9.71654940777367));
#59789=CARTESIAN_POINT('Ctrl Pts',(-0.290945986966133,0.747554112916268,
-9.7112538749422));
#59790=CARTESIAN_POINT('Ctrl Pts',(-0.412229718478951,0.687447448058585,
-9.70595834211075));
#59791=CARTESIAN_POINT('Ctrl Pts',(-0.512772535588132,0.602012523870264,
-9.70066280927928));
#59792=CARTESIAN_POINT('Ctrl Pts',(-0.613315352697312,0.516577599681943,
-9.69536727644782));
#59793=CARTESIAN_POINT('Ctrl Pts',(-0.693117255402863,0.405814416162977,
-9.69007174361635));
#59794=CARTESIAN_POINT('Ctrl Pts',(-0.739760880099864,0.283037403809672,
-9.68477621078488));
#59795=CARTESIAN_POINT('Ctrl Pts',(-0.77394532300293,0.193055894099291,
-9.68089519079781));
#59796=CARTESIAN_POINT('Ctrl Pts',(-0.790319746311059,0.0966215002284446,
-9.67701417081074));
#59797=CARTESIAN_POINT('Ctrl Pts',(-0.7897370361882,0.00012310453410933,
-9.67313315082366));
#59798=CARTESIAN_POINT('Origin',(0.,0.,-5.925));
#59799=CARTESIAN_POINT('',(-0.790129111244616,-0.000602373567983761,-9.44466684917629));
#59800=CARTESIAN_POINT('',(-0.791100127608287,-3.17057992569413E-5,-9.47313315082365));
#59801=CARTESIAN_POINT('',(-0.7911,-9.68818082805471E-17,-5.925));
#59802=CARTESIAN_POINT('Ctrl Pts',(-0.790129111244616,-0.00060237356798376,
-9.44466684917629));
#59803=CARTESIAN_POINT('Ctrl Pts',(-0.78877350216917,0.166988129555797,
-9.45140000234455));
#59804=CARTESIAN_POINT('Ctrl Pts',(-0.736146428833839,0.335184335378372,
-9.45813315551282));
#59805=CARTESIAN_POINT('Ctrl Pts',(-0.637699246421988,0.469636992975678,
-9.46486630868108));
#59806=CARTESIAN_POINT('Ctrl Pts',(-0.560271884590339,0.575382168347607,
-9.47016184151255));
#59807=CARTESIAN_POINT('Ctrl Pts',(-0.454502002845351,0.660254910048017,
-9.47545737434402));
#59808=CARTESIAN_POINT('Ctrl Pts',(-0.334816055928803,0.716130616615437,
-9.48075290717549));
#59809=CARTESIAN_POINT('Ctrl Pts',(-0.215130109012256,0.772006323182857,
-9.48604844000695));
#59810=CARTESIAN_POINT('Ctrl Pts',(-0.0815280969241502,0.798884994617287,
-9.49134397283841));
#59811=CARTESIAN_POINT('Ctrl Pts',(0.0493402593592206,0.790529462568899,
-9.49663950566987));
#59812=CARTESIAN_POINT('Ctrl Pts',(0.311076971925962,0.773818398472124,
-9.5072305713328));
#59813=CARTESIAN_POINT('Ctrl Pts',(0.561879061273764,0.616170520444079,
-9.51782163699574));
#59814=CARTESIAN_POINT('Ctrl Pts',(0.690879895303411,0.387351651535129,
-9.52841270265866));
#59815=CARTESIAN_POINT('Ctrl Pts',(0.755380312318234,0.272942217080654,
-9.53370823549013));
#59816=CARTESIAN_POINT('Ctrl Pts',(0.789430415503518,0.140740034905953,
-9.53900376832159));
#59817=CARTESIAN_POINT('Ctrl Pts',(0.7907447023627,0.00880726038284042,
-9.54429930115306));
#59818=CARTESIAN_POINT('Ctrl Pts',(0.792058989221882,-0.123125514140272,
-9.54959483398452));
#59819=CARTESIAN_POINT('Ctrl Pts',(0.760637459754962,-0.254788881011797,
-9.55489036681599));
#59820=CARTESIAN_POINT('Ctrl Pts',(0.699154343482463,-0.370660836291279,
-9.56018589964745));
#59821=CARTESIAN_POINT('Ctrl Pts',(0.637671227209964,-0.486532791570762,
-9.56548143247892));
#59822=CARTESIAN_POINT('Ctrl Pts',(0.546126524131887,-0.586613335258203,
-9.57077696531037));
#59823=CARTESIAN_POINT('Ctrl Pts',(0.43625198486056,-0.659564703765652,
-9.57607249814184));
#59824=CARTESIAN_POINT('Ctrl Pts',(0.326377445589232,-0.732516072273101,
-9.58136803097331));
#59825=CARTESIAN_POINT('Ctrl Pts',(0.198173070124655,-0.778338265600559,
-9.58666356380478));
#59826=CARTESIAN_POINT('Ctrl Pts',(0.0672927036574521,-0.789105015563541,
-9.59195909663625));
#59827=CARTESIAN_POINT('Ctrl Pts',(-0.194468029276953,-0.810638515489503,
-9.60255016229918));
#59828=CARTESIAN_POINT('Ctrl Pts',(-0.466932726221856,-0.691950241957559,
-9.61314122796209));
#59829=CARTESIAN_POINT('Ctrl Pts',(-0.626951517257354,-0.484751297419327,
-9.62373229362501));
#59830=CARTESIAN_POINT('Ctrl Pts',(-0.732383849778435,-0.348233155536065,
-9.63071047880877));
#59831=CARTESIAN_POINT('Ctrl Pts',(-0.78900163037992,-0.173291126981858,
-9.63768866399253));
#59832=CARTESIAN_POINT('Ctrl Pts',(-0.790332566743882,0.00078097778472147,
-9.6446668491763));
#59833=CARTESIAN_POINT('Ctrl Pts',(-0.7911,-5.95412608106471E-13,-9.67313315082367));
#59834=CARTESIAN_POINT('Ctrl Pts',(-0.791099999999834,-0.220167589667271,
-9.6642744072504));
#59835=CARTESIAN_POINT('Ctrl Pts',(-0.694214576672042,-0.438610418339204,
-9.65541566367713));
#59836=CARTESIAN_POINT('Ctrl Pts',(-0.531017389079889,-0.586395551223556,
-9.64655692010385));
#59837=CARTESIAN_POINT('Ctrl Pts',(-0.367820201487736,-0.734180684107907,
-9.63769817653058));
#59838=CARTESIAN_POINT('Ctrl Pts',(-0.140868175871139,-0.808992666571442,
-9.62883943295731));
#59839=CARTESIAN_POINT('Ctrl Pts',(0.0782205473253529,-0.787223447298238,
-9.61998068938404));
#59840=CARTESIAN_POINT('Ctrl Pts',(0.297309270521845,-0.765454228025035,
-9.61112194581076));
#59841=CARTESIAN_POINT('Ctrl Pts',(0.505102072676084,-0.647444880833849,
-9.60226320223749));
#59842=CARTESIAN_POINT('Ctrl Pts',(0.636026795762087,-0.470435038100494,
-9.59340445866422));
#59843=CARTESIAN_POINT('Ctrl Pts',(0.766951518848089,-0.293425195367138,
-9.58454571509095));
#59844=CARTESIAN_POINT('Ctrl Pts',(0.818956872247116,-0.0601881960093101,
-9.57568697151767));
#59845=CARTESIAN_POINT('Ctrl Pts',(0.775631781004092,0.15567450111184,-9.5668282279444));
#59846=CARTESIAN_POINT('Ctrl Pts',(0.732306689761068,0.37153719823299,-9.55796948437113));
#59847=CARTESIAN_POINT('Ctrl Pts',(0.594329958849784,0.566643518936949,
-9.54911074079786));
#59848=CARTESIAN_POINT('Ctrl Pts',(0.405242230243525,0.679424716085053,
-9.54025199722458));
#59849=CARTESIAN_POINT('Ctrl Pts',(0.216154501637265,0.792205913233156,
-9.53139325365131));
#59850=CARTESIAN_POINT('Ctrl Pts',(-0.0210816529306389,0.820894963712987,
-9.52253451007804));
#59851=CARTESIAN_POINT('Ctrl Pts',(-0.231602780753791,0.756438604215247,
-9.51367576650476));
#59852=CARTESIAN_POINT('Ctrl Pts',(-0.442123908576943,0.691982244717508,
-9.50481702293149));
#59853=CARTESIAN_POINT('Ctrl Pts',(-0.622631625634579,0.535390358803066,
-9.49595827935822));
#59854=CARTESIAN_POINT('Ctrl Pts',(-0.716163994722408,0.336077881841758,
-9.48709953578495));
#59855=CARTESIAN_POINT('Ctrl Pts',(-0.765317280859656,0.231334857513964,
-9.48244407413119));
#59856=CARTESIAN_POINT('Ctrl Pts',(-0.791100000000083,0.115702837835949,
-9.47778861247743));
#59857=CARTESIAN_POINT('Ctrl Pts',(-0.7911,-5.67157432129761E-13,-9.47313315082367));
#59858=CARTESIAN_POINT('Origin',(0.,0.,-5.925));
#59859=CARTESIAN_POINT('',(-0.791985506391904,-0.000137013821822907,-9.2446668491763));
#59860=CARTESIAN_POINT('',(-0.791291464171058,-0.000172660802811795,-9.27313315082367));
#59861=CARTESIAN_POINT('',(-0.7911,-9.68818082805471E-17,-5.925));
#59862=CARTESIAN_POINT('Ctrl Pts',(-0.791985506391904,-0.000137013821822907,
-9.2446668491763));
#59863=CARTESIAN_POINT('Ctrl Pts',(-0.791786526522987,0.112700469452395,
-9.24922474220219));
#59864=CARTESIAN_POINT('Ctrl Pts',(-0.766166379387017,0.225741947610222,
-9.25378263522809));
#59865=CARTESIAN_POINT('Ctrl Pts',(-0.718782612796448,0.329084194247059,
-9.25834052825398));
#59866=CARTESIAN_POINT('Ctrl Pts',(-0.663730357240334,0.449151132377018,
-9.26363606108544));
#59867=CARTESIAN_POINT('Ctrl Pts',(-0.579300103659578,0.556125395133812,
-9.2689315939169));
#59868=CARTESIAN_POINT('Ctrl Pts',(-0.474144470433553,0.634474832866043,
-9.27422712674836));
#59869=CARTESIAN_POINT('Ctrl Pts',(-0.263833203981505,0.791173708330505,
-9.28481819241128));
#59870=CARTESIAN_POINT('Ctrl Pts',(0.0293795810516175,0.833373283696715,
-9.29540925807423));
#59871=CARTESIAN_POINT('Ctrl Pts',(0.27582928125095,0.742478645676782,-9.30600032373715));
#59872=CARTESIAN_POINT('Ctrl Pts',(0.399054131350617,0.697031326666815,
-9.31129585656862));
#59873=CARTESIAN_POINT('Ctrl Pts',(0.510588210241836,0.618310454310313,
-9.31659138940007));
#59874=CARTESIAN_POINT('Ctrl Pts',(0.596996948867665,0.518603311976337,
-9.32188692223154));
#59875=CARTESIAN_POINT('Ctrl Pts',(0.683405687493494,0.41889616964236,-9.327182455063));
#59876=CARTESIAN_POINT('Ctrl Pts',(0.744689085853934,0.298202757330909,
-9.33247798789447));
#59877=CARTESIAN_POINT('Ctrl Pts',(0.772837210270715,0.170084972856288,
-9.33777352072594));
#59878=CARTESIAN_POINT('Ctrl Pts',(0.800985334687495,0.0419671883816674,
-9.34306905355741));
#59879=CARTESIAN_POINT('Ctrl Pts',(0.795998185160616,-0.0935749682561238,
-9.34836458638886));
#59880=CARTESIAN_POINT('Ctrl Pts',(0.759478065537175,-0.220305380588309,
-9.35366011922033));
#59881=CARTESIAN_POINT('Ctrl Pts',(0.722957945913735,-0.347035792920495,
-9.35895565205179));
#59882=CARTESIAN_POINT('Ctrl Pts',(0.654904856193732,-0.464954460947075,
-9.36425118488326));
#59883=CARTESIAN_POINT('Ctrl Pts',(0.562118924507943,-0.557886501237572,
-9.36954671771473));
#59884=CARTESIAN_POINT('Ctrl Pts',(0.376547061136364,-0.743750581818566,
-9.38013778337766));
#59885=CARTESIAN_POINT('Ctrl Pts',(0.0920438299016367,-0.82966815145523,
-9.39072884904058));
#59886=CARTESIAN_POINT('Ctrl Pts',(-0.164051761844405,-0.775331570862921,
-9.40131991470351));
#59887=CARTESIAN_POINT('Ctrl Pts',(-0.420147353590447,-0.720994990270612,
-9.41191098036644));
#59888=CARTESIAN_POINT('Ctrl Pts',(-0.647835305847804,-0.52640425944933,
-9.42250204602937));
#59889=CARTESIAN_POINT('Ctrl Pts',(-0.740936959971514,-0.281618851323722,
-9.4330931116923));
#59890=CARTESIAN_POINT('Ctrl Pts',(-0.774850264463147,-0.192453066257844,
-9.43695102418697));
#59891=CARTESIAN_POINT('Ctrl Pts',(-0.790905838144978,-0.0966271452954019,
-9.44080893668163));
#59892=CARTESIAN_POINT('Ctrl Pts',(-0.790129111244616,-0.00060237356798376,
-9.44466684917629));
#59893=CARTESIAN_POINT('Ctrl Pts',(-0.791100561757637,-0.000139575345601312,
-9.47313315082367));
#59894=CARTESIAN_POINT('Ctrl Pts',(-0.791433680411738,-0.0896913779101309,
-9.46954337783691));
#59895=CARTESIAN_POINT('Ctrl Pts',(-0.776842562758261,-0.17925244583268,
-9.46595360485014));
#59896=CARTESIAN_POINT('Ctrl Pts',(-0.747063898241547,-0.263157488256723,
-9.46236383186337));
#59897=CARTESIAN_POINT('Ctrl Pts',(-0.659206590157331,-0.510706237729051,
-9.45177276620044));
#59898=CARTESIAN_POINT('Ctrl Pts',(-0.439148817318704,-0.709021940791804,
-9.44118170053751));
#59899=CARTESIAN_POINT('Ctrl Pts',(-0.184153391517759,-0.770362785170478,
-9.43059063487458));
#59900=CARTESIAN_POINT('Ctrl Pts',(-0.0566556786172914,-0.801033207359814,
-9.42529510204312));
#59901=CARTESIAN_POINT('Ctrl Pts',(0.0795764475237638,-0.797459914878131,
-9.41999956921166));
#59902=CARTESIAN_POINT('Ctrl Pts',(0.20707040698932,-0.762932957677804,
-9.41470403638019));
#59903=CARTESIAN_POINT('Ctrl Pts',(0.334564366454881,-0.728406000477477,
-9.40940850354873));
#59904=CARTESIAN_POINT('Ctrl Pts',(0.453320159244951,-0.662925378558506,
-9.40411297071726));
#59905=CARTESIAN_POINT('Ctrl Pts',(0.547731929316479,-0.572021824466215,
-9.3988174378858));
#59906=CARTESIAN_POINT('Ctrl Pts',(0.736555469459537,-0.390214716281634,
-9.38822637222287));
#59907=CARTESIAN_POINT('Ctrl Pts',(0.828002918728424,-0.106715879403781,
-9.37763530655994));
#59908=CARTESIAN_POINT('Ctrl Pts',(0.778250780715013,0.150407707213407,
-9.36704424089701));
#59909=CARTESIAN_POINT('Ctrl Pts',(0.728498642701604,0.407531293830588,
-9.35645317523408));
#59910=CARTESIAN_POINT('Ctrl Pts',(0.537546917405906,0.638279630187101,
-9.34586210957115));
#59911=CARTESIAN_POINT('Ctrl Pts',(0.294560327079297,0.735721577128167,
-9.33527104390822));
#59912=CARTESIAN_POINT('Ctrl Pts',(0.051573736752682,0.833163524069235,
-9.32467997824529));
#59913=CARTESIAN_POINT('Ctrl Pts',(-0.243447718604854,0.797299081594843,
-9.31408891258236));
#59914=CARTESIAN_POINT('Ctrl Pts',(-0.458139645376263,0.646005494471663,
-9.30349784691943));
#59915=CARTESIAN_POINT('Ctrl Pts',(-0.565485608761967,0.570358700910073,
-9.29820231408797));
#59916=CARTESIAN_POINT('Ctrl Pts',(-0.65274919000114,0.465854621186288,
-9.29290678125651));
#59917=CARTESIAN_POINT('Ctrl Pts',(-0.710457625152268,0.347262660836506,
-9.28761124842504));
#59918=CARTESIAN_POINT('Ctrl Pts',(-0.763049648349371,0.239185026893182,
-9.28278521589125));
#59919=CARTESIAN_POINT('Ctrl Pts',(-0.791094906196155,0.119406828216415,
-9.27795918335746));
#59920=CARTESIAN_POINT('Ctrl Pts',(-0.791291464171058,-0.000172660802811794,
-9.27313315082367));
#59921=CARTESIAN_POINT('Origin',(0.,0.,-5.925));
#59922=CARTESIAN_POINT('',(-0.791150637177402,0.000157610601749369,-9.0446668491763));
#59923=CARTESIAN_POINT('',(-0.791456073972705,0.000283146808428445,-9.07313315082367));
#59924=CARTESIAN_POINT('',(-0.7911,-9.68818082805471E-17,-5.925));
#59925=CARTESIAN_POINT('Ctrl Pts',(-0.791308228660122,0.000648121520882616,
-9.0446668491763));
#59926=CARTESIAN_POINT('Ctrl Pts',(-0.791650333819295,0.0599578818431041,
-9.04704948205981));
#59927=CARTESIAN_POINT('Ctrl Pts',(-0.785358429788104,0.119155442284125,
-9.04943211494333));
#59928=CARTESIAN_POINT('Ctrl Pts',(-0.772117381331553,0.176652319058692,
-9.05181474782685));
#59929=CARTESIAN_POINT('Ctrl Pts',(-0.713259462170178,0.432232270777294,
-9.06240581348978));
#59930=CARTESIAN_POINT('Ctrl Pts',(-0.51709336754244,0.654208406401072,
-9.07299687915271));
#59931=CARTESIAN_POINT('Ctrl Pts',(-0.270410805205285,0.744469158602069,
-9.08358794481564));
#59932=CARTESIAN_POINT('Ctrl Pts',(-0.147069524036703,0.78959953470257,
-9.0888834776471));
#59933=CARTESIAN_POINT('Ctrl Pts',(-0.0110991259407661,0.801801064947372,
-9.09417901047857));
#59934=CARTESIAN_POINT('Ctrl Pts',(0.119306481265527,0.781742103048164,
-9.09947454331003));
#59935=CARTESIAN_POINT('Ctrl Pts',(0.249712088471816,0.761683141148956,
-9.1047700761415));
#59936=CARTESIAN_POINT('Ctrl Pts',(0.37455290478846,0.709363687105741,-9.11006560897296));
#59937=CARTESIAN_POINT('Ctrl Pts',(0.478944504916685,0.629935244910663,
-9.11536114180442));
#59938=CARTESIAN_POINT('Ctrl Pts',(0.583336105044909,0.550506802715584,
-9.12065667463589));
#59939=CARTESIAN_POINT('Ctrl Pts',(0.667278488984713,0.443969372368644,
-9.12595220746735));
#59940=CARTESIAN_POINT('Ctrl Pts',(0.72148242867828,0.323735228013172,-9.13124774029882));
#59941=CARTESIAN_POINT('Ctrl Pts',(0.775686368371847,0.2035010836577,-9.13654327313028));
#59942=CARTESIAN_POINT('Ctrl Pts',(0.800151863819177,0.0695702252936993,
-9.14183880596175));
#59943=CARTESIAN_POINT('Ctrl Pts',(0.789591060252161,-0.061326920050932,
-9.14713433879322));
#59944=CARTESIAN_POINT('Ctrl Pts',(0.768469453118131,-0.323121210740191,
-9.15772540445615));
#59945=CARTESIAN_POINT('Ctrl Pts',(0.60724264992672,-0.572780649351978,
-9.16831647011907));
#59946=CARTESIAN_POINT('Ctrl Pts',(0.376874024690652,-0.697149908451897,
-9.178907535782));
#59947=CARTESIAN_POINT('Ctrl Pts',(0.146505399454581,-0.821519167551817,
-9.18949860144492));
#59948=CARTESIAN_POINT('Ctrl Pts',(-0.153005047826149,-0.820598247139874,
-9.20008966710786));
#59949=CARTESIAN_POINT('Ctrl Pts',(-0.382428700634536,-0.694294638466769,
-9.21068073277079));
#59950=CARTESIAN_POINT('Ctrl Pts',(-0.611852353442922,-0.567991029793665,
-9.22127179843372));
#59951=CARTESIAN_POINT('Ctrl Pts',(-0.771189211778961,-0.316304732859401,
-9.23186286409664));
#59952=CARTESIAN_POINT('Ctrl Pts',(-0.790069154515677,-0.0548631492104814,
-9.24245392975957));
#59953=CARTESIAN_POINT('Ctrl Pts',(-0.791384092760116,-0.0366544320644326,
-9.24319156956515));
#59954=CARTESIAN_POINT('Ctrl Pts',(-0.792017708874715,-0.0183983944095057,
-9.24392920937072));
#59955=CARTESIAN_POINT('Ctrl Pts',(-0.791985506391904,-0.000137013821822907,
-9.2446668491763));
#59956=CARTESIAN_POINT('Ctrl Pts',(-0.791291464171058,-0.000172660802811794,
-9.27313315082367));
#59957=CARTESIAN_POINT('Ctrl Pts',(-0.79131058630235,-0.0118059445192655,
-9.27266365052599));
#59958=CARTESIAN_POINT('Ctrl Pts',(-0.791066138311347,-0.0234373475759765,
-9.27219415022832));
#59959=CARTESIAN_POINT('Ctrl Pts',(-0.790555079975775,-0.035055913838341,
-9.27172464993064));
#59960=CARTESIAN_POINT('Ctrl Pts',(-0.784790810585072,-0.166102687187628,
-9.26642911709918));
#59961=CARTESIAN_POINT('Ctrl Pts',(-0.745108982740585,-0.295516392910425,
-9.26113358426772));
#59962=CARTESIAN_POINT('Ctrl Pts',(-0.67707559581834,-0.408562589693877,
-9.25583805143626));
#59963=CARTESIAN_POINT('Ctrl Pts',(-0.609042208896096,-0.521608786477329,
-9.25054251860479));
#59964=CARTESIAN_POINT('Ctrl Pts',(-0.512657262896095,-0.618287474321436,
-9.24524698577332));
#59965=CARTESIAN_POINT('Ctrl Pts',(-0.399049604828334,-0.684189845414118,
-9.23995145294186));
#59966=CARTESIAN_POINT('Ctrl Pts',(-0.171834288692815,-0.815994587599481,
-9.22936038727893));
#59967=CARTESIAN_POINT('Ctrl Pts',(0.124271875713755,-0.824694062779146,
-9.21876932161601));
#59968=CARTESIAN_POINT('Ctrl Pts',(0.358336191702969,-0.706375584302658,
-9.20817825595308));
#59969=CARTESIAN_POINT('Ctrl Pts',(0.475368349697578,-0.647216345064414,
-9.20288272312161));
#59970=CARTESIAN_POINT('Ctrl Pts',(0.57689004558785,-0.55630261741213,-9.19758719029014));
#59971=CARTESIAN_POINT('Ctrl Pts',(0.651713661232107,-0.447452964148376,
-9.19229165745868));
#59972=CARTESIAN_POINT('Ctrl Pts',(0.726537276876364,-0.338603310884622,
-9.18699612462721));
#59973=CARTESIAN_POINT('Ctrl Pts',(0.774662812274606,-0.211817732009396,
-9.18170059179575));
#59974=CARTESIAN_POINT('Ctrl Pts',(0.787775960383391,-0.0814141897978206,
-9.17640505896428));
#59975=CARTESIAN_POINT('Ctrl Pts',(0.814002256600962,0.179392894625334,
-9.16581399330136));
#59976=CARTESIAN_POINT('Ctrl Pts',(0.700179003660705,0.454671832393888,
-9.15522292763843));
#59977=CARTESIAN_POINT('Ctrl Pts',(0.495808804183578,0.61844190169067,-9.1446318619755));
#59978=CARTESIAN_POINT('Ctrl Pts',(0.291438604706456,0.782211970987448,
-9.13404079631256));
#59979=CARTESIAN_POINT('Ctrl Pts',(-0.00347854130752701,0.83447317181246,
-9.12344973064964));
#59980=CARTESIAN_POINT('Ctrl Pts',(-0.251759969397478,0.751444570909924,
-9.11285866498671));
#59981=CARTESIAN_POINT('Ctrl Pts',(-0.500041397487433,0.668415970007387,
-9.10226759932378));
#59982=CARTESIAN_POINT('Ctrl Pts',(-0.701687107653353,0.450097567377298,
-9.09167653366085));
#59983=CARTESIAN_POINT('Ctrl Pts',(-0.767383052384056,0.195801645720345,
-9.08108546799792));
#59984=CARTESIAN_POINT('Ctrl Pts',(-0.783825684510273,0.132155490571162,
-9.07843469560651));
#59985=CARTESIAN_POINT('Ctrl Pts',(-0.791752152589477,0.0662556319819147,
-9.07578392321509));
#59986=CARTESIAN_POINT('Ctrl Pts',(-0.791456073972705,0.000283146808428445,
-9.07313315082367));
#59987=CARTESIAN_POINT('Origin',(0.,0.,-5.925));
#59988=CARTESIAN_POINT('',(-0.7911,-5.02375918642883E-14,-8.84466684917629));
#59989=CARTESIAN_POINT('',(-0.790337230870817,0.000108444134415879,-8.87313315082367));
#59990=CARTESIAN_POINT('',(-0.7911,-9.68818082805471E-17,-5.925));
#59991=CARTESIAN_POINT('Ctrl Pts',(-0.7911,-3.90243393155743E-14,-8.84466684917629));
#59992=CARTESIAN_POINT('Ctrl Pts',(-0.791100000000011,0.220167589666633,
-8.85352559274957));
#59993=CARTESIAN_POINT('Ctrl Pts',(-0.694214576672397,0.43861041833864,
-8.86238433632284));
#59994=CARTESIAN_POINT('Ctrl Pts',(-0.531017389080368,0.586395551223122,
-8.87124307989611));
#59995=CARTESIAN_POINT('Ctrl Pts',(-0.367820201488338,0.734180684107605,
-8.88010182346938));
#59996=CARTESIAN_POINT('Ctrl Pts',(-0.140868175871807,0.808992666571324,
-8.88896056704266));
#59997=CARTESIAN_POINT('Ctrl Pts',(0.0782205473246991,0.787223447298303,
-8.89781931061593));
#59998=CARTESIAN_POINT('Ctrl Pts',(0.297309270521205,0.765454228025282,
-8.9066780541892));
#59999=CARTESIAN_POINT('Ctrl Pts',(0.50510207267554,0.647444880834273,-8.91553679776247));
#60000=CARTESIAN_POINT('Ctrl Pts',(0.636026795761689,0.470435038101031,
-8.92439554133574));
#60001=CARTESIAN_POINT('Ctrl Pts',(0.766951518847839,0.293425195367788,
-8.93325428490902));
#60002=CARTESIAN_POINT('Ctrl Pts',(0.818956872247063,0.0601881960100098,
-8.94211302848229));
#60003=CARTESIAN_POINT('Ctrl Pts',(0.775631781004226,-0.155674501111174,
-8.95097177205556));
#60004=CARTESIAN_POINT('Ctrl Pts',(0.732306689761388,-0.371537198232358,
-8.95983051562884));
#60005=CARTESIAN_POINT('Ctrl Pts',(0.594329958850275,-0.566643518936432,
-8.96868925920211));
#60006=CARTESIAN_POINT('Ctrl Pts',(0.405242230244118,-0.679424716084699,
-8.97754800277538));
#60007=CARTESIAN_POINT('Ctrl Pts',(0.21615450163796,-0.792205913232966,
-8.98640674634865));
#60008=CARTESIAN_POINT('Ctrl Pts',(-0.0210816529299142,-0.820894963713004,
-8.99526548992193));
#60009=CARTESIAN_POINT('Ctrl Pts',(-0.23160278075312,-0.756438604215453,
-9.0041242334952));
#60010=CARTESIAN_POINT('Ctrl Pts',(-0.442123908576326,-0.691982244717901,
-9.01298297706847));
#60011=CARTESIAN_POINT('Ctrl Pts',(-0.622631625634097,-0.535390358803624,
-9.02184172064174));
#60012=CARTESIAN_POINT('Ctrl Pts',(-0.716163994722105,-0.336077881842404,
-9.03070046421501));
#60013=CARTESIAN_POINT('Ctrl Pts',(-0.765317280859466,-0.231334857514613,
-9.03535592586877));
#60014=CARTESIAN_POINT('Ctrl Pts',(-0.791099999999998,-0.115702837836572,
-9.04001138752253));
#60015=CARTESIAN_POINT('Ctrl Pts',(-0.7911,-1.11022302462516E-14,-9.04466684917629));
#60016=CARTESIAN_POINT('Ctrl Pts',(-0.791456073972705,0.000283146808428445,
-9.07313315082367));
#60017=CARTESIAN_POINT('Ctrl Pts',(-0.791160666862189,-0.0655397127790337,
-9.07048839038363));
#60018=CARTESIAN_POINT('Ctrl Pts',(-0.782679968229602,-0.131434869890149,
-9.06784362994358));
#60019=CARTESIAN_POINT('Ctrl Pts',(-0.766305602181184,-0.195236054083216,
-9.06519886950353));
#60020=CARTESIAN_POINT('Ctrl Pts',(-0.73351964860641,-0.322983452473125,
-9.05990333667207));
#60021=CARTESIAN_POINT('Ctrl Pts',(-0.669087210450313,-0.442335908667745,
-9.0546078038406));
#60022=CARTESIAN_POINT('Ctrl Pts',(-0.579860291012648,-0.538487042069976,
-9.04931227100913));
#60023=CARTESIAN_POINT('Ctrl Pts',(-0.490633371574989,-0.634638175472201,
-9.04401673817767));
#60024=CARTESIAN_POINT('Ctrl Pts',(-0.376611970855764,-0.707587986082038,
-9.0387212053462));
#60025=CARTESIAN_POINT('Ctrl Pts',(-0.251576818747605,-0.749709181228937,
-9.03342567251474));
#60026=CARTESIAN_POINT('Ctrl Pts',(-0.126541666639438,-0.791830376375839,
-9.02813013968327));
#60027=CARTESIAN_POINT('Ctrl Pts',(0.00950723685766419,-0.803122956059799,
-9.02283460685182));
#60028=CARTESIAN_POINT('Ctrl Pts',(0.138760010107436,-0.779808945368305,
-9.01753907402035));
#60029=CARTESIAN_POINT('Ctrl Pts',(0.397265556606972,-0.733180923985319,
-9.00694800835743));
#60030=CARTESIAN_POINT('Ctrl Pts',(0.628586582117184,-0.548126541100527,
-8.99635694269448));
#60031=CARTESIAN_POINT('Ctrl Pts',(0.730394500479292,-0.306423181323989,
-8.98576587703155));
#60032=CARTESIAN_POINT('Ctrl Pts',(0.781298459660345,-0.185571501435724,
-8.98047034420009));
#60033=CARTESIAN_POINT('Ctrl Pts',(0.799824142054372,-0.0505575773245239,
-8.97517481136864));
#60034=CARTESIAN_POINT('Ctrl Pts',(0.786389927968675,0.0808438776355248,
-8.96987927853717));
#60035=CARTESIAN_POINT('Ctrl Pts',(0.772955713882977,0.212245332595581,
-8.96458374570571));
#60036=CARTESIAN_POINT('Ctrl Pts',(0.727561603317545,0.340034318404495,
-8.95928821287423));
#60037=CARTESIAN_POINT('Ctrl Pts',(0.65313927536984,0.447915528897771,-8.95399268004277));
#60038=CARTESIAN_POINT('Ctrl Pts',(0.504294619474436,0.663677949884313,
-8.94340161437983));
#60039=CARTESIAN_POINT('Ctrl Pts',(0.239337094049943,0.799809269608347,
-8.93281054871691));
#60040=CARTESIAN_POINT('Ctrl Pts',(-0.0224489462895803,0.792333768612198,
-8.92221948305399));
#60041=CARTESIAN_POINT('Ctrl Pts',(-0.284234986629107,0.78485826761605,
-8.91162841739106));
#60042=CARTESIAN_POINT('Ctrl Pts',(-0.54284954188366,0.633775945899715,
-8.90103735172813));
#60043=CARTESIAN_POINT('Ctrl Pts',(-0.678338600276407,0.409766724754542,
-8.8904462860652));
#60044=CARTESIAN_POINT('Ctrl Pts',(-0.752166247916911,0.287704662746626,
-8.88467524098468));
#60045=CARTESIAN_POINT('Ctrl Pts',(-0.789436301294637,0.14398963633968,
-8.87890419590418));
#60046=CARTESIAN_POINT('Ctrl Pts',(-0.789536508750431,0.000222284108289859,
-8.87313315082367));
#60047=CARTESIAN_POINT('Origin',(0.,0.,-5.925));
#60048=CARTESIAN_POINT('',(-0.7911,-5.56776846849516E-14,-8.64466684917629));
#60049=CARTESIAN_POINT('',(-0.7911,-6.11399819661074E-13,-8.67313315082367));
#60050=CARTESIAN_POINT('',(-0.7911,-9.68818082805471E-17,-5.925));
#60051=CARTESIAN_POINT('Ctrl Pts',(-0.7911,-7.82152120848423E-14,-8.64466684917629));
#60052=CARTESIAN_POINT('Ctrl Pts',(-0.791100000000022,0.220167589666598,
-8.65352559274957));
#60053=CARTESIAN_POINT('Ctrl Pts',(-0.694214576672415,0.438610418338613,
-8.66238433632284));
#60054=CARTESIAN_POINT('Ctrl Pts',(-0.531017389080388,0.586395551223103,
-8.67124307989611));
#60055=CARTESIAN_POINT('Ctrl Pts',(-0.367820201488361,0.734180684107594,
-8.68010182346938));
#60056=CARTESIAN_POINT('Ctrl Pts',(-0.140868175871828,0.808992666571322,
-8.68896056704266));
#60057=CARTESIAN_POINT('Ctrl Pts',(0.0782205473246826,0.787223447298305,
-8.69781931061593));
#60058=CARTESIAN_POINT('Ctrl Pts',(0.297309270521193,0.765454228025288,
-8.7066780541892));
#60059=CARTESIAN_POINT('Ctrl Pts',(0.505102072675533,0.647444880834279,
-8.71553679776247));
#60060=CARTESIAN_POINT('Ctrl Pts',(0.636026795761686,0.470435038101035,
-8.72439554133575));
#60061=CARTESIAN_POINT('Ctrl Pts',(0.766951518847839,0.293425195367791,
-8.73325428490902));
#60062=CARTESIAN_POINT('Ctrl Pts',(0.818956872247065,0.0601881960100074,
-8.74211302848229));
#60063=CARTESIAN_POINT('Ctrl Pts',(0.775631781004225,-0.15567450111118,
-8.75097177205556));
#60064=CARTESIAN_POINT('Ctrl Pts',(0.732306689761385,-0.371537198232367,
-8.75983051562884));
#60065=CARTESIAN_POINT('Ctrl Pts',(0.594329958850266,-0.566643518936443,
-8.76868925920211));
#60066=CARTESIAN_POINT('Ctrl Pts',(0.405242230244103,-0.679424716084707,
-8.77754800277538));
#60067=CARTESIAN_POINT('Ctrl Pts',(0.21615450163794,-0.792205913232972,
-8.78640674634865));
#60068=CARTESIAN_POINT('Ctrl Pts',(-0.02108165292994,-0.820894963713005,
-8.79526548992193));
#60069=CARTESIAN_POINT('Ctrl Pts',(-0.231602780753147,-0.756438604215444,
-8.8041242334952));
#60070=CARTESIAN_POINT('Ctrl Pts',(-0.442123908576354,-0.691982244717884,
-8.81298297706847));
#60071=CARTESIAN_POINT('Ctrl Pts',(-0.622631625634123,-0.535390358803596,
-8.82184172064174));
#60072=CARTESIAN_POINT('Ctrl Pts',(-0.716163994722122,-0.336077881842368,
-8.83070046421502));
#60073=CARTESIAN_POINT('Ctrl Pts',(-0.765317280859468,-0.231334857514595,
-8.83535592586878));
#60074=CARTESIAN_POINT('Ctrl Pts',(-0.791099999999994,-0.115702837836577,
-8.84001138752253));
#60075=CARTESIAN_POINT('Ctrl Pts',(-0.7911,-3.90243393155743E-14,-8.84466684917629));
#60076=CARTESIAN_POINT('Ctrl Pts',(-0.7911,-6.05904215689179E-13,-8.87313315082367));
#60077=CARTESIAN_POINT('Ctrl Pts',(-0.791099999999831,-0.220167589667286,
-8.8642744072504));
#60078=CARTESIAN_POINT('Ctrl Pts',(-0.694214576672033,-0.438610418339221,
-8.85541566367713));
#60079=CARTESIAN_POINT('Ctrl Pts',(-0.531017389079873,-0.58639555122357,
-8.84655692010385));
#60080=CARTESIAN_POINT('Ctrl Pts',(-0.367820201487713,-0.73418068410792,
-8.83769817653058));
#60081=CARTESIAN_POINT('Ctrl Pts',(-0.140868175871109,-0.808992666571448,
-8.82883943295731));
#60082=CARTESIAN_POINT('Ctrl Pts',(0.0782205473253857,-0.787223447298235,
-8.81998068938404));
#60083=CARTESIAN_POINT('Ctrl Pts',(0.29730927052188,-0.765454228025022,
-8.81112194581076));
#60084=CARTESIAN_POINT('Ctrl Pts',(0.505102072676118,-0.647444880833824,
-8.80226320223749));
#60085=CARTESIAN_POINT('Ctrl Pts',(0.636026795762113,-0.470435038100458,
-8.79340445866422));
#60086=CARTESIAN_POINT('Ctrl Pts',(0.766951518848108,-0.293425195367092,
-8.78454571509094));
#60087=CARTESIAN_POINT('Ctrl Pts',(0.818956872247121,-0.0601881960092564,
-8.77568697151767));
#60088=CARTESIAN_POINT('Ctrl Pts',(0.775631781004081,0.155674501111895,
-8.7668282279444));
#60089=CARTESIAN_POINT('Ctrl Pts',(0.732306689761042,0.371537198233045,
-8.75796948437113));
#60090=CARTESIAN_POINT('Ctrl Pts',(0.594329958849739,0.566643518936997,
-8.74911074079785));
#60091=CARTESIAN_POINT('Ctrl Pts',(0.405242230243467,0.679424716085087,
-8.74025199722458));
#60092=CARTESIAN_POINT('Ctrl Pts',(0.216154501637195,0.792205913233177,
-8.73139325365131));
#60093=CARTESIAN_POINT('Ctrl Pts',(-0.0210816529307163,0.820894963712986,
-8.72253451007803));
#60094=CARTESIAN_POINT('Ctrl Pts',(-0.231602780753866,0.756438604215224,
-8.71367576650476));
#60095=CARTESIAN_POINT('Ctrl Pts',(-0.442123908577015,0.691982244717463,
-8.70481702293149));
#60096=CARTESIAN_POINT('Ctrl Pts',(-0.622631625634637,0.535390358802999,
-8.69595827935822));
#60097=CARTESIAN_POINT('Ctrl Pts',(-0.716163994722446,0.336077881841678,
-8.68709953578495));
#60098=CARTESIAN_POINT('Ctrl Pts',(-0.765317280859677,0.231334857513888,
-8.68244407413119));
#60099=CARTESIAN_POINT('Ctrl Pts',(-0.791100000000091,0.115702837835882,
-8.67778861247743));
#60100=CARTESIAN_POINT('Ctrl Pts',(-0.7911,-6.22557561058557E-13,-8.67313315082367));
#60101=CARTESIAN_POINT('Origin',(0.,0.,-5.925));
#60102=CARTESIAN_POINT('',(-0.7911,-6.11177775056149E-14,-8.44466684917629));
#60103=CARTESIAN_POINT('',(-0.791450958846291,0.000332134113033131,-8.47313315082367));
#60104=CARTESIAN_POINT('',(-0.7911,-9.68818082805471E-17,-5.925));
#60105=CARTESIAN_POINT('Ctrl Pts',(-0.7911,-6.11177775056149E-14,-8.44466684917629));
#60106=CARTESIAN_POINT('Ctrl Pts',(-0.791100000000017,0.220167589666615,
-8.45352559274957));
#60107=CARTESIAN_POINT('Ctrl Pts',(-0.694214576672406,0.438610418338628,
-8.46238433632284));
#60108=CARTESIAN_POINT('Ctrl Pts',(-0.531017389080376,0.586395551223115,
-8.47124307989611));
#60109=CARTESIAN_POINT('Ctrl Pts',(-0.367820201488346,0.734180684107602,
-8.48010182346938));
#60110=CARTESIAN_POINT('Ctrl Pts',(-0.14086817587181,0.808992666571325,
-8.48896056704266));
#60111=CARTESIAN_POINT('Ctrl Pts',(0.0782205473246995,0.787223447298303,
-8.49781931061593));
#60112=CARTESIAN_POINT('Ctrl Pts',(0.297309270521209,0.765454228025282,
-8.5066780541892));
#60113=CARTESIAN_POINT('Ctrl Pts',(0.505102072675547,0.647444880834269,
-8.51553679776247));
#60114=CARTESIAN_POINT('Ctrl Pts',(0.636026795761696,0.470435038101021,
-8.52439554133575));
#60115=CARTESIAN_POINT('Ctrl Pts',(0.766951518847846,0.293425195367774,
-8.53325428490902));
#60116=CARTESIAN_POINT('Ctrl Pts',(0.818956872247066,0.0601881960099898,
-8.54211302848229));
#60117=CARTESIAN_POINT('Ctrl Pts',(0.775631781004221,-0.155674501111196,
-8.55097177205556));
#60118=CARTESIAN_POINT('Ctrl Pts',(0.732306689761376,-0.371537198232383,
-8.55983051562884));
#60119=CARTESIAN_POINT('Ctrl Pts',(0.594329958850254,-0.566643518936455,
-8.56868925920211));
#60120=CARTESIAN_POINT('Ctrl Pts',(0.405242230244088,-0.679424716084716,
-8.57754800277538));
#60121=CARTESIAN_POINT('Ctrl Pts',(0.216154501637923,-0.792205913232977,
-8.58640674634865));
#60122=CARTESIAN_POINT('Ctrl Pts',(-0.0210816529299578,-0.820894963713004,
-8.59526548992193));
#60123=CARTESIAN_POINT('Ctrl Pts',(-0.231602780753163,-0.756438604215439,
-8.6041242334952));
#60124=CARTESIAN_POINT('Ctrl Pts',(-0.442123908576369,-0.691982244717875,
-8.61298297706847));
#60125=CARTESIAN_POINT('Ctrl Pts',(-0.622631625634134,-0.535390358803583,
-8.62184172064175));
#60126=CARTESIAN_POINT('Ctrl Pts',(-0.716163994722129,-0.336077881842353,
-8.63070046421502));
#60127=CARTESIAN_POINT('Ctrl Pts',(-0.765317280859465,-0.231334857514596,
-8.63535592586878));
#60128=CARTESIAN_POINT('Ctrl Pts',(-0.791099999999989,-0.115702837836598,
-8.64001138752253));
#60129=CARTESIAN_POINT('Ctrl Pts',(-0.7911,-7.82152120848423E-14,-8.64466684917629));
#60130=CARTESIAN_POINT('Ctrl Pts',(-0.7911,-6.22557561058557E-13,-8.67313315082367));
#60131=CARTESIAN_POINT('Ctrl Pts',(-0.791099999999827,-0.220167589667295,
-8.6642744072504));
#60132=CARTESIAN_POINT('Ctrl Pts',(-0.69421457667203,-0.438610418339221,
-8.65541566367713));
#60133=CARTESIAN_POINT('Ctrl Pts',(-0.531017389079877,-0.586395551223566,
-8.64655692010385));
#60134=CARTESIAN_POINT('Ctrl Pts',(-0.367820201487724,-0.734180684107912,
-8.63769817653058));
#60135=CARTESIAN_POINT('Ctrl Pts',(-0.14086817587113,-0.808992666571442,
-8.62883943295731));
#60136=CARTESIAN_POINT('Ctrl Pts',(0.0782205473253575,-0.787223447298238,
-8.61998068938404));
#60137=CARTESIAN_POINT('Ctrl Pts',(0.297309270521845,-0.765454228025034,
-8.61112194581076));
#60138=CARTESIAN_POINT('Ctrl Pts',(0.505102072676081,-0.647444880833851,
-8.60226320223749));
#60139=CARTESIAN_POINT('Ctrl Pts',(0.636026795762083,-0.470435038100499,
-8.59340445866422));
#60140=CARTESIAN_POINT('Ctrl Pts',(0.766951518848085,-0.293425195367147,
-8.58454571509095));
#60141=CARTESIAN_POINT('Ctrl Pts',(0.818956872247114,-0.0601881960093249,
-8.57568697151767));
#60142=CARTESIAN_POINT('Ctrl Pts',(0.775631781004096,0.155674501111823,
-8.5668282279444));
#60143=CARTESIAN_POINT('Ctrl Pts',(0.732306689761077,0.37153719823297,-8.55796948437113));
#60144=CARTESIAN_POINT('Ctrl Pts',(0.594329958849801,0.566643518936929,
-8.54911074079786));
#60145=CARTESIAN_POINT('Ctrl Pts',(0.40524223024355,0.679424716085038,-8.54025199722458));
#60146=CARTESIAN_POINT('Ctrl Pts',(0.216154501637298,0.792205913233147,
-8.53139325365131));
#60147=CARTESIAN_POINT('Ctrl Pts',(-0.0210816529306007,0.820894963712987,
-8.52253451007804));
#60148=CARTESIAN_POINT('Ctrl Pts',(-0.231602780753753,0.756438604215259,
-8.51367576650477));
#60149=CARTESIAN_POINT('Ctrl Pts',(-0.442123908576904,0.691982244717531,
-8.5048170229315));
#60150=CARTESIAN_POINT('Ctrl Pts',(-0.622631625634545,0.535390358803103,
-8.49595827935822));
#60151=CARTESIAN_POINT('Ctrl Pts',(-0.716163994722386,0.336077881841805,
-8.48709953578495));
#60152=CARTESIAN_POINT('Ctrl Pts',(-0.765317280859654,0.231334857513987,
-8.48244407413119));
#60153=CARTESIAN_POINT('Ctrl Pts',(-0.791100000000089,0.11570283783594,
-8.47778861247743));
#60154=CARTESIAN_POINT('Ctrl Pts',(-0.7911,-6.0551563763056E-13,-8.47313315082367));
#60155=CARTESIAN_POINT('Origin',(0.,0.,-5.925));
#60156=CARTESIAN_POINT('',(-0.7911,-6.65578703262781E-14,-8.24466684917629));
#60157=CARTESIAN_POINT('',(-0.789508070680606,0.000139428570836753,-8.27313315082367));
#60158=CARTESIAN_POINT('',(-0.7911,-9.68818082805471E-17,-5.925));
#60159=CARTESIAN_POINT('Ctrl Pts',(-0.7911,-4.40758540776187E-14,-8.24466684917629));
#60160=CARTESIAN_POINT('Ctrl Pts',(-0.791100000000012,0.220167589666636,
-8.25352559274957));
#60161=CARTESIAN_POINT('Ctrl Pts',(-0.694214576672393,0.43861041833865,
-8.26238433632284));
#60162=CARTESIAN_POINT('Ctrl Pts',(-0.531017389080355,0.586395551223134,
-8.27124307989611));
#60163=CARTESIAN_POINT('Ctrl Pts',(-0.367820201488317,0.734180684107618,
-8.28010182346939));
#60164=CARTESIAN_POINT('Ctrl Pts',(-0.140868175871773,0.808992666571332,
-8.28896056704266));
#60165=CARTESIAN_POINT('Ctrl Pts',(0.0782205473247389,0.787223447298299,
-8.29781931061593));
#60166=CARTESIAN_POINT('Ctrl Pts',(0.297309270521251,0.765454228025267,
-8.3066780541892));
#60167=CARTESIAN_POINT('Ctrl Pts',(0.505102072675586,0.647444880834239,
-8.31553679776248));
#60168=CARTESIAN_POINT('Ctrl Pts',(0.636026795761727,0.47043503810098,-8.32439554133575));
#60169=CARTESIAN_POINT('Ctrl Pts',(0.766951518847867,0.293425195367722,
-8.33325428490902));
#60170=CARTESIAN_POINT('Ctrl Pts',(0.818956872247071,0.0601881960099293,
-8.34211302848229));
#60171=CARTESIAN_POINT('Ctrl Pts',(0.775631781004209,-0.155674501111257,
-8.35097177205557));
#60172=CARTESIAN_POINT('Ctrl Pts',(0.732306689761347,-0.371537198232444,
-8.35983051562884));
#60173=CARTESIAN_POINT('Ctrl Pts',(0.594329958850205,-0.566643518936508,
-8.36868925920211));
#60174=CARTESIAN_POINT('Ctrl Pts',(0.405242230244025,-0.679424716084754,
-8.37754800277538));
#60175=CARTESIAN_POINT('Ctrl Pts',(0.216154501637846,-0.792205913232999,
-8.38640674634866));
#60176=CARTESIAN_POINT('Ctrl Pts',(-0.0210816529300418,-0.820894963713003,
-8.39526548992193));
#60177=CARTESIAN_POINT('Ctrl Pts',(-0.231602780753244,-0.756438604215415,
-8.4041242334952));
#60178=CARTESIAN_POINT('Ctrl Pts',(-0.442123908576446,-0.691982244717826,
-8.41298297706848));
#60179=CARTESIAN_POINT('Ctrl Pts',(-0.622631625634197,-0.535390358803511,
-8.42184172064175));
#60180=CARTESIAN_POINT('Ctrl Pts',(-0.71616399472217,-0.336077881842266,
-8.43070046421502));
#60181=CARTESIAN_POINT('Ctrl Pts',(-0.765317280859482,-0.231334857514527,
-8.43535592586878));
#60182=CARTESIAN_POINT('Ctrl Pts',(-0.791099999999991,-0.115702837836555,
-8.44001138752254));
#60183=CARTESIAN_POINT('Ctrl Pts',(-0.7911,-6.11177775056149E-14,-8.44466684917629));
#60184=CARTESIAN_POINT('Ctrl Pts',(-0.792046526175884,0.000895756401040832,
-8.47313315082367));
#60185=CARTESIAN_POINT('Ctrl Pts',(-0.79009966938662,-0.226486983166913,
-8.46396260995651));
#60186=CARTESIAN_POINT('Ctrl Pts',(-0.686581284676827,-0.455897606404604,
-8.45479206908934));
#60187=CARTESIAN_POINT('Ctrl Pts',(-0.514165232817067,-0.60306395904845,
-8.44562152822217));
#60188=CARTESIAN_POINT('Ctrl Pts',(-0.315041783825346,-0.773026508346413,
-8.43503046255924));
#60189=CARTESIAN_POINT('Ctrl Pts',(-0.0240228999910702,-0.833291976129561,
-8.42443939689631));
#60190=CARTESIAN_POINT('Ctrl Pts',(0.227752151920718,-0.758514331340251,
-8.41384833123338));
#60191=CARTESIAN_POINT('Ctrl Pts',(0.35363967787661,-0.721125508945596,
-8.40855279840192));
#60192=CARTESIAN_POINT('Ctrl Pts',(0.46971624585188,-0.649975908407827,
-8.40325726557046));
#60193=CARTESIAN_POINT('Ctrl Pts',(0.562287117707967,-0.55603470216158,
-8.397961732739));
#60194=CARTESIAN_POINT('Ctrl Pts',(0.654857989564054,-0.462093495915333,
-8.39266619990753));
#60195=CARTESIAN_POINT('Ctrl Pts',(0.723923165300961,-0.345360683960607,
-8.38737066707606));
#60196=CARTESIAN_POINT('Ctrl Pts',(0.760326468312458,-0.219339720876201,
-8.38207513424459));
#60197=CARTESIAN_POINT('Ctrl Pts',(0.796729771323954,-0.0933187577917998,
-8.37677960141313));
#60198=CARTESIAN_POINT('Ctrl Pts',(0.800471201610043,0.041990356422283,
-8.37148406858167));
#60199=CARTESIAN_POINT('Ctrl Pts',(0.772117869221663,0.170847148582369,
-8.3661885357502));
#60200=CARTESIAN_POINT('Ctrl Pts',(0.743764536833282,0.299703940742463,
-8.36089300291874));
#60201=CARTESIAN_POINT('Ctrl Pts',(0.683316441770433,0.422108410848553,
-8.35559747008728));
#60202=CARTESIAN_POINT('Ctrl Pts',(0.596716058659417,0.520851492288747,
-8.35030193725581));
#60203=CARTESIAN_POINT('Ctrl Pts',(0.423515292437392,0.718337655169128,
-8.33971087159288));
#60204=CARTESIAN_POINT('Ctrl Pts',(0.145705374022713,0.821178263385903,
-8.32911980592995));
#60205=CARTESIAN_POINT('Ctrl Pts',(-0.113892328640817,0.783836609160277,
-8.31852874026702));
#60206=CARTESIAN_POINT('Ctrl Pts',(-0.243691179972587,0.765165782047463,
-8.31323320743556));
#60207=CARTESIAN_POINT('Ctrl Pts',(-0.368936977366574,0.711449389324045,
-8.3079376746041));
#60208=CARTESIAN_POINT('Ctrl Pts',(-0.474613758660987,0.632207743903391,
-8.30264214177263));
#60209=CARTESIAN_POINT('Ctrl Pts',(-0.580290539955397,0.55296609848274,
-8.29734660894117));
#60210=CARTESIAN_POINT('Ctrl Pts',(-0.666398305150239,0.448199200364853,
-8.2920510761097));
#60211=CARTESIAN_POINT('Ctrl Pts',(-0.72048428825659,0.328818528118176,
-8.28675554327824));
#60212=CARTESIAN_POINT('Ctrl Pts',(-0.766861773558151,0.226452350147002,
-8.28221474579338));
#60213=CARTESIAN_POINT('Ctrl Pts',(-0.789694706689629,0.113341149727473,
-8.27767394830853));
#60214=CARTESIAN_POINT('Ctrl Pts',(-0.789508070680606,0.000139428570836753,
-8.27313315082367));
#60215=CARTESIAN_POINT('Origin',(0.,0.,-5.925));
#60216=CARTESIAN_POINT('',(-0.790047180336124,-0.000229621036622829,-8.04466684917629));
#60217=CARTESIAN_POINT('',(-0.791166926155794,-0.000598937135766913,-8.07313315082367));
#60218=CARTESIAN_POINT('',(-0.7911,-9.68818082805471E-17,-5.925));
#60219=CARTESIAN_POINT('Ctrl Pts',(-0.790047180336124,-0.000229621036622829,
-8.04466684917629));
#60220=CARTESIAN_POINT('Ctrl Pts',(-0.788717572232258,0.183736650574578,
-8.05205977984234));
#60221=CARTESIAN_POINT('Ctrl Pts',(-0.725318385967807,0.368133308188168,
-8.05945271050839));
#60222=CARTESIAN_POINT('Ctrl Pts',(-0.608036083416137,0.508275660055627,
-8.06684564117444));
#60223=CARTESIAN_POINT('Ctrl Pts',(-0.440018199367973,0.70904270601237,
-8.07743670683737));
#60224=CARTESIAN_POINT('Ctrl Pts',(-0.161414669232722,0.818985550804046,
-8.0880277725003));
#60225=CARTESIAN_POINT('Ctrl Pts',(0.0984571409497746,0.786513157848435,
-8.09861883816323));
#60226=CARTESIAN_POINT('Ctrl Pts',(0.358328951132271,0.754040764892825,
-8.10920990382615));
#60227=CARTESIAN_POINT('Ctrl Pts',(0.599469041362017,0.579153134189927,
-8.11980096948908));
#60228=CARTESIAN_POINT('Ctrl Pts',(0.713725172026125,0.343242789982087,
-8.13039203515201));
#60229=CARTESIAN_POINT('Ctrl Pts',(0.770853237358178,0.225287617878169,
-8.13568756798348));
#60230=CARTESIAN_POINT('Ctrl Pts',(0.796260312798822,0.0920767673980271,
-8.14098310081494));
#60231=CARTESIAN_POINT('Ctrl Pts',(0.7895301003907,-0.0398380714741007,
-8.14627863364641));
#60232=CARTESIAN_POINT('Ctrl Pts',(0.782799887982578,-0.17175291034624,
-8.15157416647787));
#60233=CARTESIAN_POINT('Ctrl Pts',(0.74393238772568,-0.302371737610357,
-8.15686969930934));
#60234=CARTESIAN_POINT('Ctrl Pts',(0.675220556067583,-0.414063392546229,
-8.1621652321408));
#60235=CARTESIAN_POINT('Ctrl Pts',(0.537796892751397,-0.637446702417962,
-8.17275629780373));
#60236=CARTESIAN_POINT('Ctrl Pts',(0.28099590383042,-0.785121322976735,
-8.18334736346666));
#60237=CARTESIAN_POINT('Ctrl Pts',(0.0184047961489411,-0.791844426109169,
-8.19393842912959));
#60238=CARTESIAN_POINT('Ctrl Pts',(-0.112890757691798,-0.795205977675386,
-8.19923396196105));
#60239=CARTESIAN_POINT('Ctrl Pts',(-0.245633841222665,-0.763329649885019,
-8.20452949479251));
#60240=CARTESIAN_POINT('Ctrl Pts',(-0.362797491579033,-0.70266117884375,
-8.20982502762398));
#60241=CARTESIAN_POINT('Ctrl Pts',(-0.479961141935401,-0.641992707802481,
-8.21512056045545));
#60242=CARTESIAN_POINT('Ctrl Pts',(-0.581545359117274,-0.55253209351031,
-8.22041609328692));
#60243=CARTESIAN_POINT('Ctrl Pts',(-0.655091465745599,-0.443916009035298,
-8.22571162611838));
#60244=CARTESIAN_POINT('Ctrl Pts',(-0.728637572373925,-0.335299924560287,
-8.23100715894985));
#60245=CARTESIAN_POINT('Ctrl Pts',(-0.774145568448705,-0.207528369902432,
-8.2363026917813));
#60246=CARTESIAN_POINT('Ctrl Pts',(-0.787097833118284,-0.076278396999101,
-8.24159822461277));
#60247=CARTESIAN_POINT('Ctrl Pts',(-0.789599667449425,-0.0509264067064596,
-8.24262109946728));
#60248=CARTESIAN_POINT('Ctrl Pts',(-0.790886846250653,-0.025444636501807,
-8.24364397432178));
#60249=CARTESIAN_POINT('Ctrl Pts',(-0.790961777408698,4.04858511152684E-5,
-8.24466684917629));
#60250=CARTESIAN_POINT('Ctrl Pts',(-0.789508070680606,0.000139428570836753,
-8.27313315082367));
#60251=CARTESIAN_POINT('Ctrl Pts',(-0.78925939235702,-0.150693277248314,
-8.2670828826456));
#60252=CARTESIAN_POINT('Ctrl Pts',(-0.748142827911767,-0.301686689427919,
-8.26103261446752));
#60253=CARTESIAN_POINT('Ctrl Pts',(-0.667400237636104,-0.427637321659363,
-8.25498234628945));
#60254=CARTESIAN_POINT('Ctrl Pts',(-0.52605938294417,-0.648115385935031,
-8.24439128062652));
#60255=CARTESIAN_POINT('Ctrl Pts',(-0.263292835701562,-0.791855073477848,
-8.23380021496359));
#60256=CARTESIAN_POINT('Ctrl Pts',(-0.00149710346494951,-0.79249592050826,
-8.22320914930066));
#60257=CARTESIAN_POINT('Ctrl Pts',(0.260298628771663,-0.793136767538672,
-8.21261808363773));
#60258=CARTESIAN_POINT('Ctrl Pts',(0.521123546002274,-0.65067877405668,
-8.2020270179748));
#60259=CARTESIAN_POINT('Ctrl Pts',(0.664616688819202,-0.430696750041217,
-8.19143595231187));
#60260=CARTESIAN_POINT('Ctrl Pts',(0.736363260227663,-0.320705738033488,
-8.18614041948041));
#60261=CARTESIAN_POINT('Ctrl Pts',(0.778776888032708,-0.191333718392383,
-8.18084488664894));
#60262=CARTESIAN_POINT('Ctrl Pts',(0.788520488945965,-0.0598066155259459,
-8.17554935381748));
#60263=CARTESIAN_POINT('Ctrl Pts',(0.798264089859222,0.071720487340495,
-8.17025382098602));
#60264=CARTESIAN_POINT('Ctrl Pts',(0.775337663880695,0.205402673432278,
-8.16495828815455));
#60265=CARTESIAN_POINT('Ctrl Pts',(0.721503951327807,0.325020460569648,
-8.15966275532308));
#60266=CARTESIAN_POINT('Ctrl Pts',(0.667670238774919,0.444638247707018,
-8.15436722249162));
#60267=CARTESIAN_POINT('Ctrl Pts',(0.582929239647671,0.550191635889973,
-8.14907168966016));
#60268=CARTESIAN_POINT('Ctrl Pts',(0.477902833472298,0.630050501078506,
-8.14377615682869));
#60269=CARTESIAN_POINT('Ctrl Pts',(0.372876427296924,0.709909366267039,
-8.13848062399723));
#60270=CARTESIAN_POINT('Ctrl Pts',(0.247564614073427,0.764073708461148,
-8.13318509116576));
#60271=CARTESIAN_POINT('Ctrl Pts',(0.117637024355971,0.783273810478888,
-8.1278895583343));
#60272=CARTESIAN_POINT('Ctrl Pts',(-0.14221815507894,0.821674014514368,
-8.11729849267136));
#60273=CARTESIAN_POINT('Ctrl Pts',(-0.420536440489676,0.72021725784437,
-8.10670742700844));
#60274=CARTESIAN_POINT('Ctrl Pts',(-0.59422621506534,0.523704590119495,
-8.09611636134551));
#60275=CARTESIAN_POINT('Ctrl Pts',(-0.681071102353172,0.425448256257057,
-8.09082082851405));
#60276=CARTESIAN_POINT('Ctrl Pts',(-0.741758861932236,0.303427944630902,
-8.08552529568258));
#60277=CARTESIAN_POINT('Ctrl Pts',(-0.771007462975747,0.174620569800434,
-8.08022976285112));
#60278=CARTESIAN_POINT('Ctrl Pts',(-0.784072939139481,0.117081760232854,
-8.07786422550864));
#60279=CARTESIAN_POINT('Ctrl Pts',(-0.790864896553931,0.0581886278955768,
-8.07549868816616));
#60280=CARTESIAN_POINT('Ctrl Pts',(-0.791166926155794,-0.000598937135766913,
-8.07313315082367));
#60281=CARTESIAN_POINT('Origin',(0.,0.,-5.925));
#60282=CARTESIAN_POINT('',(-0.792491847548892,-0.000436464152781535,-7.8446668491763));
#60283=CARTESIAN_POINT('',(-0.792077464554372,0.000352317614289522,-7.87313315082367));
#60284=CARTESIAN_POINT('',(-0.7911,-9.68818082805471E-17,-5.925));
#60285=CARTESIAN_POINT('Ctrl Pts',(-0.792491847548892,-0.000436464152781535,
-7.8446668491763));
#60286=CARTESIAN_POINT('Ctrl Pts',(-0.792298347834538,0.25945640178687,
-7.85518005253144));
#60287=CARTESIAN_POINT('Ctrl Pts',(-0.651590353855427,0.520785898705083,
-7.86569325588657));
#60288=CARTESIAN_POINT('Ctrl Pts',(-0.434108069765603,0.663209574596977,
-7.87620645924171));
#60289=CARTESIAN_POINT('Ctrl Pts',(-0.21501508035881,0.806688060874836,
-7.88679752490464));
#60290=CARTESIAN_POINT('Ctrl Pts',(0.0819936133437958,0.829492936536737,
-7.89738859056758));
#60291=CARTESIAN_POINT('Ctrl Pts',(0.321795719765056,0.723648221720539,
-7.9079796562305));
#60292=CARTESIAN_POINT('Ctrl Pts',(0.441696772975692,0.670725864312437,
-7.91327518906196));
#60293=CARTESIAN_POINT('Ctrl Pts',(0.547296179365993,0.585641109284806,
-7.91857072189342));
#60294=CARTESIAN_POINT('Ctrl Pts',(0.627561863841052,0.480740011247315,
-7.92386625472489));
#60295=CARTESIAN_POINT('Ctrl Pts',(0.707827548316103,0.375838913209837,
-7.92916178755636));
#60296=CARTESIAN_POINT('Ctrl Pts',(0.762759510875919,0.251121472162503,
-7.93445732038783));
#60297=CARTESIAN_POINT('Ctrl Pts',(0.782691847255788,0.121510347799813,
-7.9397528532193));
#60298=CARTESIAN_POINT('Ctrl Pts',(0.822556520015527,-0.137711900925585,
-7.95034391888223));
#60299=CARTESIAN_POINT('Ctrl Pts',(0.72242268805546,-0.416508882912403,
-7.96093498454514));
#60300=CARTESIAN_POINT('Ctrl Pts',(0.526630374428653,-0.591622160175378,
-7.97152605020807));
#60301=CARTESIAN_POINT('Ctrl Pts',(0.428734217615251,-0.679178798806863,
-7.97682158303954));
#60302=CARTESIAN_POINT('Ctrl Pts',(0.306923440385164,-0.740814511257387,
-7.98211711587101));
#60303=CARTESIAN_POINT('Ctrl Pts',(0.178348500349687,-0.770419732725704,
-7.98741264870248));
#60304=CARTESIAN_POINT('Ctrl Pts',(0.0497735603142099,-0.800024954194021,
-7.99270818153394));
#60305=CARTESIAN_POINT('Ctrl Pts',(-0.0855655425266594,-0.797599684680131,
-7.9980037143654));
#60306=CARTESIAN_POINT('Ctrl Pts',(-0.211934595031162,-0.762423752908789,
-8.00329924719686));
#60307=CARTESIAN_POINT('Ctrl Pts',(-0.338303647535658,-0.727247821137449,
-8.00859478002833));
#60308=CARTESIAN_POINT('Ctrl Pts',(-0.455702649703791,-0.659321227108661,
-8.01389031285979));
#60309=CARTESIAN_POINT('Ctrl Pts',(-0.550539734854605,-0.567668383032269,
-8.01918584569126));
#60310=CARTESIAN_POINT('Ctrl Pts',(-0.64537682000543,-0.476015538955867,
-8.02448137852272));
#60311=CARTESIAN_POINT('Ctrl Pts',(-0.717651988138931,-0.360636444831854,
-8.02977691135419));
#60312=CARTESIAN_POINT('Ctrl Pts',(-0.756263393901083,-0.235118507562208,
-8.03507244418565));
#60313=CARTESIAN_POINT('Ctrl Pts',(-0.779582008283564,-0.159314368357715,
-8.03827057918253));
#60314=CARTESIAN_POINT('Ctrl Pts',(-0.790622360383279,-0.0798122653305001,
-8.04146871417941));
#60315=CARTESIAN_POINT('Ctrl Pts',(-0.790047180336124,-0.000229621036622829,
-8.04466684917629));
#60316=CARTESIAN_POINT('Ctrl Pts',(-0.791166926155794,-0.000598937135766913,
-8.07313315082367));
#60317=CARTESIAN_POINT('Ctrl Pts',(-0.791541025247406,-0.0734142325262931,
-8.07020315533469));
#60318=CARTESIAN_POINT('Ctrl Pts',(-0.781958453425139,-0.146067569424397,
-8.0672731598457));
#60319=CARTESIAN_POINT('Ctrl Pts',(-0.762007978713805,-0.215784787311132,
-8.06434316435672));
#60320=CARTESIAN_POINT('Ctrl Pts',(-0.689892923086983,-0.467791875803772,
-8.05375209869379));
#60321=CARTESIAN_POINT('Ctrl Pts',(-0.482309986174684,-0.681435389142571,
-8.04316103303086));
#60322=CARTESIAN_POINT('Ctrl Pts',(-0.231854275641584,-0.757984400195306,
-8.03256996736793));
#60323=CARTESIAN_POINT('Ctrl Pts',(0.0186014348915136,-0.834533411248041,
-8.021978901705));
#60324=CARTESIAN_POINT('Ctrl Pts',(0.311929919045417,-0.77398792001471,
-8.01138783604208));
#60325=CARTESIAN_POINT('Ctrl Pts',(0.511883075792864,-0.605002266159273,
-8.00079677037915));
#60326=CARTESIAN_POINT('Ctrl Pts',(0.711836232540309,-0.43601661230384,
-7.99020570471622));
#60327=CARTESIAN_POINT('Ctrl Pts',(0.818414061881308,-0.158590795826307,
-7.97961463905329));
#60328=CARTESIAN_POINT('Ctrl Pts',(0.78537732129719,0.101968116316403,-7.96902357339036));
#60329=CARTESIAN_POINT('Ctrl Pts',(0.76885895100513,0.232247572387769,-7.9637280405589));
#60330=CARTESIAN_POINT('Ctrl Pts',(0.717436938231784,0.358310302375426,
-7.95843250772743));
#60331=CARTESIAN_POINT('Ctrl Pts',(0.63971903264416,0.464866595940244,-7.95313697489597));
#60332=CARTESIAN_POINT('Ctrl Pts',(0.562001127056541,0.571422889505055,
-7.9478414420645));
#60333=CARTESIAN_POINT('Ctrl Pts',(0.45798732865465,0.658472746647027,-7.94254590923304));
#60334=CARTESIAN_POINT('Ctrl Pts',(0.3395209030078,0.714794941218329,-7.93725037640157));
#60335=CARTESIAN_POINT('Ctrl Pts',(0.221054477360954,0.771117135789629,
-7.93195484357011));
#60336=CARTESIAN_POINT('Ctrl Pts',(0.0881354244691417,0.796711667790262,
-7.92665931073864));
#60337=CARTESIAN_POINT('Ctrl Pts',(-0.0436115676640736,0.789590262931357,
-7.92136377790718));
#60338=CARTESIAN_POINT('Ctrl Pts',(-0.175358559797293,0.782468858072452,
-7.91606824507571));
#60339=CARTESIAN_POINT('Ctrl Pts',(-0.305933491171922,0.74263151635401,
-7.91077271224425));
#60340=CARTESIAN_POINT('Ctrl Pts',(-0.417392339406398,0.673156717775511,
-7.90547717941278));
#60341=CARTESIAN_POINT('Ctrl Pts',(-0.640310035875351,0.534207120618512,
-7.89488611374986));
#60342=CARTESIAN_POINT('Ctrl Pts',(-0.786763399783684,0.27670769602129,
-7.88429504808694));
#60343=CARTESIAN_POINT('Ctrl Pts',(-0.791935199270052,0.0144890489754226,
-7.873703982424));
#60344=CARTESIAN_POINT('Ctrl Pts',(-0.792028114898857,0.00977807544695631,
-7.87351370522389));
#60345=CARTESIAN_POINT('Ctrl Pts',(-0.792075428969904,0.00506557869147931,
-7.87332342802378));
#60346=CARTESIAN_POINT('Ctrl Pts',(-0.792077464554372,0.000352317614289522,
-7.87313315082367));
#60347=CARTESIAN_POINT('Origin',(0.,0.,-5.925));
#60348=CARTESIAN_POINT('',(-0.790740166226785,0.000940778128334207,-7.64466684917629));
#60349=CARTESIAN_POINT('',(-0.790714182338634,7.12898943596447E-5,-7.67313315082367));
#60350=CARTESIAN_POINT('',(-0.7911,-9.68818082805471E-17,-5.925));
#60351=CARTESIAN_POINT('Ctrl Pts',(-0.790740166226785,0.000940778128334207,
-7.64466684917629));
#60352=CARTESIAN_POINT('Ctrl Pts',(-0.791434367191261,0.0767299662908557,
-7.6477092595576));
#60353=CARTESIAN_POINT('Ctrl Pts',(-0.781492355410326,0.152314472677872,
-7.6507516699389));
#60354=CARTESIAN_POINT('Ctrl Pts',(-0.760203509104705,0.224471336293998,
-7.6537940803202));
#60355=CARTESIAN_POINT('Ctrl Pts',(-0.686093990383465,0.475659698418317,
-7.66438514598313));
#60356=CARTESIAN_POINT('Ctrl Pts',(-0.474479483182523,0.685310662716084,
-7.67497621164606));
#60357=CARTESIAN_POINT('Ctrl Pts',(-0.223185687336729,0.759873267740378,
-7.68556727730899));
#60358=CARTESIAN_POINT('Ctrl Pts',(-0.0975387894138313,0.797154570252525,
-7.69086281014045));
#60359=CARTESIAN_POINT('Ctrl Pts',(0.0380279306702764,0.800663782946304,
-7.69615834297192));
#60360=CARTESIAN_POINT('Ctrl Pts',(0.167113678227793,0.772669314720665,
-7.70145387580338));
#60361=CARTESIAN_POINT('Ctrl Pts',(0.29619942578531,0.744674846495026,-7.70674940863485));
#60362=CARTESIAN_POINT('Ctrl Pts',(0.418804200816231,0.685176697349972,
-7.71204494146632));
#60363=CARTESIAN_POINT('Ctrl Pts',(0.517900519948477,0.599291534914524,
-7.71734047429778));
#60364=CARTESIAN_POINT('Ctrl Pts',(0.716093158212969,0.427521210043628,
-7.72793153996071));
#60365=CARTESIAN_POINT('Ctrl Pts',(0.820251972882747,0.150202832011168,
-7.73852260562363));
#60366=CARTESIAN_POINT('Ctrl Pts',(0.784380873848862,-0.110013528356924,
-7.74911367128656));
#60367=CARTESIAN_POINT('Ctrl Pts',(0.766445324331919,-0.24012170854097,
-7.75440920411803));
#60368=CARTESIAN_POINT('Ctrl Pts',(0.713502296389051,-0.365954384308944,
-7.7597047369495));
#60369=CARTESIAN_POINT('Ctrl Pts',(0.634668669730602,-0.471752511188351,
-7.76500026978096));
#60370=CARTESIAN_POINT('Ctrl Pts',(0.555835043072157,-0.577550638067753,
-7.77029580261242));
#60371=CARTESIAN_POINT('Ctrl Pts',(0.451110817698131,-0.663314216058609,
-7.77559133544388));
#60372=CARTESIAN_POINT('Ctrl Pts',(0.332022261747654,-0.718308756228488,
-7.78088686827535));
#60373=CARTESIAN_POINT('Ctrl Pts',(0.21293370579717,-0.77330329639837,-7.78618240110681));
#60374=CARTESIAN_POINT('Ctrl Pts',(0.0794808192702385,-0.797528798747268,
-7.79147793393828));
#60375=CARTESIAN_POINT('Ctrl Pts',(-0.0521348267623253,-0.789064859556369,
-7.79677346676974));
#60376=CARTESIAN_POINT('Ctrl Pts',(-0.183750472794889,-0.78060092036547,
-7.80206899960121));
#60377=CARTESIAN_POINT('Ctrl Pts',(-0.31352887833308,-0.739447539634773,
-7.80736453243267));
#60378=CARTESIAN_POINT('Ctrl Pts',(-0.424212478024202,-0.668774107633984,
-7.81266006526414));
#60379=CARTESIAN_POINT('Ctrl Pts',(-0.645579677406446,-0.527427243632406,
-7.82325113092707));
#60380=CARTESIAN_POINT('Ctrl Pts',(-0.790567653400404,-0.268000174550464,
-7.83384219659));
#60381=CARTESIAN_POINT('Ctrl Pts',(-0.792472998841892,-0.00621059156258216,
-7.84443326225293));
#60382=CARTESIAN_POINT('Ctrl Pts',(-0.792487006364641,-0.00428599381809321,
-7.84451112456072));
#60383=CARTESIAN_POINT('Ctrl Pts',(-0.792493280635821,-0.00236126838574793,
-7.84458898686851));
#60384=CARTESIAN_POINT('Ctrl Pts',(-0.792491847548892,-0.000436464152781535,
-7.8446668491763));
#60385=CARTESIAN_POINT('Ctrl Pts',(-0.792077464554372,0.000352317614289522,
-7.87313315082367));
#60386=CARTESIAN_POINT('Ctrl Pts',(-0.792132080551777,-0.126107408735287,
-7.86802789519232));
#60387=CARTESIAN_POINT('Ctrl Pts',(-0.759591516535767,-0.253117356739719,
-7.86292263956095));
#60388=CARTESIAN_POINT('Ctrl Pts',(-0.70069585656924,-0.366019354609049,
-7.8578173839296));
#60389=CARTESIAN_POINT('Ctrl Pts',(-0.639605105487552,-0.483129305535492,
-7.85252185109813));
#60390=CARTESIAN_POINT('Ctrl Pts',(-0.550158094686481,-0.585060078253289,
-7.84722631826667));
#60391=CARTESIAN_POINT('Ctrl Pts',(-0.441106678461014,-0.657756894510047,
-7.84193078543521));
#60392=CARTESIAN_POINT('Ctrl Pts',(-0.223003846010083,-0.803150527023559,
-7.83133971977229));
#60393=CARTESIAN_POINT('Ctrl Pts',(0.0735166081384336,-0.831608333692926,
-7.82074865410935));
#60394=CARTESIAN_POINT('Ctrl Pts',(0.313965838386481,-0.727820175866948,
-7.81015758844642));
#60395=CARTESIAN_POINT('Ctrl Pts',(0.554415068634545,-0.624032018040962,
-7.79956652278349));
#60396=CARTESIAN_POINT('Ctrl Pts',(0.738793074982127,-0.387997895719602,
-7.78897545712056));
#60397=CARTESIAN_POINT('Ctrl Pts',(0.781802262290506,-0.129758421763161,
-7.77838439145763));
#60398=CARTESIAN_POINT('Ctrl Pts',(0.824811449598881,0.128481052193258,
-7.76779332579471));
#60399=CARTESIAN_POINT('Ctrl Pts',(0.726451817868084,0.408925877784763,
-7.75720226013178));
#60400=CARTESIAN_POINT('Ctrl Pts',(0.532598074500645,0.58613507367438,-7.74661119446885));
#60401=CARTESIAN_POINT('Ctrl Pts',(0.435671202816917,0.674739671619196,
-7.74131566163738));
#60402=CARTESIAN_POINT('Ctrl Pts',(0.314870803224043,0.737535362138529,
-7.73602012880591));
#60403=CARTESIAN_POINT('Ctrl Pts',(0.186655454501568,0.768440716030238,
-7.73072459597445));
#60404=CARTESIAN_POINT('Ctrl Pts',(0.0584401057790991,0.799346069921944,
-7.72542906314298));
#60405=CARTESIAN_POINT('Ctrl Pts',(-0.0771901920729581,0.798361087186018,
-7.72013353031152));
#60406=CARTESIAN_POINT('Ctrl Pts',(-0.203944522867036,0.764599818966159,
-7.71483799748006));
#60407=CARTESIAN_POINT('Ctrl Pts',(-0.330698853661106,0.730838550746301,
-7.7095424646486));
#60408=CARTESIAN_POINT('Ctrl Pts',(-0.448577217397205,0.664300997042512,
-7.70424693181714));
#60409=CARTESIAN_POINT('Ctrl Pts',(-0.544383506192386,0.573586393088096,
-7.69895139898567));
#60410=CARTESIAN_POINT('Ctrl Pts',(-0.640189794987579,0.482871789133669,
-7.6936558661542));
#60411=CARTESIAN_POINT('Ctrl Pts',(-0.713924008841854,0.367980134928604,
-7.68836033332273));
#60412=CARTESIAN_POINT('Ctrl Pts',(-0.753902240174265,0.242873926022679,
-7.68306480049127));
#60413=CARTESIAN_POINT('Ctrl Pts',(-0.778894990388472,0.164662656408623,
-7.67975425060207));
#60414=CARTESIAN_POINT('Ctrl Pts',(-0.79069510103305,0.0824592962534152,
-7.67644370071287));
#60415=CARTESIAN_POINT('Ctrl Pts',(-0.790044269977258,0.000195073709034593,
-7.67313315082367));
#60416=CARTESIAN_POINT('Origin',(0.,0.,-5.925));
#60417=CARTESIAN_POINT('',(-0.789800442128824,-0.000456880331022314,-7.44466684917629));
#60418=CARTESIAN_POINT('',(-0.7911,-6.10178574333986E-13,-7.47313315082367));
#60419=CARTESIAN_POINT('',(-0.7911,-9.68818082805471E-17,-5.925));
#60420=CARTESIAN_POINT('Ctrl Pts',(-0.789800442128824,-0.000456880331022313,
-7.44466684917629));
#60421=CARTESIAN_POINT('Ctrl Pts',(-0.788892940225841,0.153073306983262,
-7.45082953224669));
#60422=CARTESIAN_POINT('Ctrl Pts',(-0.745378609669688,0.306963099682475,
-7.45699221531708));
#60423=CARTESIAN_POINT('Ctrl Pts',(-0.662015882221351,0.434688630798064,
-7.46315489838748));
#60424=CARTESIAN_POINT('Ctrl Pts',(-0.590383112033339,0.544441920998588,
-7.46845043121894));
#60425=CARTESIAN_POINT('Ctrl Pts',(-0.489327100322849,0.634876055401825,
-7.4737459640504));
#60426=CARTESIAN_POINT('Ctrl Pts',(-0.372816842178655,0.697102900259108,
-7.47904149688187));
#60427=CARTESIAN_POINT('Ctrl Pts',(-0.256306584034461,0.759329745116391,
-7.48433702971333));
#60428=CARTESIAN_POINT('Ctrl Pts',(-0.124342079456564,0.793349300427721,
-7.4896325625448));
#60429=CARTESIAN_POINT('Ctrl Pts',(0.0067861929163434,0.792038660652882,
-7.49492809537627));
#60430=CARTESIAN_POINT('Ctrl Pts',(0.269042737662159,0.789417381103205,
-7.5055191610392));
#60431=CARTESIAN_POINT('Ctrl Pts',(0.527954353588018,0.645475321208852,
-7.51611022670212));
#60432=CARTESIAN_POINT('Ctrl Pts',(0.669065422703021,0.423919558200222,
-7.52670129236505));
#60433=CARTESIAN_POINT('Ctrl Pts',(0.739620957260523,0.313141676695907,
-7.53199682519651));
#60434=CARTESIAN_POINT('Ctrl Pts',(0.78072635511531,0.182960369413022,-7.53729235802798));
#60435=CARTESIAN_POINT('Ctrl Pts',(0.789128762633997,0.0512888694929381,
-7.54258789085944));
#60436=CARTESIAN_POINT('Ctrl Pts',(0.797531170152684,-0.0803826304271457,
-7.54788342369091));
#60437=CARTESIAN_POINT('Ctrl Pts',(0.77323058733527,-0.213544322984428,
-7.55317895652238));
#60438=CARTESIAN_POINT('Ctrl Pts',(0.718063232484806,-0.33255292168919,
-7.55847448935384));
#60439=CARTESIAN_POINT('Ctrl Pts',(0.662895877634341,-0.451561520393951,
-7.5637700221853));
#60440=CARTESIAN_POINT('Ctrl Pts',(0.576861750750826,-0.556417025246192,
-7.56906555501677));
#60441=CARTESIAN_POINT('Ctrl Pts',(0.471066362514449,-0.635167595879746,
-7.57436108784823));
#60442=CARTESIAN_POINT('Ctrl Pts',(0.365270974278072,-0.7139181665133,-7.5796566206797));
#60443=CARTESIAN_POINT('Ctrl Pts',(0.239714324688833,-0.766563802928168,
-7.58495215351116));
#60444=CARTESIAN_POINT('Ctrl Pts',(0.109601684041382,-0.784348458536356,
-7.59024768634263));
#60445=CARTESIAN_POINT('Ctrl Pts',(-0.15062359725352,-0.819917769752734,
-7.60083875200556));
#60446=CARTESIAN_POINT('Ctrl Pts',(-0.42907284278127,-0.716043157742395,
-7.61142981766848));
#60447=CARTESIAN_POINT('Ctrl Pts',(-0.599995200424376,-0.517742971761791,
-7.62202088333141));
#60448=CARTESIAN_POINT('Ctrl Pts',(-0.721818064981508,-0.376406887755678,
-7.62956953861304));
#60449=CARTESIAN_POINT('Ctrl Pts',(-0.789017754349279,-0.187103037074619,
-7.63711819389467));
#60450=CARTESIAN_POINT('Ctrl Pts',(-0.790740166226785,0.000940778128334207,
-7.64466684917629));
#60451=CARTESIAN_POINT('Ctrl Pts',(-0.7911,-6.27220497761982E-13,-7.67313315082367));
#60452=CARTESIAN_POINT('Ctrl Pts',(-0.791099999999826,-0.220167589667307,
-7.6642744072504));
#60453=CARTESIAN_POINT('Ctrl Pts',(-0.694214576672021,-0.438610418339239,
-7.65541566367712));
#60454=CARTESIAN_POINT('Ctrl Pts',(-0.531017389079857,-0.586395551223585,
-7.64655692010385));
#60455=CARTESIAN_POINT('Ctrl Pts',(-0.367820201487694,-0.73418068410793,
-7.63769817653058));
#60456=CARTESIAN_POINT('Ctrl Pts',(-0.140868175871087,-0.808992666571452,
-7.62883943295731));
#60457=CARTESIAN_POINT('Ctrl Pts',(0.0782205473254069,-0.787223447298233,
-7.61998068938403));
#60458=CARTESIAN_POINT('Ctrl Pts',(0.297309270521901,-0.765454228025015,
-7.61112194581076));
#60459=CARTESIAN_POINT('Ctrl Pts',(0.505102072676136,-0.647444880833811,
-7.60226320223749));
#60460=CARTESIAN_POINT('Ctrl Pts',(0.636026795762126,-0.470435038100441,
-7.59340445866422));
#60461=CARTESIAN_POINT('Ctrl Pts',(0.766951518848116,-0.293425195367071,
-7.58454571509094));
#60462=CARTESIAN_POINT('Ctrl Pts',(0.818956872247122,-0.0601881960092344,
-7.57568697151767));
#60463=CARTESIAN_POINT('Ctrl Pts',(0.775631781004077,0.155674501111915,
-7.5668282279444));
#60464=CARTESIAN_POINT('Ctrl Pts',(0.732306689761032,0.371537198233065,
-7.55796948437113));
#60465=CARTESIAN_POINT('Ctrl Pts',(0.594329958849724,0.566643518937013,
-7.54911074079785));
#60466=CARTESIAN_POINT('Ctrl Pts',(0.405242230243449,0.679424716085098,
-7.54025199722458));
#60467=CARTESIAN_POINT('Ctrl Pts',(0.216154501637174,0.792205913233182,
-7.53139325365131));
#60468=CARTESIAN_POINT('Ctrl Pts',(-0.0210816529307384,0.820894963712985,
-7.52253451007803));
#60469=CARTESIAN_POINT('Ctrl Pts',(-0.231602780753886,0.756438604215218,
-7.51367576650476));
#60470=CARTESIAN_POINT('Ctrl Pts',(-0.442123908577034,0.691982244717451,
-7.50481702293149));
#60471=CARTESIAN_POINT('Ctrl Pts',(-0.622631625634652,0.535390358802983,
-7.49595827935822));
#60472=CARTESIAN_POINT('Ctrl Pts',(-0.716163994722455,0.336077881841658,
-7.48709953578494));
#60473=CARTESIAN_POINT('Ctrl Pts',(-0.765317280859679,0.231334857513877,
-7.48244407413119));
#60474=CARTESIAN_POINT('Ctrl Pts',(-0.791100000000089,0.115702837835883,
-7.47778861247743));
#60475=CARTESIAN_POINT('Ctrl Pts',(-0.7911,-6.10178574333986E-13,-7.47313315082367));
#60476=CARTESIAN_POINT('Origin',(0.,0.,-5.925));
#60477=CARTESIAN_POINT('',(-0.791849645310631,-0.000332508792182717,-7.2446668491763));
#60478=CARTESIAN_POINT('',(-0.79118714610156,-0.000297183305454875,-7.27313315082367));
#60479=CARTESIAN_POINT('',(-0.7911,-9.68818082805471E-17,-5.925));
#60480=CARTESIAN_POINT('Ctrl Pts',(-0.791849645310631,-0.000332508792182717,
-7.2446668491763));
#60481=CARTESIAN_POINT('Ctrl Pts',(-0.791466899765427,0.0984544020189313,
-7.24865427210432));
#60482=CARTESIAN_POINT('Ctrl Pts',(-0.771963610279708,0.197476669386961,
-7.25264169503234));
#60483=CARTESIAN_POINT('Ctrl Pts',(-0.735428824803906,0.289981542532058,
-7.25662911796036));
#60484=CARTESIAN_POINT('Ctrl Pts',(-0.686908474825973,0.412833470118636,
-7.26192465079182));
#60485=CARTESIAN_POINT('Ctrl Pts',(-0.608348982910782,0.524190404532698,
-7.26722018362329));
#60486=CARTESIAN_POINT('Ctrl Pts',(-0.507555772110868,0.608077651768299,
-7.27251571645475));
#60487=CARTESIAN_POINT('Ctrl Pts',(-0.305969350511039,0.775852146239502,
-7.28310678211768));
#60488=CARTESIAN_POINT('Ctrl Pts',(-0.0154480533723153,0.833747891996867,
-7.29369784778061));
#60489=CARTESIAN_POINT('Ctrl Pts',(0.235530167590292,0.756228716617091,
-7.30428891344354));
#60490=CARTESIAN_POINT('Ctrl Pts',(0.361019278071595,0.717469128927203,
-7.30958444627501));
#60491=CARTESIAN_POINT('Ctrl Pts',(0.47662261950887,0.64485581095303,-7.31487997910647));
#60492=CARTESIAN_POINT('Ctrl Pts',(0.568264721859209,0.549936321804992,
-7.32017551193793));
#60493=CARTESIAN_POINT('Ctrl Pts',(0.659906824209543,0.455016832656958,
-7.3254710447694));
#60494=CARTESIAN_POINT('Ctrl Pts',(0.727587687472945,0.337791172335062,
-7.33076657760086));
#60495=CARTESIAN_POINT('Ctrl Pts',(0.762580140965066,0.211371190506761,
-7.33606211043232));
#60496=CARTESIAN_POINT('Ctrl Pts',(0.79757259445719,0.0849512086784458,
-7.34135764326379));
#60497=CARTESIAN_POINT('Ctrl Pts',(0.799876638178026,-0.0506630946562756,
-7.34665317609526));
#60498=CARTESIAN_POINT('Ctrl Pts',(0.770219737559319,-0.179172957285143,
-7.35194870892672));
#60499=CARTESIAN_POINT('Ctrl Pts',(0.740562836940614,-0.307682819914002,
-7.35724424175819));
#60500=CARTESIAN_POINT('Ctrl Pts',(0.678944991982372,-0.429088241837008,
-7.36253977458965));
#60501=CARTESIAN_POINT('Ctrl Pts',(0.591287272089202,-0.526872276190706,
-7.36783530742111));
#60502=CARTESIAN_POINT('Ctrl Pts',(0.415971832302867,-0.722440344898095,
-7.37842637308404));
#60503=CARTESIAN_POINT('Ctrl Pts',(0.136496892776829,-0.823522863328255,
-7.38901743874697));
#60504=CARTESIAN_POINT('Ctrl Pts',(-0.122148664389583,-0.783027285047501,
-7.3996085044099));
#60505=CARTESIAN_POINT('Ctrl Pts',(-0.380794221556001,-0.742531706766746,
-7.41019957007283));
#60506=CARTESIAN_POINT('Ctrl Pts',(-0.618610396362793,-0.560458031775068,
-7.42079063573576));
#60507=CARTESIAN_POINT('Ctrl Pts',(-0.724732196623136,-0.321029592484128,
-7.43138170139869));
#60508=CARTESIAN_POINT('Ctrl Pts',(-0.769104306844893,-0.220918728624132,
-7.43581008399122));
#60509=CARTESIAN_POINT('Ctrl Pts',(-0.790452555110128,-0.110780646970491,
-7.44023846658376));
#60510=CARTESIAN_POINT('Ctrl Pts',(-0.789800442128824,-0.000456880331022313,
-7.44466684917629));
#60511=CARTESIAN_POINT('Ctrl Pts',(-0.790956389731621,2.47836052598815E-5,
-7.47313315082367));
#60512=CARTESIAN_POINT('Ctrl Pts',(-0.791255261516135,-0.103754980737926,
-7.46897290773903));
#60513=CARTESIAN_POINT('Ctrl Pts',(-0.771529051809008,-0.20768044077452,
-7.4648126646544));
#60514=CARTESIAN_POINT('Ctrl Pts',(-0.731842388362112,-0.302924165886258,
-7.46065242156976));
#60515=CARTESIAN_POINT('Ctrl Pts',(-0.630808854994587,-0.545393782713588,
-7.45006135590683));
#60516=CARTESIAN_POINT('Ctrl Pts',(-0.400411655188217,-0.731597090389257,
-7.4394702902439));
#60517=CARTESIAN_POINT('Ctrl Pts',(-0.142488267591274,-0.779145933687615,
-7.42887922458097));
#60518=CARTESIAN_POINT('Ctrl Pts',(-0.0135265737928139,-0.802920355336793,
-7.42358369174951));
#60519=CARTESIAN_POINT('Ctrl Pts',(0.122316666953292,-0.79203116089165,
-7.41828815891805));
#60520=CARTESIAN_POINT('Ctrl Pts',(0.247770929032774,-0.750702616278884,
-7.41299262608658));
#60521=CARTESIAN_POINT('Ctrl Pts',(0.373225191112264,-0.709374071666116,
-7.40769709325512));
#60522=CARTESIAN_POINT('Ctrl Pts',(0.488290474525134,-0.63760617688572,
-7.40240156042365));
#60523=CARTESIAN_POINT('Ctrl Pts',(0.577680693555855,-0.541760325560331,
-7.39710602759218));
#60524=CARTESIAN_POINT('Ctrl Pts',(0.756461131617302,-0.350068622909547,
-7.38651496192925));
#60525=CARTESIAN_POINT('Ctrl Pts',(0.832541312150155,-0.0620650940787978,
-7.37592389626633));
#60526=CARTESIAN_POINT('Ctrl Pts',(0.769043337874916,0.192013282204457,
-7.3653328306034));
#60527=CARTESIAN_POINT('Ctrl Pts',(0.705545363599678,0.446091658487705,
-7.35474176494047));
#60528=CARTESIAN_POINT('Ctrl Pts',(0.502469234516344,0.666244882223448,
-7.34415069927754));
#60529=CARTESIAN_POINT('Ctrl Pts',(0.254597269143168,0.750488011820216,
-7.33355963361461));
#60530=CARTESIAN_POINT('Ctrl Pts',(0.0067253037699912,0.834731141416984,
-7.32296856795168));
#60531=CARTESIAN_POINT('Ctrl Pts',(-0.285942497893035,0.783064176874781,
-7.31237750228875));
#60532=CARTESIAN_POINT('Ctrl Pts',(-0.492193727927431,0.620451744893963,
-7.30178643662582));
#60533=CARTESIAN_POINT('Ctrl Pts',(-0.595319342944629,0.539145528903554,
-7.29649090379436));
#60534=CARTESIAN_POINT('Ctrl Pts',(-0.676840815054672,0.43010294605349,
-7.29119537096289));
#60535=CARTESIAN_POINT('Ctrl Pts',(-0.728092771174107,0.308581122741266,
-7.28589983813143));
#60536=CARTESIAN_POINT('Ctrl Pts',(-0.769279542396317,0.210924527476826,
-7.28164427569551));
#60537=CARTESIAN_POINT('Ctrl Pts',(-0.790918414901856,0.105208902504377,
-7.27738871325959));
#60538=CARTESIAN_POINT('Ctrl Pts',(-0.79118714610156,-0.000297183305454875,
-7.27313315082367));
#60539=CARTESIAN_POINT('Origin',(0.,0.,-5.925));
#60540=CARTESIAN_POINT('',(-0.791588575322523,0.000669637297368075,-7.04466684917629));
#60541=CARTESIAN_POINT('',(-0.79166200567261,0.000301740142700173,-7.07313315082367));
#60542=CARTESIAN_POINT('',(-0.7911,-9.68818082805471E-17,-5.925));
#60543=CARTESIAN_POINT('Ctrl Pts',(-0.791588575322523,0.000669637297368075,
-7.04466684917629));
#60544=CARTESIAN_POINT('Ctrl Pts',(-0.791840267553662,0.0457204045308561,
-7.04647901196194));
#60545=CARTESIAN_POINT('Ctrl Pts',(-0.788201041072123,0.0906952463488291,
-7.04829117474759));
#60546=CARTESIAN_POINT('Ctrl Pts',(-0.78049488948999,0.134903742954435,
-7.05010333753324));
#60547=CARTESIAN_POINT('Ctrl Pts',(-0.735456795748511,0.393277380310535,
-7.06069440319616));
#60548=CARTESIAN_POINT('Ctrl Pts',(-0.551503082409662,0.62547465164853,
-7.0712854688591));
#60549=CARTESIAN_POINT('Ctrl Pts',(-0.310027561283053,0.728861607526646,
-7.08187653452203));
#60550=CARTESIAN_POINT('Ctrl Pts',(-0.189289800719745,0.780555085465705,
-7.08717206735349));
#60551=CARTESIAN_POINT('Ctrl Pts',(-0.0541715882094928,0.800045984539794,
-7.09246760018496));
#60552=CARTESIAN_POINT('Ctrl Pts',(0.0771235418761442,0.787023958617911,
-7.09776313301642));
#60553=CARTESIAN_POINT('Ctrl Pts',(0.208418671961781,0.774001932696027,
-7.10305866584788));
#60554=CARTESIAN_POINT('Ctrl Pts',(0.335890719622808,0.728466981778171,
-7.10835419867935));
#60555=CARTESIAN_POINT('Ctrl Pts',(0.44439992785956,0.654763282178348,-7.11364973151082));
#60556=CARTESIAN_POINT('Ctrl Pts',(0.552909136096312,0.581059582578525,
-7.11894526434228));
#60557=CARTESIAN_POINT('Ctrl Pts',(0.642455504908794,0.479187134296732,
-7.12424079717374));
#60558=CARTESIAN_POINT('Ctrl Pts',(0.703042458559388,0.362039630718822,
-7.12953633000521));
#60559=CARTESIAN_POINT('Ctrl Pts',(0.763629412209986,0.244892127140904,
-7.13483186283667));
#60560=CARTESIAN_POINT('Ctrl Pts',(0.795256950698695,0.112469568266862,
-7.14012739566814));
#60561=CARTESIAN_POINT('Ctrl Pts',(0.791745773177158,-0.0188059620644556,
-7.1454229284996));
#60562=CARTESIAN_POINT('Ctrl Pts',(0.784723418134085,-0.281357022727077,
-7.15601399416253));
#60563=CARTESIAN_POINT('Ctrl Pts',(0.637146199050064,-0.539319969218789,
-7.16660505982546));
#60564=CARTESIAN_POINT('Ctrl Pts',(0.413794019970774,-0.67588943946288,
-7.17719612548839));
#60565=CARTESIAN_POINT('Ctrl Pts',(0.190441840891483,-0.81245890970697,
-7.18778719115132));
#60566=CARTESIAN_POINT('Ctrl Pts',(-0.108685298183076,-0.82763490370342,
-7.19837825681425));
#60567=CARTESIAN_POINT('Ctrl Pts',(-0.344564940049599,-0.713842950628033,
-7.20896932247718));
#60568=CARTESIAN_POINT('Ctrl Pts',(-0.580444581916116,-0.600050997552649,
-7.21956038814011));
#60569=CARTESIAN_POINT('Ctrl Pts',(-0.753076726574608,-0.357291097405433,
-7.23015145380304));
#60570=CARTESIAN_POINT('Ctrl Pts',(-0.785979164073213,-0.0972419030109067,
-7.24074251946596));
#60571=CARTESIAN_POINT('Ctrl Pts',(-0.790042967066146,-0.0651230457215302,
-7.24205062936941));
#60572=CARTESIAN_POINT('Ctrl Pts',(-0.791975208424256,-0.0327404421103452,
-7.24335873927285));
#60573=CARTESIAN_POINT('Ctrl Pts',(-0.791849645310631,-0.000332508792182717,
-7.2446668491763));
#60574=CARTESIAN_POINT('Ctrl Pts',(-0.79118714610156,-0.000297183305454875,
-7.27313315082367));
#60575=CARTESIAN_POINT('Ctrl Pts',(-0.791252818382547,-0.026080662562157,
-7.27209318042813));
#60576=CARTESIAN_POINT('Ctrl Pts',(-0.790042241667021,-0.0518516279031952,
-7.27105321003258));
#60577=CARTESIAN_POINT('Ctrl Pts',(-0.787528821063515,-0.0774894029197258,
-7.27001323963704));
#60578=CARTESIAN_POINT('Ctrl Pts',(-0.774730474704658,-0.208037041494106,
-7.26471770680557));
#60579=CARTESIAN_POINT('Ctrl Pts',(-0.728151341858118,-0.335131254868476,
-7.25942217397411));
#60580=CARTESIAN_POINT('Ctrl Pts',(-0.65414120250197,-0.4443580080739,-7.25412664114264));
#60581=CARTESIAN_POINT('Ctrl Pts',(-0.580131063145823,-0.553584761279323,
-7.24883110831117));
#60582=CARTESIAN_POINT('Ctrl Pts',(-0.478689917280069,-0.644944054315796,
-7.24353557547971));
#60583=CARTESIAN_POINT('Ctrl Pts',(-0.361704854671847,-0.704645960598841,
-7.23824004264825));
#60584=CARTESIAN_POINT('Ctrl Pts',(-0.127734729455401,-0.824049773164929,
-7.22764897698532));
#60585=CARTESIAN_POINT('Ctrl Pts',(0.168411062730911,-0.816824038717297,
-7.21705791132239));
#60586=CARTESIAN_POINT('Ctrl Pts',(0.395778758995229,-0.686098000515455,
-7.20646684565946));
#60587=CARTESIAN_POINT('Ctrl Pts',(0.509462607127388,-0.620734981414534,
-7.201171312828));
#60588=CARTESIAN_POINT('Ctrl Pts',(0.605951931279045,-0.524496886375062,
-7.19587577999653));
#60589=CARTESIAN_POINT('Ctrl Pts',(0.674817884216283,-0.411783528693883,
-7.19058024716507));
#60590=CARTESIAN_POINT('Ctrl Pts',(0.743683837153516,-0.299070171012709,
-7.1852847143336));
#60591=CARTESIAN_POINT('Ctrl Pts',(0.784926418876335,-0.169881550689812,
-7.17998918150214));
#60592=CARTESIAN_POINT('Ctrl Pts',(0.7910127788093,-0.0389617481486627,
-7.17469364867067));
#60593=CARTESIAN_POINT('Ctrl Pts',(0.803185498675229,0.222877856933658,
-7.16410258300775));
#60594=CARTESIAN_POINT('Ctrl Pts',(0.674733331381749,0.491642190889068,
-7.15351151734481));
#60595=CARTESIAN_POINT('Ctrl Pts',(0.461857506030851,0.644192828426151,
-7.14292045168188));
#60596=CARTESIAN_POINT('Ctrl Pts',(0.248981680679959,0.796743465963228,
-7.13232938601895));
#60597=CARTESIAN_POINT('Ctrl Pts',(-0.0483178027283369,0.833080407081984,
-7.12173832035603));
#60598=CARTESIAN_POINT('Ctrl Pts',(-0.291778532425519,0.736829229439651,
-7.1111472546931));
#60599=CARTESIAN_POINT('Ctrl Pts',(-0.535239262122695,0.64057805179732,
-7.10055618903017));
#60600=CARTESIAN_POINT('Ctrl Pts',(-0.724861238108755,0.411738755393912,
-7.08996512336723));
#60601=CARTESIAN_POINT('Ctrl Pts',(-0.77679647965955,0.154279819618756,
-7.07937405770431));
#60602=CARTESIAN_POINT('Ctrl Pts',(-0.786997625186592,0.103709609629245,
-7.07729375541076));
#60603=CARTESIAN_POINT('Ctrl Pts',(-0.791886677657495,0.0520352250930769,
-7.07521345311722));
#60604=CARTESIAN_POINT('Ctrl Pts',(-0.79166200567261,0.000301740142700173,
-7.07313315082367));
#60605=CARTESIAN_POINT('Origin',(0.,0.,-5.925));
#60606=CARTESIAN_POINT('',(-0.790368242092622,-4.0643268100924E-5,-6.8446668491763));
#60607=CARTESIAN_POINT('',(-0.790586355510369,0.000136246675610042,-6.87313315082367));
#60608=CARTESIAN_POINT('',(-0.7911,-9.68818082805471E-17,-5.925));
#60609=CARTESIAN_POINT('Ctrl Pts',(-0.789428704647104,-9.28270190198588E-5,
-6.8446668491763));
#60610=CARTESIAN_POINT('Ctrl Pts',(-0.789627609852131,0.122617963089258,
-6.84959928465104));
#60611=CARTESIAN_POINT('Ctrl Pts',(-0.762676444066611,0.245335071236163,
-6.85453172012578));
#60612=CARTESIAN_POINT('Ctrl Pts',(-0.708130487639264,0.354834530672168,
-6.85946415560052));
#60613=CARTESIAN_POINT('Ctrl Pts',(-0.649569173545256,0.472394706662429,
-6.86475968843198));
#60614=CARTESIAN_POINT('Ctrl Pts',(-0.559200793589236,0.574719593190071,
-6.87005522126344));
#60615=CARTESIAN_POINT('Ctrl Pts',(-0.450699011174817,0.64978854520237,
-6.87535075409491));
#60616=CARTESIAN_POINT('Ctrl Pts',(-0.342197228760398,0.724857497214669,
-6.88064628692637));
#60617=CARTESIAN_POINT('Ctrl Pts',(-0.215562043887583,0.772670514711624,
-6.88594181975784));
#60618=CARTESIAN_POINT('Ctrl Pts',(-0.085145053365461,0.78673793060833,
-6.89123735258931));
#60619=CARTESIAN_POINT('Ctrl Pts',(0.0452719371566612,0.800805346505035,
-6.89653288542077));
#60620=CARTESIAN_POINT('Ctrl Pts',(0.179470733328086,0.781127160801492,
-6.90182841825223));
#60621=CARTESIAN_POINT('Ctrl Pts',(0.301485273272662,0.73105952066025,-6.9071239510837));
#60622=CARTESIAN_POINT('Ctrl Pts',(0.423499813217231,0.680991880519011,
-6.91241948391516));
#60623=CARTESIAN_POINT('Ctrl Pts',(0.533330096934947,0.60053478594008,-6.91771501674662));
#60624=CARTESIAN_POINT('Ctrl Pts',(0.61563544230515,0.498204813034557,-6.92301054957809));
#60625=CARTESIAN_POINT('Ctrl Pts',(0.780246133045565,0.293544867223497,
-6.93360161524102));
#60626=CARTESIAN_POINT('Ctrl Pts',(0.834757070395902,0.00139340810604574,
-6.94419268090395));
#60627=CARTESIAN_POINT('Ctrl Pts',(0.752928668151673,-0.247286162201554,
-6.95478374656688));
#60628=CARTESIAN_POINT('Ctrl Pts',(0.671100265907444,-0.495965732509153,
-6.96537481222981));
#60629=CARTESIAN_POINT('Ctrl Pts',(0.45293252406866,-0.701173414006912,
-6.97596587789274));
#60630=CARTESIAN_POINT('Ctrl Pts',(0.199483730741222,-0.76713949008136,
-6.98655694355566));
#60631=CARTESIAN_POINT('Ctrl Pts',(-0.0539650625862154,-0.833105566155808,
-6.99714800921859));
#60632=CARTESIAN_POINT('Ctrl Pts',(-0.342694907402299,-0.759830036806941,
-7.00773907488152));
#60633=CARTESIAN_POINT('Ctrl Pts',(-0.536116319172053,-0.582922401676084,
-7.01833014054445));
#60634=CARTESIAN_POINT('Ctrl Pts',(-0.632827025056924,-0.49446858411066,
-7.02362567337592));
#60635=CARTESIAN_POINT('Ctrl Pts',(-0.705710622680213,-0.380106740099744,
-7.02892120620738));
#60636=CARTESIAN_POINT('Ctrl Pts',(-0.748257350506165,-0.255060363002999,
-7.03421673903885));
#60637=CARTESIAN_POINT('Ctrl Pts',(-0.776244335380633,-0.172805598812202,
-7.03770010908466));
#60638=CARTESIAN_POINT('Ctrl Pts',(-0.791104768246437,-0.0859277116632267,
-7.04118347913048));
#60639=CARTESIAN_POINT('Ctrl Pts',(-0.791588575322523,0.000669637297368075,
-7.04466684917629));
#60640=CARTESIAN_POINT('Ctrl Pts',(-0.79166200567261,0.000301740142700173,
-7.07313315082367));
#60641=CARTESIAN_POINT('Ctrl Pts',(-0.79131476179894,-0.0796554281791444,
-7.06991792028576));
#60642=CARTESIAN_POINT('Ctrl Pts',(-0.778752090620685,-0.159753772823585,
-7.06670268974784));
#60643=CARTESIAN_POINT('Ctrl Pts',(-0.754706361115264,-0.236134921687598,
-7.06348745920992));
#60644=CARTESIAN_POINT('Ctrl Pts',(-0.715102684629,-0.361935817375853,-7.05819192637846));
#60645=CARTESIAN_POINT('Ctrl Pts',(-0.64434939448989,-0.477653231021849,
-7.05289639354698));
#60646=CARTESIAN_POINT('Ctrl Pts',(-0.550084282291531,-0.568870401714096,
-7.04760086071552));
#60647=CARTESIAN_POINT('Ctrl Pts',(-0.455819170093172,-0.660087572406342,
-7.04230532788405));
#60648=CARTESIAN_POINT('Ctrl Pts',(-0.338042235835557,-0.726804500144844,
-7.0370097950526));
#60649=CARTESIAN_POINT('Ctrl Pts',(-0.210924183965184,-0.762145485303659,
-7.03171426222113));
#60650=CARTESIAN_POINT('Ctrl Pts',(-0.0838061320948113,-0.797486470462474,
-7.02641872938967));
#60651=CARTESIAN_POINT('Ctrl Pts',(0.0526530373883043,-0.801451513041607,
-7.0211231965582));
#60652=CARTESIAN_POINT('Ctrl Pts',(0.180466151444074,-0.771225194002639,
-7.01582766372673));
#60653=CARTESIAN_POINT('Ctrl Pts',(0.436092379555614,-0.710772555924703,
-7.0052365980638));
#60654=CARTESIAN_POINT('Ctrl Pts',(0.657134385957696,-0.513554471374351,
-6.99464553240088));
#60655=CARTESIAN_POINT('Ctrl Pts',(0.74580613841404,-0.266729256526248,
-6.98405446673795));
#60656=CARTESIAN_POINT('Ctrl Pts',(0.790142014642215,-0.14331664910219,
-6.97875893390648));
#60657=CARTESIAN_POINT('Ctrl Pts',(0.801385327383953,-0.00750225910368728,
-6.97346340107502));
#60658=CARTESIAN_POINT('Ctrl Pts',(0.780909059079954,0.122987368492008,
-6.96816786824355));
#60659=CARTESIAN_POINT('Ctrl Pts',(0.760432790775956,0.253476996087696,
-6.96287233541209));
#60660=CARTESIAN_POINT('Ctrl Pts',(0.708236941426225,0.378641861280584,
-6.95757680258063));
#60661=CARTESIAN_POINT('Ctrl Pts',(0.62812465768728,0.482367752304858,-6.95228126974916));
#60662=CARTESIAN_POINT('Ctrl Pts',(0.467900090209389,0.689819534353405,
-6.94169020408624));
#60663=CARTESIAN_POINT('Ctrl Pts',(0.196009785174654,0.811515419727503,
-6.9310991384233));
#60664=CARTESIAN_POINT('Ctrl Pts',(-0.0649962387595744,0.789982433361549,
-6.92050807276037));
#60665=CARTESIAN_POINT('Ctrl Pts',(-0.326002262693803,0.768449446995596,
-6.90991700709744));
#60666=CARTESIAN_POINT('Ctrl Pts',(-0.57612400552752,0.603687588889572,
-6.89932594143451));
#60667=CARTESIAN_POINT('Ctrl Pts',(-0.699379104787005,0.372720931969687,
-6.88873487577159));
#60668=CARTESIAN_POINT('Ctrl Pts',(-0.759901568351269,0.259308414662271,
-6.88353430078895));
#60669=CARTESIAN_POINT('Ctrl Pts',(-0.789834639283667,0.129932957625574,
-6.87833372580631));
#60670=CARTESIAN_POINT('Ctrl Pts',(-0.789580398820022,0.000403081535511013,
-6.87313315082368));
#60671=CARTESIAN_POINT('Origin',(0.,0.,-5.925));
#60672=CARTESIAN_POINT('',(-0.7911,2.4980018054066E-14,-6.6446668491763));
#60673=CARTESIAN_POINT('',(-0.7911,-5.4195536947077E-13,-6.67313315082367));
#60674=CARTESIAN_POINT('',(-0.7911,-9.68818082805471E-17,-5.925));
#60675=CARTESIAN_POINT('Ctrl Pts',(-0.7911,2.4980018054066E-15,-6.6446668491763));
#60676=CARTESIAN_POINT('Ctrl Pts',(-0.791099999999999,0.220167589666675,
-6.65352559274957));
#60677=CARTESIAN_POINT('Ctrl Pts',(-0.694214576672374,0.438610418338676,
-6.66238433632284));
#60678=CARTESIAN_POINT('Ctrl Pts',(-0.531017389080337,0.58639555122315,
-6.67124307989611));
#60679=CARTESIAN_POINT('Ctrl Pts',(-0.3678202014883,0.734180684107624,-6.68010182346939));
#60680=CARTESIAN_POINT('Ctrl Pts',(-0.140868175871764,0.808992666571332,
-6.68896056704266));
#60681=CARTESIAN_POINT('Ctrl Pts',(0.0782205473247404,0.787223447298299,
-6.69781931061593));
#60682=CARTESIAN_POINT('Ctrl Pts',(0.297309270521245,0.765454228025267,
-6.7066780541892));
#60683=CARTESIAN_POINT('Ctrl Pts',(0.505102072675574,0.647444880834246,
-6.71553679776247));
#60684=CARTESIAN_POINT('Ctrl Pts',(0.636026795761714,0.470435038100997,
-6.72439554133575));
#60685=CARTESIAN_POINT('Ctrl Pts',(0.766951518847854,0.293425195367748,
-6.73325428490902));
#60686=CARTESIAN_POINT('Ctrl Pts',(0.818956872247066,0.0601881960099669,
-6.74211302848229));
#60687=CARTESIAN_POINT('Ctrl Pts',(0.775631781004217,-0.155674501111215,
-6.75097177205557));
#60688=CARTESIAN_POINT('Ctrl Pts',(0.732306689761369,-0.371537198232396,
-6.75983051562884));
#60689=CARTESIAN_POINT('Ctrl Pts',(0.594329958850246,-0.566643518936463,
-6.76868925920211));
#60690=CARTESIAN_POINT('Ctrl Pts',(0.405242230244082,-0.67942471608472,
-6.77754800277538));
#60691=CARTESIAN_POINT('Ctrl Pts',(0.216154501637919,-0.792205913232977,
-6.78640674634865));
#60692=CARTESIAN_POINT('Ctrl Pts',(-0.0210816529299573,-0.820894963713003,
-6.79526548992193));
#60693=CARTESIAN_POINT('Ctrl Pts',(-0.23160278075316,-0.756438604215441,
-6.8041242334952));
#60694=CARTESIAN_POINT('Ctrl Pts',(-0.442123908576362,-0.691982244717878,
-6.81298297706847));
#60695=CARTESIAN_POINT('Ctrl Pts',(-0.622631625634126,-0.535390358803591,
-6.82184172064174));
#60696=CARTESIAN_POINT('Ctrl Pts',(-0.716163994722123,-0.336077881842366,
-6.83070046421502));
#60697=CARTESIAN_POINT('Ctrl Pts',(-0.765317280859478,-0.231334857514573,
-6.83535592586878));
#60698=CARTESIAN_POINT('Ctrl Pts',(-0.791100000000004,-0.11570283783653,
-6.84001138752254));
#60699=CARTESIAN_POINT('Ctrl Pts',(-0.7911,3.0364599723498E-14,-6.8446668491763));
#60700=CARTESIAN_POINT('Ctrl Pts',(-0.7911,-5.58997292898766E-13,-6.87313315082367));
#60701=CARTESIAN_POINT('Ctrl Pts',(-0.791099999999845,-0.220167589667239,
-6.8642744072504));
#60702=CARTESIAN_POINT('Ctrl Pts',(-0.694214576672059,-0.438610418339179,
-6.85541566367713));
#60703=CARTESIAN_POINT('Ctrl Pts',(-0.531017389079908,-0.586395551223539,
-6.84655692010385));
#60704=CARTESIAN_POINT('Ctrl Pts',(-0.367820201487757,-0.734180684107898,
-6.83769817653058));
#60705=CARTESIAN_POINT('Ctrl Pts',(-0.140868175871157,-0.80899266657144,
-6.82883943295731));
#60706=CARTESIAN_POINT('Ctrl Pts',(0.078220547325339,-0.78722344729824,
-6.81998068938404));
#60707=CARTESIAN_POINT('Ctrl Pts',(0.297309270521835,-0.76545422802504,
-6.81112194581076));
#60708=CARTESIAN_POINT('Ctrl Pts',(0.50510207267608,-0.647444880833854,
-6.80226320223749));
#60709=CARTESIAN_POINT('Ctrl Pts',(0.636026795762085,-0.470435038100496,
-6.79340445866422));
#60710=CARTESIAN_POINT('Ctrl Pts',(0.766951518848091,-0.293425195367137,
-6.78454571509095));
#60711=CARTESIAN_POINT('Ctrl Pts',(0.818956872247117,-0.060188196009305,
-6.77568697151767));
#60712=CARTESIAN_POINT('Ctrl Pts',(0.77563178100409,0.155674501111848,-6.7668282279444));
#60713=CARTESIAN_POINT('Ctrl Pts',(0.732306689761064,0.371537198233002,
-6.75796948437113));
#60714=CARTESIAN_POINT('Ctrl Pts',(0.594329958849773,0.566643518936962,
-6.74911074079786));
#60715=CARTESIAN_POINT('Ctrl Pts',(0.405242230243508,0.679424716085063,
-6.74025199722458));
#60716=CARTESIAN_POINT('Ctrl Pts',(0.216154501637242,0.792205913233164,
-6.73139325365131));
#60717=CARTESIAN_POINT('Ctrl Pts',(-0.0210816529306676,0.820894963712987,
-6.72253451007804));
#60718=CARTESIAN_POINT('Ctrl Pts',(-0.231602780753821,0.756438604215238,
-6.71367576650476));
#60719=CARTESIAN_POINT('Ctrl Pts',(-0.442123908576974,0.691982244717489,
-6.70481702293149));
#60720=CARTESIAN_POINT('Ctrl Pts',(-0.622631625634606,0.535390358803036,
-6.69595827935822));
#60721=CARTESIAN_POINT('Ctrl Pts',(-0.716163994722426,0.33607788184172,
-6.68709953578495));
#60722=CARTESIAN_POINT('Ctrl Pts',(-0.765317280859659,0.231334857513943,
-6.68244407413119));
#60723=CARTESIAN_POINT('Ctrl Pts',(-0.791100000000079,0.115702837835951,
-6.67778861247743));
#60724=CARTESIAN_POINT('Ctrl Pts',(-0.7911,-5.4195536947077E-13,-6.67313315082367));
#60725=CARTESIAN_POINT('Origin',(0.,0.,-5.925));
#60726=CARTESIAN_POINT('',(-0.791106330306829,3.30307559588206E-6,-6.4446668491763));
#60727=CARTESIAN_POINT('',(-0.791564826434644,0.000250487832263192,-6.47313315082367));
#60728=CARTESIAN_POINT('',(-0.7911,-9.68818082805471E-17,-5.925));
#60729=CARTESIAN_POINT('Ctrl Pts',(-0.7911,4.20219414820622E-14,-6.4446668491763));
#60730=CARTESIAN_POINT('Ctrl Pts',(-0.791099999999988,0.220167589666714,
-6.45352559274957));
#60731=CARTESIAN_POINT('Ctrl Pts',(-0.694214576672352,0.438610418338711,
-6.46238433632284));
#60732=CARTESIAN_POINT('Ctrl Pts',(-0.531017389080308,0.586395551223177,
-6.47124307989611));
#60733=CARTESIAN_POINT('Ctrl Pts',(-0.367820201488263,0.734180684107642,
-6.48010182346939));
#60734=CARTESIAN_POINT('Ctrl Pts',(-0.140868175871724,0.808992666571339,
-6.48896056704266));
#60735=CARTESIAN_POINT('Ctrl Pts',(0.0782205473247798,0.787223447298295,
-6.49781931061593));
#60736=CARTESIAN_POINT('Ctrl Pts',(0.297309270521284,0.765454228025252,
-6.5066780541892));
#60737=CARTESIAN_POINT('Ctrl Pts',(0.505102072675606,0.647444880834221,
-6.51553679776248));
#60738=CARTESIAN_POINT('Ctrl Pts',(0.636026795761738,0.470435038100965,
-6.52439554133575));
#60739=CARTESIAN_POINT('Ctrl Pts',(0.766951518847869,0.29342519536771,-6.53325428490902));
#60740=CARTESIAN_POINT('Ctrl Pts',(0.818956872247069,0.0601881960099259,
-6.54211302848229));
#60741=CARTESIAN_POINT('Ctrl Pts',(0.77563178100421,-0.155674501111253,
-6.55097177205557));
#60742=CARTESIAN_POINT('Ctrl Pts',(0.73230668976135,-0.371537198232433,
-6.55983051562884));
#60743=CARTESIAN_POINT('Ctrl Pts',(0.594329958850217,-0.566643518936493,
-6.56868925920211));
#60744=CARTESIAN_POINT('Ctrl Pts',(0.405242230244048,-0.67942471608474,
-6.57754800277538));
#60745=CARTESIAN_POINT('Ctrl Pts',(0.216154501637879,-0.792205913232988,
-6.58640674634866));
#60746=CARTESIAN_POINT('Ctrl Pts',(-0.0210816529299984,-0.820894963713002,
-6.59526548992193));
#60747=CARTESIAN_POINT('Ctrl Pts',(-0.231602780753197,-0.756438604215429,
-6.6041242334952));
#60748=CARTESIAN_POINT('Ctrl Pts',(-0.442123908576397,-0.691982244717856,
-6.61298297706847));
#60749=CARTESIAN_POINT('Ctrl Pts',(-0.622631625634152,-0.53539035880356,
-6.62184172064175));
#60750=CARTESIAN_POINT('Ctrl Pts',(-0.716163994722139,-0.336077881842331,
-6.63070046421502));
#60751=CARTESIAN_POINT('Ctrl Pts',(-0.76531728085948,-0.231334857514555,
-6.63535592586878));
#60752=CARTESIAN_POINT('Ctrl Pts',(-0.7911,-0.115702837836536,-6.64001138752254));
#60753=CARTESIAN_POINT('Ctrl Pts',(-0.7911,2.4980018054066E-15,-6.6446668491763));
#60754=CARTESIAN_POINT('Ctrl Pts',(-0.7911,-5.4195536947077E-13,-6.67313315082367));
#60755=CARTESIAN_POINT('Ctrl Pts',(-0.791099999999849,-0.220167589667214,
-6.6642744072504));
#60756=CARTESIAN_POINT('Ctrl Pts',(-0.694214576672075,-0.43861041833915,
-6.65541566367713));
#60757=CARTESIAN_POINT('Ctrl Pts',(-0.531017389079937,-0.586395551223512,
-6.64655692010386));
#60758=CARTESIAN_POINT('Ctrl Pts',(-0.367820201487799,-0.734180684107875,
-6.63769817653058));
#60759=CARTESIAN_POINT('Ctrl Pts',(-0.140868175871213,-0.808992666571428,
-6.62883943295731));
#60760=CARTESIAN_POINT('Ctrl Pts',(0.0782205473252772,-0.787223447298246,
-6.61998068938404));
#60761=CARTESIAN_POINT('Ctrl Pts',(0.297309270521767,-0.765454228025064,
-6.61112194581077));
#60762=CARTESIAN_POINT('Ctrl Pts',(0.505102072676015,-0.647444880833902,
-6.60226320223749));
#60763=CARTESIAN_POINT('Ctrl Pts',(0.636026795762035,-0.470435038100564,
-6.59340445866422));
#60764=CARTESIAN_POINT('Ctrl Pts',(0.766951518848055,-0.293425195367225,
-6.58454571509095));
#60765=CARTESIAN_POINT('Ctrl Pts',(0.818956872247108,-0.0601881960094084,
-6.57568697151768));
#60766=CARTESIAN_POINT('Ctrl Pts',(0.775631781004111,0.155674501111744,
-6.5668282279444));
#60767=CARTESIAN_POINT('Ctrl Pts',(0.732306689761115,0.371537198232896,
-6.55796948437113));
#60768=CARTESIAN_POINT('Ctrl Pts',(0.594329958849859,0.566643518936868,
-6.54911074079786));
#60769=CARTESIAN_POINT('Ctrl Pts',(0.405242230243619,0.679424716084996,
-6.54025199722459));
#60770=CARTESIAN_POINT('Ctrl Pts',(0.216154501637378,0.792205913233125,
-6.53139325365132));
#60771=CARTESIAN_POINT('Ctrl Pts',(-0.021081652930517,0.820894963712989,
-6.52253451007804));
#60772=CARTESIAN_POINT('Ctrl Pts',(-0.231602780753675,0.756438604215283,
-6.51367576650477));
#60773=CARTESIAN_POINT('Ctrl Pts',(-0.442123908576834,0.691982244717576,
-6.5048170229315));
#60774=CARTESIAN_POINT('Ctrl Pts',(-0.622631625634491,0.535390358803167,
-6.49595827935823));
#60775=CARTESIAN_POINT('Ctrl Pts',(-0.716163994722352,0.336077881841878,
-6.48709953578495));
#60776=CARTESIAN_POINT('Ctrl Pts',(-0.76531728085963,0.231334857514065,
-6.48244407413119));
#60777=CARTESIAN_POINT('Ctrl Pts',(-0.791100000000077,0.115702837836021,
-6.47778861247743));
#60778=CARTESIAN_POINT('Ctrl Pts',(-0.7911,-5.24857934891543E-13,-6.47313315082367));
#60779=CARTESIAN_POINT('Origin',(0.,0.,-5.925));
#60780=CARTESIAN_POINT('',(-0.791105591446152,0.000150202279374845,-6.2446668491763));
#60781=CARTESIAN_POINT('',(-0.789646943890772,0.00034450190664909,-6.27313315082367));
#60782=CARTESIAN_POINT('',(-0.7911,-9.68818082805471E-17,-5.925));
#60783=CARTESIAN_POINT('Ctrl Pts',(-0.791105591446152,0.000150202279374845,
-6.2446668491763));
#60784=CARTESIAN_POINT('Ctrl Pts',(-0.79144237439907,0.0923771225581108,
-6.24836903705538));
#60785=CARTESIAN_POINT('Ctrl Pts',(-0.775893102399071,0.184576764100862,
-6.25207122493447));
#60786=CARTESIAN_POINT('Ctrl Pts',(-0.744247893335028,0.270759032458304,
-6.25577341281355));
#60787=CARTESIAN_POINT('Ctrl Pts',(-0.653718590646796,0.517305694314754,
-6.26636447847648));
#60788=CARTESIAN_POINT('Ctrl Pts',(-0.431461112281039,0.714606537868241,
-6.27695554413941));
#60789=CARTESIAN_POINT('Ctrl Pts',(-0.176182923218375,0.772665632828024,
-6.28754660980234));
#60790=CARTESIAN_POINT('Ctrl Pts',(0.0790952658442903,0.830724727787806,
-6.29813767546527));
#60791=CARTESIAN_POINT('Ctrl Pts',(0.367394165603863,0.749542074153883,
-6.3087287411282));
#60792=CARTESIAN_POINT('Ctrl Pts',(0.554559547305794,0.56635654910048,-6.31931980679113));
#60793=CARTESIAN_POINT('Ctrl Pts',(0.741724929007724,0.383171024047077,
-6.32991087245406));
#60794=CARTESIAN_POINT('Ctrl Pts',(0.827756792652013,0.0979826275741944,
-6.34050193811698));
#60795=CARTESIAN_POINT('Ctrl Pts',(0.775857090223025,-0.158950432914308,
-6.35109300377991));
#60796=CARTESIAN_POINT('Ctrl Pts',(0.749907239008532,-0.287416963158559,
-6.35638853661138));
#60797=CARTESIAN_POINT('Ctrl Pts',(0.689474496275719,-0.408819659406715,
-6.36168406944284));
#60798=CARTESIAN_POINT('Ctrl Pts',(0.604249241889583,-0.509732962576653,
-6.36697960227431));
#60799=CARTESIAN_POINT('Ctrl Pts',(0.519023987503447,-0.61064626574659,
-6.37227513510577));
#60800=CARTESIAN_POINT('Ctrl Pts',(0.409006221463986,-0.691070175838309,
-6.37757066793724));
#60801=CARTESIAN_POINT('Ctrl Pts',(0.286695534736869,-0.738360975552133,
-6.3828662007687));
#60802=CARTESIAN_POINT('Ctrl Pts',(0.0420741612826401,-0.832942574979778,
-6.39345726643163));
#60803=CARTESIAN_POINT('Ctrl Pts',(-0.251718894922216,-0.794991732895852,
-6.40404833209456));
#60804=CARTESIAN_POINT('Ctrl Pts',(-0.464779911730617,-0.641354845576358,
-6.41463939775749));
#60805=CARTESIAN_POINT('Ctrl Pts',(-0.57131042013482,-0.564536401916609,
-6.41993493058895));
#60806=CARTESIAN_POINT('Ctrl Pts',(-0.657657918689909,-0.458796446947966,
-6.42523046342042));
#60807=CARTESIAN_POINT('Ctrl Pts',(-0.714173715474753,-0.339574174989383,
-6.43052599625189));
#60808=CARTESIAN_POINT('Ctrl Pts',(-0.764479107816768,-0.233452992807072,
-6.43523961389336));
#60809=CARTESIAN_POINT('Ctrl Pts',(-0.791148858337168,-0.116649777874704,
-6.43995323153483));
#60810=CARTESIAN_POINT('Ctrl Pts',(-0.791304868704775,0.000106897948089511,
-6.4446668491763));
#60811=CARTESIAN_POINT('Ctrl Pts',(-0.792405686160893,0.000703614237492454,
-6.47313315082367));
#60812=CARTESIAN_POINT('Ctrl Pts',(-0.790931820918324,-0.240478805143301,
-6.46339213985864));
#60813=CARTESIAN_POINT('Ctrl Pts',(-0.672291318622103,-0.48357032053066,
-6.4536511288936));
#60814=CARTESIAN_POINT('Ctrl Pts',(-0.481013815618491,-0.629823575980568,
-6.44391011792856));
#60815=CARTESIAN_POINT('Ctrl Pts',(-0.273044375749921,-0.788839702483944,
-6.43331905226563));
#60816=CARTESIAN_POINT('Ctrl Pts',(0.0207926315836592,-0.833378830523809,
-6.4227279866027));
#60817=CARTESIAN_POINT('Ctrl Pts',(0.268185334101307,-0.745178944639886,
-6.41213692093977));
#60818=CARTESIAN_POINT('Ctrl Pts',(0.39188168536012,-0.701079001697929,
-6.40684138810831));
#60819=CARTESIAN_POINT('Ctrl Pts',(0.50396696041495,-0.623794305275027,
-6.40154585527685));
#60820=CARTESIAN_POINT('Ctrl Pts',(0.591355703565141,-0.525014117087408,
-6.39625032244538));
#60821=CARTESIAN_POINT('Ctrl Pts',(0.678744446715342,-0.426233928899778,
-6.39095478961392));
#60822=CARTESIAN_POINT('Ctrl Pts',(0.741436657960902,-0.305958248947421,
-6.38565925678245));
#60823=CARTESIAN_POINT('Ctrl Pts',(0.771015028956397,-0.178163093565044,
-6.38036372395099));
#60824=CARTESIAN_POINT('Ctrl Pts',(0.800593399951893,-0.0503679381826663,
-6.37506819111952));
#60825=CARTESIAN_POINT('Ctrl Pts',(0.797057930697324,0.084946692629738,
-6.36977265828806));
#60826=CARTESIAN_POINT('Ctrl Pts',(0.761820860783038,0.212093593185943,
-6.36447712545659));
#60827=CARTESIAN_POINT('Ctrl Pts',(0.726583790868755,0.339240493742134,
-6.35918159262512));
#60828=CARTESIAN_POINT('Ctrl Pts',(0.659645120294761,0.458219664042133,
-6.35388605979366));
#60829=CARTESIAN_POINT('Ctrl Pts',(0.567863458218445,0.552166186136732,
-6.3485905269622));
#60830=CARTESIAN_POINT('Ctrl Pts',(0.384300134065797,0.740059230325945,
-6.33799946129927));
#60831=CARTESIAN_POINT('Ctrl Pts',(0.101364843903861,0.827821681693549,
-6.32740839563635));
#60832=CARTESIAN_POINT('Ctrl Pts',(-0.155850887918912,0.776583389335134,
-6.31681732997342));
#60833=CARTESIAN_POINT('Ctrl Pts',(-0.284458753830295,0.750964243155928,
-6.31152179714195));
#60834=CARTESIAN_POINT('Ctrl Pts',(-0.406636730156887,0.690594911045214,
-6.30622626431048));
#60835=CARTESIAN_POINT('Ctrl Pts',(-0.50790244458249,0.60578869768958,-6.30093073147902));
#60836=CARTESIAN_POINT('Ctrl Pts',(-0.609168159008086,0.520982484333951,
-6.29563519864755));
#60837=CARTESIAN_POINT('Ctrl Pts',(-0.689521611532702,0.411739389733399,
-6.29033966581609));
#60838=CARTESIAN_POINT('Ctrl Pts',(-0.737113985579674,0.289624648184222,
-6.28504413298462));
#60839=CARTESIAN_POINT('Ctrl Pts',(-0.77279638281976,0.198069082737379,
-6.28107380559764));
#60840=CARTESIAN_POINT('Ctrl Pts',(-0.790062941498036,0.0992780359435954,
-6.27710347821066));
#60841=CARTESIAN_POINT('Ctrl Pts',(-0.789646943890772,0.00034450190664909,
-6.27313315082367));
#60842=CARTESIAN_POINT('Origin',(0.,0.,-5.925));
#60843=CARTESIAN_POINT('',(-0.790663869694179,-0.000319622920649363,-6.0446668491763));
#60844=CARTESIAN_POINT('',(-0.790931871961626,-0.000575333837205039,-6.07313315082367));
#60845=CARTESIAN_POINT('',(-0.7911,-9.68818082805471E-17,-5.925));
#60846=CARTESIAN_POINT('Ctrl Pts',(-0.79027278667866,-0.00060623243642971,
-6.0446668491763));
#60847=CARTESIAN_POINT('Ctrl Pts',(-0.789239692543626,0.169353443234173,
-6.05148930974447));
#60848=CARTESIAN_POINT('Ctrl Pts',(-0.735523539619875,0.339963444333918,
-6.05831177031265));
#60849=CARTESIAN_POINT('Ctrl Pts',(-0.634255164638182,0.475084083996859,
-6.06513423088083));
#60850=CARTESIAN_POINT('Ctrl Pts',(-0.477047952036308,0.684842946329087,
-6.07572529654376));
#60851=CARTESIAN_POINT('Ctrl Pts',(-0.205245106273596,0.809076344901306,
-6.08631636220669));
#60852=CARTESIAN_POINT('Ctrl Pts',(0.0559109762185824,0.790524027970827,
-6.09690742786962));
#60853=CARTESIAN_POINT('Ctrl Pts',(0.317067058710761,0.771971711040347,
-6.10749849353255));
#60854=CARTESIAN_POINT('Ctrl Pts',(0.567576377932405,0.610633678607169,
-6.11808955919547));
#60855=CARTESIAN_POINT('Ctrl Pts',(0.694329353803112,0.381187901319921,
-6.1286806248584));
#60856=CARTESIAN_POINT('Ctrl Pts',(0.757705841738466,0.266465012676297,
-6.13397615768987));
#60857=CARTESIAN_POINT('Ctrl Pts',(0.790143243836085,0.134715187819156,
-6.13927169052133));
#60858=CARTESIAN_POINT('Ctrl Pts',(0.790491482816431,0.0026078004279992,
-6.14456722335279));
#60859=CARTESIAN_POINT('Ctrl Pts',(0.790839721796777,-0.129499586963158,
-6.14986275618426));
#60860=CARTESIAN_POINT('Ctrl Pts',(0.759098797659849,-0.261964536888331,
-6.15515828901573));
#60861=CARTESIAN_POINT('Ctrl Pts',(0.696510600452876,-0.377164033684325,
-6.1604538218472));
#60862=CARTESIAN_POINT('Ctrl Pts',(0.57133420603893,-0.607563027276312,
-6.17104488751013));
#60863=CARTESIAN_POINT('Ctrl Pts',(0.322768719344804,-0.76890020835158,
-6.18163595317304));
#60864=CARTESIAN_POINT('Ctrl Pts',(0.0609180238672261,-0.789725501077674,
-6.19222701883598));
#60865=CARTESIAN_POINT('Ctrl Pts',(-0.0700073238715702,-0.800138147440722,
-6.19752255166744));
#60866=CARTESIAN_POINT('Ctrl Pts',(-0.20425397380623,-0.775422821716471,
-6.20281808449891));
#60867=CARTESIAN_POINT('Ctrl Pts',(-0.324505308412596,-0.721134851061482,
-6.20811361733038));
#60868=CARTESIAN_POINT('Ctrl Pts',(-0.444756643018949,-0.666846880406498,
-6.21340915016184));
#60869=CARTESIAN_POINT('Ctrl Pts',(-0.551012662297012,-0.582986264820781,
-6.2187046829933));
#60870=CARTESIAN_POINT('Ctrl Pts',(-0.630292184928299,-0.478482327068392,
-6.22400021582476));
#60871=CARTESIAN_POINT('Ctrl Pts',(-0.70957170755959,-0.373978389315996,
-6.22929574865623));
#60872=CARTESIAN_POINT('Ctrl Pts',(-0.761874733544102,-0.248831129396924,
-6.23459128148769));
#60873=CARTESIAN_POINT('Ctrl Pts',(-0.78185994282399,-0.118465106685406,
-6.23988681431916));
#60874=CARTESIAN_POINT('Ctrl Pts',(-0.78787318707,-0.079239961480945,-6.24148015927154));
#60875=CARTESIAN_POINT('Ctrl Pts',(-0.79096064704149,-0.0395423532307859,
-6.24307350422392));
#60876=CARTESIAN_POINT('Ctrl Pts',(-0.791105591446152,0.000150202279374845,
-6.2446668491763));
#60877=CARTESIAN_POINT('Ctrl Pts',(-0.789646943890772,0.00034450190664909,
-6.27313315082367));
#60878=CARTESIAN_POINT('Ctrl Pts',(-0.7889532451066,-0.164632582280567,
-6.26651241254773));
#60879=CARTESIAN_POINT('Ctrl Pts',(-0.739088975450182,-0.330005886277594,
-6.25989167427178));
#60880=CARTESIAN_POINT('Ctrl Pts',(-0.643454389938275,-0.462884953618257,
-6.25327093599584));
#60881=CARTESIAN_POINT('Ctrl Pts',(-0.490469612019563,-0.67544900142945,
-6.24267987033291));
#60882=CARTESIAN_POINT('Ctrl Pts',(-0.220359621998779,-0.804861026158961,
-6.23208880466998));
#60883=CARTESIAN_POINT('Ctrl Pts',(0.0410929792480928,-0.791431595050273,
-6.22149773900705));
#60884=CARTESIAN_POINT('Ctrl Pts',(0.30254558049498,-0.778002163941584,
-6.21090667334412));
#60885=CARTESIAN_POINT('Ctrl Pts',(0.555340792967953,-0.621731276994677,
-6.20031560768119));
#60886=CARTESIAN_POINT('Ctrl Pts',(0.68680223501153,-0.394357794869774,
-6.18972454201826));
#60887=CARTESIAN_POINT('Ctrl Pts',(0.752532956033317,-0.280671053807326,
-6.1844290091868));
#60888=CARTESIAN_POINT('Ctrl Pts',(0.787930234447756,-0.14920866395038,
-6.17913347635533));
#60889=CARTESIAN_POINT('Ctrl Pts',(0.790593478787117,-0.0173465556812871,
-6.17383794352387));
#60890=CARTESIAN_POINT('Ctrl Pts',(0.793256723126477,0.114515552587806,
-6.1685424106924));
#60891=CARTESIAN_POINT('Ctrl Pts',(0.763185933390757,0.246777379269046,
-6.16324687786094));
#60892=CARTESIAN_POINT('Ctrl Pts',(0.702998643332439,0.363326964552898,
-6.15795134502948));
#60893=CARTESIAN_POINT('Ctrl Pts',(0.642811353274121,0.47987654983675,-6.15265581219801));
#60894=CARTESIAN_POINT('Ctrl Pts',(0.552507562893205,0.580713893723215,
-6.14736027936654));
#60895=CARTESIAN_POINT('Ctrl Pts',(0.443345199926037,0.654816159166802,
-6.14206474653508));
#60896=CARTESIAN_POINT('Ctrl Pts',(0.33418283695887,0.728918424610389,-6.13676921370361));
#60897=CARTESIAN_POINT('Ctrl Pts',(0.206161901405452,0.776285611611098,
-6.13147368087215));
#60898=CARTESIAN_POINT('Ctrl Pts',(0.0753900581244591,0.788475561967689,
-6.12617814804069));
#60899=CARTESIAN_POINT('Ctrl Pts',(-0.186153628437527,0.81285546268087,
-6.11558708237776));
#60900=CARTESIAN_POINT('Ctrl Pts',(-0.458700945909811,0.696526416817579,
-6.10499601671483));
#60901=CARTESIAN_POINT('Ctrl Pts',(-0.621527725141712,0.49100204859901,
-6.0944049510519));
#60902=CARTESIAN_POINT('Ctrl Pts',(-0.702941114757658,0.388239864489732,
-6.08910941822044));
#60903=CARTESIAN_POINT('Ctrl Pts',(-0.756924369813512,0.263178849791636,
-6.08381388538897));
#60904=CARTESIAN_POINT('Ctrl Pts',(-0.77923235736188,0.132968109968668,
-6.0785183525575));
#60905=CARTESIAN_POINT('Ctrl Pts',(-0.786794266430465,0.0888295801187872,
-6.07672328531289));
#60906=CARTESIAN_POINT('Ctrl Pts',(-0.790716502172883,0.044099316760431,
-6.07492821806828));
#60907=CARTESIAN_POINT('Ctrl Pts',(-0.790931871961626,-0.000575333837205039,
-6.07313315082367));
#60908=CARTESIAN_POINT('Origin',(0.,0.,-5.925));
#60909=CARTESIAN_POINT('',(-0.7911,9.31477117660506E-14,-5.8446668491763));
#60910=CARTESIAN_POINT('',(-0.792458596363369,-0.000371319283420802,-5.87313315082368));
#60911=CARTESIAN_POINT('',(-0.7911,-9.68818082805471E-17,-5.925));
#60912=CARTESIAN_POINT('Ctrl Pts',(-0.7911,9.31477117660506E-14,-5.8446668491763));
#60913=CARTESIAN_POINT('Ctrl Pts',(-0.791099999999974,0.220167589666758,
-5.85352559274957));
#60914=CARTESIAN_POINT('Ctrl Pts',(-0.694214576672331,0.438610418338741,
-5.86238433632284));
#60915=CARTESIAN_POINT('Ctrl Pts',(-0.531017389080286,0.586395551223196,
-5.87124307989612));
#60916=CARTESIAN_POINT('Ctrl Pts',(-0.367820201488242,0.734180684107651,
-5.88010182346939));
#60917=CARTESIAN_POINT('Ctrl Pts',(-0.14086817587171,0.808992666571339,
-5.88896056704266));
#60918=CARTESIAN_POINT('Ctrl Pts',(0.0782205473247859,0.787223447298295,
-5.89781931061593));
#60919=CARTESIAN_POINT('Ctrl Pts',(0.297309270521282,0.76545422802525,-5.9066780541892));
#60920=CARTESIAN_POINT('Ctrl Pts',(0.505102072675597,0.647444880834226,
-5.91553679776248));
#60921=CARTESIAN_POINT('Ctrl Pts',(0.636026795761728,0.470435038100979,
-5.92439554133575));
#60922=CARTESIAN_POINT('Ctrl Pts',(0.766951518847859,0.293425195367732,
-5.93325428490902));
#60923=CARTESIAN_POINT('Ctrl Pts',(0.818956872247065,0.0601881960099587,
-5.94211302848229));
#60924=CARTESIAN_POINT('Ctrl Pts',(0.775631781004217,-0.155674501111215,
-5.95097177205556));
#60925=CARTESIAN_POINT('Ctrl Pts',(0.73230668976137,-0.37153719823239,-5.95983051562884));
#60926=CARTESIAN_POINT('Ctrl Pts',(0.594329958850255,-0.56664351893645,
-5.96868925920211));
#60927=CARTESIAN_POINT('Ctrl Pts',(0.405242230244101,-0.679424716084709,
-5.97754800277538));
#60928=CARTESIAN_POINT('Ctrl Pts',(0.216154501637947,-0.792205913232967,
-5.98640674634865));
#60929=CARTESIAN_POINT('Ctrl Pts',(-0.0210816529299185,-0.820894963713002,
-5.99526548992193));
#60930=CARTESIAN_POINT('Ctrl Pts',(-0.231602780753117,-0.756438604215453,
-6.0041242334952));
#60931=CARTESIAN_POINT('Ctrl Pts',(-0.442123908576316,-0.691982244717905,
-6.01298297706847));
#60932=CARTESIAN_POINT('Ctrl Pts',(-0.622631625634084,-0.535390358803637,
-6.02184172064174));
#60933=CARTESIAN_POINT('Ctrl Pts',(-0.716163994722094,-0.336077881842427,
-6.03070046421501));
#60934=CARTESIAN_POINT('Ctrl Pts',(-0.765317280859475,-0.231334857514603,
-6.03535592586878));
#60935=CARTESIAN_POINT('Ctrl Pts',(-0.791100000000011,-0.115702837836522,
-6.04001138752254));
#60936=CARTESIAN_POINT('Ctrl Pts',(-0.7911,7.60502771868232E-14,-6.0446668491763));
#60937=CARTESIAN_POINT('Ctrl Pts',(-0.790931871961626,-0.000575333837205039,
-6.07313315082367));
#60938=CARTESIAN_POINT('Ctrl Pts',(-0.791351853183058,-0.0876930044934924,
-6.06963268523682));
#60939=CARTESIAN_POINT('Ctrl Pts',(-0.777675796400345,-0.174599197422119,
-6.06613221964997));
#60940=CARTESIAN_POINT('Ctrl Pts',(-0.749405440614064,-0.256493573493322,
-6.06263175406311));
#60941=CARTESIAN_POINT('Ctrl Pts',(-0.663870191939938,-0.504274530875614,
-6.05204068840018));
#60942=CARTESIAN_POINT('Ctrl Pts',(-0.444733565754056,-0.706175543231099,
-6.04144962273725));
#60943=CARTESIAN_POINT('Ctrl Pts',(-0.190625871903937,-0.769230819079553,
-6.03085855707432));
#60944=CARTESIAN_POINT('Ctrl Pts',(0.063481821946182,-0.832286094928007,
-6.02026749141139));
#60945=CARTESIAN_POINT('Ctrl Pts',(0.352560583460537,-0.75649563426943,
-6.00967642574847));
#60946=CARTESIAN_POINT('Ctrl Pts',(0.543404894746757,-0.576797729800151,
-5.99908536008554));
#60947=CARTESIAN_POINT('Ctrl Pts',(0.734249206032977,-0.397099825330873,
-5.98849429442261));
#60948=CARTESIAN_POINT('Ctrl Pts',(0.826859067091062,-0.113494477050894,
-5.97790322875968));
#60949=CARTESIAN_POINT('Ctrl Pts',(0.779142391420507,0.144110508626454,
-5.96731216309675));
#60950=CARTESIAN_POINT('Ctrl Pts',(0.731425715749952,0.401715494303803,
-5.95672109743382));
#60951=CARTESIAN_POINT('Ctrl Pts',(0.543382503350756,0.633320117378521,
-5.94613003177089));
#60952=CARTESIAN_POINT('Ctrl Pts',(0.301070755401524,0.732930491279356,
-5.93553896610796));
#60953=CARTESIAN_POINT('Ctrl Pts',(0.0587590074522929,0.83254086518019,
-5.92494790044503));
#60954=CARTESIAN_POINT('Ctrl Pts',(-0.237821276046974,0.800156989907141,
-5.9143568347821));
#60955=CARTESIAN_POINT('Ctrl Pts',(-0.452886511529511,0.650290941357769,
-5.90376576911917));
#60956=CARTESIAN_POINT('Ctrl Pts',(-0.660231440322552,0.50580471095775,
-5.89355489635401));
#60957=CARTESIAN_POINT('Ctrl Pts',(-0.791808652946734,0.252119551325989,
-5.88334402358884));
#60958=CARTESIAN_POINT('Ctrl Pts',(-0.792458596363369,-0.000371319283420802,
-5.87313315082368));
#60959=CARTESIAN_POINT('Origin',(0.,0.,-5.925));
#60960=CARTESIAN_POINT('',(-0.7911,1.10300657496509E-13,-5.6446668491763));
#60961=CARTESIAN_POINT('',(-0.790982034689833,0.00049980459233876,-5.67313315082368));
#60962=CARTESIAN_POINT('',(-0.7911,-9.68818082805471E-17,-5.925));
#60963=CARTESIAN_POINT('Ctrl Pts',(-0.7911,1.10300657496509E-13,-5.6446668491763));
#60964=CARTESIAN_POINT('Ctrl Pts',(-0.791099999999969,0.22016758966679,
-5.65352559274957));
#60965=CARTESIAN_POINT('Ctrl Pts',(-0.694214576672307,0.438610418338786,
-5.66238433632285));
#60966=CARTESIAN_POINT('Ctrl Pts',(-0.53101738908024,0.586395551223237,
-5.67124307989612));
#60967=CARTESIAN_POINT('Ctrl Pts',(-0.367820201488173,0.734180684107689,
-5.68010182346939));
#60968=CARTESIAN_POINT('Ctrl Pts',(-0.140868175871616,0.808992666571359,
-5.68896056704266));
#60969=CARTESIAN_POINT('Ctrl Pts',(0.0782205473248925,0.787223447298284,
-5.69781931061594));
#60970=CARTESIAN_POINT('Ctrl Pts',(0.297309270521401,0.765454228025208,
-5.70667805418921));
#60971=CARTESIAN_POINT('Ctrl Pts',(0.505102072675713,0.647444880834141,
-5.71553679776248));
#60972=CARTESIAN_POINT('Ctrl Pts',(0.636026795761818,0.470435038100856,
-5.72439554133575));
#60973=CARTESIAN_POINT('Ctrl Pts',(0.766951518847924,0.293425195367572,
-5.73325428490903));
#60974=CARTESIAN_POINT('Ctrl Pts',(0.818956872247083,0.0601881960097696,
-5.7421130284823));
#60975=CARTESIAN_POINT('Ctrl Pts',(0.775631781004179,-0.155674501111408,
-5.75097177205557));
#60976=CARTESIAN_POINT('Ctrl Pts',(0.732306689761274,-0.371537198232586,
-5.75983051562884));
#60977=CARTESIAN_POINT('Ctrl Pts',(0.594329958850094,-0.566643518936625,
-5.76868925920212));
#60978=CARTESIAN_POINT('Ctrl Pts',(0.405242230243893,-0.679424716084833,
-5.77754800277539));
#60979=CARTESIAN_POINT('Ctrl Pts',(0.216154501637692,-0.792205913233041,
-5.78640674634866));
#60980=CARTESIAN_POINT('Ctrl Pts',(-0.0210816529302019,-0.820894963712999,
-5.79526548992194));
#60981=CARTESIAN_POINT('Ctrl Pts',(-0.231602780753392,-0.756438604215369,
-5.80412423349521));
#60982=CARTESIAN_POINT('Ctrl Pts',(-0.442123908576581,-0.69198224471774,
-5.81298297706848));
#60983=CARTESIAN_POINT('Ctrl Pts',(-0.622631625634302,-0.535390358803389,
-5.82184172064175));
#60984=CARTESIAN_POINT('Ctrl Pts',(-0.716163994722235,-0.336077881842126,
-5.83070046421503));
#60985=CARTESIAN_POINT('Ctrl Pts',(-0.765317280859527,-0.231334857514377,
-5.83535592586878));
#60986=CARTESIAN_POINT('Ctrl Pts',(-0.791100000000014,-0.1157028378364,
-5.84001138752254));
#60987=CARTESIAN_POINT('Ctrl Pts',(-0.7911,9.31477117660506E-14,-5.8446668491763));
#60988=CARTESIAN_POINT('Ctrl Pts',(-0.792458596363369,-0.000371319283420802,
-5.87313315082368));
#60989=CARTESIAN_POINT('Ctrl Pts',(-0.792482796436823,-0.00977259554683975,
-5.87275295792591));
#60990=CARTESIAN_POINT('Ctrl Pts',(-0.792325481568797,-0.0191722160718984,
-5.87237276502815));
#60991=CARTESIAN_POINT('Ctrl Pts',(-0.791983804387725,-0.0285644822897483,
-5.87199257213039));
#60992=CARTESIAN_POINT('Ctrl Pts',(-0.782465674297599,-0.290205635562192,
-5.86140150646746));
#60993=CARTESIAN_POINT('Ctrl Pts',(-0.629879226651533,-0.546139720281407,
-5.85081044080453));
#60994=CARTESIAN_POINT('Ctrl Pts',(-0.404949836955553,-0.680744516845347,
-5.8402193751416));
#60995=CARTESIAN_POINT('Ctrl Pts',(-0.292485142107553,-0.748046915127322,
-5.83492384231014));
#60996=CARTESIAN_POINT('Ctrl Pts',(-0.161934711747093,-0.785016991370474,
-5.82962830947867));
#60997=CARTESIAN_POINT('Ctrl Pts',(-0.0299182311690132,-0.789929417398865,
-5.82433277664721));
#60998=CARTESIAN_POINT('Ctrl Pts',(0.102098249409059,-0.794841843427256,
-5.81903724381574));
#60999=CARTESIAN_POINT('Ctrl Pts',(0.235580780204725,-0.767696619240881,
-5.81374171098428));
#61000=CARTESIAN_POINT('Ctrl Pts',(0.352873959307637,-0.709126006920355,
-5.80844617815281));
#61001=CARTESIAN_POINT('Ctrl Pts',(0.587460317513463,-0.591984782279301,
-5.79785511248988));
#61002=CARTESIAN_POINT('Ctrl Pts',(0.757289268948261,-0.349142005101648,
-5.78726404682695));
#61003=CARTESIAN_POINT('Ctrl Pts',(0.787149237372238,-0.0881671752330585,
-5.77667298116402));
#61004=CARTESIAN_POINT('Ctrl Pts',(0.802079221584226,0.0423202397012362,
-5.77137744833256));
#61005=CARTESIAN_POINT('Ctrl Pts',(0.782016960043503,0.177340667808283,
-5.7660819155011));
#61006=CARTESIAN_POINT('Ctrl Pts',(0.731916162847515,0.29939589036256,-5.76078638266963));
#61007=CARTESIAN_POINT('Ctrl Pts',(0.68181536565153,0.42145111291683,-5.75549084983817));
#61008=CARTESIAN_POINT('Ctrl Pts',(0.601676032800284,0.530541129918351,
-5.7501953170067));
#61009=CARTESIAN_POINT('Ctrl Pts',(0.499973647650632,0.613383996655761,
-5.74489978417524));
#61010=CARTESIAN_POINT('Ctrl Pts',(0.398271262500969,0.69622686339318,-5.73960425134377));
#61011=CARTESIAN_POINT('Ctrl Pts',(0.2750058250529,0.752822579866479,-5.73430871851231));
#61012=CARTESIAN_POINT('Ctrl Pts',(0.145408139388317,0.777300086642441,
-5.72901318568084));
#61013=CARTESIAN_POINT('Ctrl Pts',(0.0158104537237486,0.8017775934184,-5.72371765284938));
#61014=CARTESIAN_POINT('Ctrl Pts',(-0.120119480157327,0.794136890497028,
-5.71842212001791));
#61015=CARTESIAN_POINT('Ctrl Pts',(-0.244883133276068,0.753158437135428,
-5.71312658718645));
#61016=CARTESIAN_POINT('Ctrl Pts',(-0.49441043951357,0.67120153041222,-5.70253552152352));
#61017=CARTESIAN_POINT('Ctrl Pts',(-0.699272622701712,0.455893621928078,
-5.69194445586059));
#61018=CARTESIAN_POINT('Ctrl Pts',(-0.766117078544422,0.202773826096619,
-5.68135339019766));
#61019=CARTESIAN_POINT('Ctrl Pts',(-0.783410819178852,0.137287645629397,
-5.67861331040633));
#61020=CARTESIAN_POINT('Ctrl Pts',(-0.791466474469695,0.0692705624365982,
-5.67587323061501));
#61021=CARTESIAN_POINT('Ctrl Pts',(-0.79084825614368,0.00106660793215366,
-5.67313315082368));
#61022=CARTESIAN_POINT('Origin',(0.,0.,-5.925));
#61023=CARTESIAN_POINT('',(-0.790955350306868,1.92250298529111E-5,-5.4446668491763));
#61024=CARTESIAN_POINT('',(-0.79043867098578,-0.000255047988537571,-5.47313315082368));
#61025=CARTESIAN_POINT('',(-0.7911,-9.68818082805471E-17,-5.925));
#61026=CARTESIAN_POINT('Ctrl Pts',(-0.7911,1.27342580924505E-13,-5.4446668491763));
#61027=CARTESIAN_POINT('Ctrl Pts',(-0.791099999999964,0.220167589666792,
-5.45352559274957));
#61028=CARTESIAN_POINT('Ctrl Pts',(-0.694214576672312,0.438610418338771,
-5.46238433632285));
#61029=CARTESIAN_POINT('Ctrl Pts',(-0.531017389080261,0.586395551223219,
-5.47124307989612));
#61030=CARTESIAN_POINT('Ctrl Pts',(-0.36782020148821,0.734180684107666,
-5.48010182346939));
#61031=CARTESIAN_POINT('Ctrl Pts',(-0.140868175871675,0.808992666571345,
-5.48896056704266));
#61032=CARTESIAN_POINT('Ctrl Pts',(0.0782205473248199,0.787223447298291,
-5.49781931061593));
#61033=CARTESIAN_POINT('Ctrl Pts',(0.297309270521315,0.765454228025237,
-5.50667805418921));
#61034=CARTESIAN_POINT('Ctrl Pts',(0.505102072675625,0.647444880834204,
-5.51553679776248));
#61035=CARTESIAN_POINT('Ctrl Pts',(0.636026795761748,0.470435038100951,
-5.52439554133575));
#61036=CARTESIAN_POINT('Ctrl Pts',(0.766951518847871,0.293425195367699,
-5.53325428490902));
#61037=CARTESIAN_POINT('Ctrl Pts',(0.818956872247068,0.0601881960099234,
-5.54211302848229));
#61038=CARTESIAN_POINT('Ctrl Pts',(0.775631781004211,-0.155674501111249,
-5.55097177205557));
#61039=CARTESIAN_POINT('Ctrl Pts',(0.732306689761354,-0.371537198232421,
-5.55983051562884));
#61040=CARTESIAN_POINT('Ctrl Pts',(0.59432995885023,-0.566643518936476,
-5.56868925920211));
#61041=CARTESIAN_POINT('Ctrl Pts',(0.405242230244071,-0.679424716084726,
-5.57754800277538));
#61042=CARTESIAN_POINT('Ctrl Pts',(0.216154501637913,-0.792205913232977,
-5.58640674634866));
#61043=CARTESIAN_POINT('Ctrl Pts',(-0.021081652929954,-0.820894963713001,
-5.59526548992193));
#61044=CARTESIAN_POINT('Ctrl Pts',(-0.23160278075315,-0.756438604215443,
-5.6041242334952));
#61045=CARTESIAN_POINT('Ctrl Pts',(-0.442123908576346,-0.691982244717885,
-5.61298297706847));
#61046=CARTESIAN_POINT('Ctrl Pts',(-0.622631625634107,-0.53539035880361,
-5.62184172064174));
#61047=CARTESIAN_POINT('Ctrl Pts',(-0.716163994722109,-0.336077881842396,
-5.63070046421501));
#61048=CARTESIAN_POINT('Ctrl Pts',(-0.765317280859485,-0.23133485751457,
-5.63535592586878));
#61049=CARTESIAN_POINT('Ctrl Pts',(-0.791100000000016,-0.115702837836488,
-5.64001138752254));
#61050=CARTESIAN_POINT('Ctrl Pts',(-0.7911,1.10300657496509E-13,-5.6446668491763));
#61051=CARTESIAN_POINT('Ctrl Pts',(-0.7911,-4.56634730028327E-13,-5.67313315082368));
#61052=CARTESIAN_POINT('Ctrl Pts',(-0.791099999999873,-0.220167589667121,
-5.6642744072504));
#61053=CARTESIAN_POINT('Ctrl Pts',(-0.694214576672129,-0.43861041833906,
-5.65541566367713));
#61054=CARTESIAN_POINT('Ctrl Pts',(-0.531017389080017,-0.58639555122344,
-5.64655692010386));
#61055=CARTESIAN_POINT('Ctrl Pts',(-0.367820201487905,-0.73418068410782,
-5.63769817653059));
#61056=CARTESIAN_POINT('Ctrl Pts',(-0.140868175871339,-0.808992666571404,
-5.62883943295732));
#61057=CARTESIAN_POINT('Ctrl Pts',(0.0782205473251476,-0.787223447298259,
-5.61998068938404));
#61058=CARTESIAN_POINT('Ctrl Pts',(0.297309270521634,-0.765454228025114,
-5.61112194581077));
#61059=CARTESIAN_POINT('Ctrl Pts',(0.505102072675895,-0.647444880833994,
-5.6022632022375));
#61060=CARTESIAN_POINT('Ctrl Pts',(0.636026795761944,-0.470435038100687,
-5.59340445866423));
#61061=CARTESIAN_POINT('Ctrl Pts',(0.766951518847994,-0.293425195367379,
-5.58454571509096));
#61062=CARTESIAN_POINT('Ctrl Pts',(0.818956872247093,-0.0601881960095824,
-5.57568697151768));
#61063=CARTESIAN_POINT('Ctrl Pts',(0.775631781004146,0.155674501111572,
-5.56682822794441));
#61064=CARTESIAN_POINT('Ctrl Pts',(0.732306689761199,0.371537198232726,
-5.55796948437114));
#61065=CARTESIAN_POINT('Ctrl Pts',(0.594329958849994,0.566643518936724,
-5.54911074079787));
#61066=CARTESIAN_POINT('Ctrl Pts',(0.405242230243789,0.679424716084895,
-5.5402519972246));
#61067=CARTESIAN_POINT('Ctrl Pts',(0.216154501637583,0.792205913233067,
-5.53139325365132));
#61068=CARTESIAN_POINT('Ctrl Pts',(-0.0210816529302957,0.820894963712993,
-5.52253451007805));
#61069=CARTESIAN_POINT('Ctrl Pts',(-0.231602780753465,0.756438604215347,
-5.51367576650478));
#61070=CARTESIAN_POINT('Ctrl Pts',(-0.442123908576634,0.691982244717702,
-5.50481702293151));
#61071=CARTESIAN_POINT('Ctrl Pts',(-0.62263162563433,0.535390358803351,
-5.49595827935824));
#61072=CARTESIAN_POINT('Ctrl Pts',(-0.716163994722249,0.336077881842098,
-5.48709953578496));
#61073=CARTESIAN_POINT('Ctrl Pts',(-0.765317280859578,0.231334857514259,
-5.4824440741312));
#61074=CARTESIAN_POINT('Ctrl Pts',(-0.791100000000061,0.115702837836174,
-5.47778861247744));
#61075=CARTESIAN_POINT('Ctrl Pts',(-0.7911,-4.17166301502903E-13,-5.47313315082368));
#61076=CARTESIAN_POINT('Origin',(0.,0.,-5.925));
#61077=CARTESIAN_POINT('',(-0.790920704737585,-0.000653246164056709,-5.2446668491763));
#61078=CARTESIAN_POINT('',(-0.79181808259713,-0.000281894939852955,-5.27313315082368));
#61079=CARTESIAN_POINT('',(-0.7911,-9.68818082805471E-17,-5.925));
#61080=CARTESIAN_POINT('Ctrl Pts',(-0.790920704737585,-0.000653246164056709,
-5.2446668491763));
#61081=CARTESIAN_POINT('Ctrl Pts',(-0.788945460378493,0.215598739194996,
-5.25337933483792));
#61082=CARTESIAN_POINT('Ctrl Pts',(-0.697988167637598,0.433127810576575,
-5.26209182049953));
#61083=CARTESIAN_POINT('Ctrl Pts',(-0.540326790654243,0.579951476740454,
-5.27080430616114));
#61084=CARTESIAN_POINT('Ctrl Pts',(-0.348670578983709,0.758433158043535,
-5.28139537182407));
#61085=CARTESIAN_POINT('Ctrl Pts',(-0.0584437231446916,0.832431322067987,
-5.291986437487));
#61086=CARTESIAN_POINT('Ctrl Pts',(0.195313604932554,0.768052485885201,
-5.30257750314993));
#61087=CARTESIAN_POINT('Ctrl Pts',(0.449070933009777,0.703673649702421,
-5.31316856881286));
#61088=CARTESIAN_POINT('Ctrl Pts',(0.666358733325236,0.50091781331243,-5.32375963447579));
#61089=CARTESIAN_POINT('Ctrl Pts',(0.750740772904286,0.252196997301994,
-5.33435070013872));
#61090=CARTESIAN_POINT('Ctrl Pts',(0.792931792693813,0.127836589296773,
-5.33964623297019));
#61091=CARTESIAN_POINT('Ctrl Pts',(0.801896372299235,-0.00801506361356036,
-5.34494176580165));
#61092=CARTESIAN_POINT('Ctrl Pts',(0.778678837782813,-0.13784288282515,
-5.35023729863311));
#61093=CARTESIAN_POINT('Ctrl Pts',(0.755461303266393,-0.267670702036732,
-5.35553283146458));
#61094=CARTESIAN_POINT('Ctrl Pts',(0.700061654628132,-0.391474687549571,
-5.36082836429603));
#61095=CARTESIAN_POINT('Ctrl Pts',(0.618214469457432,-0.49398089165876,
-5.3661238971275));
#61096=CARTESIAN_POINT('Ctrl Pts',(0.536367284286727,-0.596487095767956,
-5.37141942995896));
#61097=CARTESIAN_POINT('Ctrl Pts',(0.428072562583579,-0.677695518473499,
-5.37671496279044));
#61098=CARTESIAN_POINT('Ctrl Pts',(0.306507155037109,-0.72897744547975,
-5.3820104956219));
#61099=CARTESIAN_POINT('Ctrl Pts',(0.184941747490638,-0.780259372486002,
-5.38730602845337));
#61100=CARTESIAN_POINT('Ctrl Pts',(0.0501056541008438,-0.80161480379296,
-5.39260156128483));
#61101=CARTESIAN_POINT('Ctrl Pts',(-0.0805206321447689,-0.787954795419253,
-5.39789709411629));
#61102=CARTESIAN_POINT('Ctrl Pts',(-0.341773204635994,-0.760634778671838,
-5.40848815977922));
#61103=CARTESIAN_POINT('Ctrl Pts',(-0.586186548550494,-0.59325300320176,
-5.41907922544215));
#61104=CARTESIAN_POINT('Ctrl Pts',(-0.70564674271158,-0.359769324320271,
-5.42967029110508));
#61105=CARTESIAN_POINT('Ctrl Pts',(-0.762030484629915,-0.249567900451454,
-5.43466914379549));
#61106=CARTESIAN_POINT('Ctrl Pts',(-0.790578115231393,-0.124640797836264,
-5.43966799648589));
#61107=CARTESIAN_POINT('Ctrl Pts',(-0.790531284472335,7.55865616196768E-5,
-5.4446668491763));
#61108=CARTESIAN_POINT('Ctrl Pts',(-0.789707734786939,-0.000536940665675214,
-5.47313315082368));
#61109=CARTESIAN_POINT('Ctrl Pts',(-0.79018851931201,-0.118315462065016,
-5.46840243764117));
#61110=CARTESIAN_POINT('Ctrl Pts',(-0.765626792726158,-0.235892771010167,
-5.46367172445866));
#61111=CARTESIAN_POINT('Ctrl Pts',(-0.715193436764779,-0.341394750524073,
-5.45894101127615));
#61112=CARTESIAN_POINT('Ctrl Pts',(-0.602283825891805,-0.57759135545288,
-5.44834994561322));
#61113=CARTESIAN_POINT('Ctrl Pts',(-0.359701123138071,-0.753264315732189,
-5.43775887995029));
#61114=CARTESIAN_POINT('Ctrl Pts',(-0.0999042190561839,-0.786330656795897,
-5.42716781428736));
#61115=CARTESIAN_POINT('Ctrl Pts',(0.159892685025703,-0.819396997859606,
-5.41657674862443));
#61116=CARTESIAN_POINT('Ctrl Pts',(0.436903790435752,-0.709856719707715,
-5.40598568296151));
#61117=CARTESIAN_POINT('Ctrl Pts',(0.606154956204237,-0.509701287988473,
-5.39539461729858));
#61118=CARTESIAN_POINT('Ctrl Pts',(0.690780539088484,-0.409623572128847,
-5.39009908446711));
#61119=CARTESIAN_POINT('Ctrl Pts',(0.74846613706234,-0.286892067877377,
-5.38480355163564));
#61120=CARTESIAN_POINT('Ctrl Pts',(0.774698971576816,-0.157436828890488,
-5.37950801880418));
#61121=CARTESIAN_POINT('Ctrl Pts',(0.800931806091292,-0.0279815899036063,
-5.37421248597271));
#61122=CARTESIAN_POINT('Ctrl Pts',(0.795711877146396,0.108197383818677,
-5.36891695314125));
#61123=CARTESIAN_POINT('Ctrl Pts',(0.756882813203795,0.233451706564843,
-5.36362142030979));
#61124=CARTESIAN_POINT('Ctrl Pts',(0.679224685318594,0.483960352057175,
-5.35303035464686));
#61125=CARTESIAN_POINT('Ctrl Pts',(0.467130017442567,0.690770393644964,
-5.34243928898393));
#61126=CARTESIAN_POINT('Ctrl Pts',(0.214430568118855,0.762480074022537,
-5.331848223321));
#61127=CARTESIAN_POINT('Ctrl Pts',(0.0880808434569991,0.798334914211325,
-5.32655269048953));
#61128=CARTESIAN_POINT('Ctrl Pts',(-0.0484200765667811,0.800414664097558,
-5.32125715765807));
#61129=CARTESIAN_POINT('Ctrl Pts',(-0.176978016792099,0.770735709357923,
-5.31596162482661));
#61130=CARTESIAN_POINT('Ctrl Pts',(-0.305535957017418,0.741056754618287,
-5.31066609199514));
#61131=CARTESIAN_POINT('Ctrl Pts',(-0.426150917444278,0.679619095252781,
-5.30537055916368));
#61132=CARTESIAN_POINT('Ctrl Pts',(-0.52436170595682,0.592664367831045,
-5.30007502633221));
#61133=CARTESIAN_POINT('Ctrl Pts',(-0.62257249446936,0.505709640409309,
-5.29477949350075));
#61134=CARTESIAN_POINT('Ctrl Pts',(-0.698379111067585,0.39323784493134,
-5.28948396066928));
#61135=CARTESIAN_POINT('Ctrl Pts',(-0.743513036798558,0.26931349180263,
-5.28418842783782));
#61136=CARTESIAN_POINT('Ctrl Pts',(-0.774921147972737,0.18307614822532,
-5.28050333549977));
#61137=CARTESIAN_POINT('Ctrl Pts',(-0.791475742174448,0.0912928041298384,
-5.27681824316172));
#61138=CARTESIAN_POINT('Ctrl Pts',(-0.79181808259713,-0.000281894939852955,
-5.27313315082368));
#61139=CARTESIAN_POINT('Origin',(0.,0.,-5.925));
#61140=CARTESIAN_POINT('',(-0.792204594358573,0.000315518470781081,-5.0446668491763));
#61141=CARTESIAN_POINT('',(-0.791078014336539,0.000374052597120995,-5.07313315082368));
#61142=CARTESIAN_POINT('',(-0.7911,-9.68818082805471E-17,-5.925));
#61143=CARTESIAN_POINT('Ctrl Pts',(-0.792204594358573,0.000315518470781081,
-5.0446668491763));
#61144=CARTESIAN_POINT('Ctrl Pts',(-0.79246329697991,0.0310447806827188,
-5.04590854186408));
#61145=CARTESIAN_POINT('Ctrl Pts',(-0.790845381848934,0.0617570747404931,
-5.04715023455185));
#61146=CARTESIAN_POINT('Ctrl Pts',(-0.787265111314072,0.0922518323957158,
-5.04839192723963));
#61147=CARTESIAN_POINT('Ctrl Pts',(-0.756727055723453,0.352358043764337,
-5.05898299290256));
#61148=CARTESIAN_POINT('Ctrl Pts',(-0.583421702319185,0.596637823128375,
-5.06957405856549));
#61149=CARTESIAN_POINT('Ctrl Pts',(-0.348334401689638,0.711839286595329,
-5.08016512422842));
#61150=CARTESIAN_POINT('Ctrl Pts',(-0.113247101060097,0.827040750062279,
-5.09075618989135));
#61151=CARTESIAN_POINT('Ctrl Pts',(0.183622146794714,0.813163897632151,
-5.10134725555427));
#61152=CARTESIAN_POINT('Ctrl Pts',(0.408947385305092,0.678216093590518,
-5.1119383212172));
#61153=CARTESIAN_POINT('Ctrl Pts',(0.521610004560291,0.610742191569696,
-5.11723385404867));
#61154=CARTESIAN_POINT('Ctrl Pts',(0.616386621479376,0.513000551645993,
-5.12252938688014));
#61155=CARTESIAN_POINT('Ctrl Pts',(0.682734783222974,0.399017052926018,
-5.1278249197116));
#61156=CARTESIAN_POINT('Ctrl Pts',(0.749082944966569,0.285033554206049,
-5.13312045254307));
#61157=CARTESIAN_POINT('Ctrl Pts',(0.787002651534682,0.154808196689791,
-5.13841598537453));
#61158=CARTESIAN_POINT('Ctrl Pts',(0.790977118250049,0.0236949356473377,
-5.14371151820599));
#61159=CARTESIAN_POINT('Ctrl Pts',(0.794951584965415,-0.107418325395108,
-5.14900705103746));
#61160=CARTESIAN_POINT('Ctrl Pts',(0.764980811828053,-0.239419489963747,
-5.15430258386892));
#61161=CARTESIAN_POINT('Ctrl Pts',(0.705522254309981,-0.357201764866207,
-5.15959811670039));
#61162=CARTESIAN_POINT('Ctrl Pts',(0.646063696791902,-0.47498403976868,
-5.16489364953185));
#61163=CARTESIAN_POINT('Ctrl Pts',(0.557117354893093,-0.578547425004965,
-5.17018918236332));
#61164=CARTESIAN_POINT('Ctrl Pts',(0.448712359625208,-0.652697134972368,
-5.17548471519478));
#61165=CARTESIAN_POINT('Ctrl Pts',(0.231902369089455,-0.800996554907163,
-5.18607578085771));
#61166=CARTESIAN_POINT('Ctrl Pts',(-0.062742234922631,-0.831641273766528,
-5.19666684652064));
#61167=CARTESIAN_POINT('Ctrl Pts',(-0.304939923081079,-0.7310150037407,
-5.20725791218357));
#61168=CARTESIAN_POINT('Ctrl Pts',(-0.426038767160313,-0.680701868727781,
-5.21255344501503));
#61169=CARTESIAN_POINT('Ctrl Pts',(-0.534025882276133,-0.597570986493561,
-5.2178489778465));
#61170=CARTESIAN_POINT('Ctrl Pts',(-0.616719234357281,-0.494572782648415,
-5.22314451067796));
#61171=CARTESIAN_POINT('Ctrl Pts',(-0.69941258643842,-0.391574578803282,
-5.22844004350943));
#61172=CARTESIAN_POINT('Ctrl Pts',(-0.756812175484892,-0.268709053347231,
-5.23373557634089));
#61173=CARTESIAN_POINT('Ctrl Pts',(-0.779564306932199,-0.139637836612918,
-5.23903110917236));
#61174=CARTESIAN_POINT('Ctrl Pts',(-0.787635581435542,-0.0938500728090807,
-5.24090968917367));
#61175=CARTESIAN_POINT('Ctrl Pts',(-0.791346605530403,-0.0472813464236894,
-5.24278826917499));
#61176=CARTESIAN_POINT('Ctrl Pts',(-0.790920704737585,-0.000653246164056709,
-5.2446668491763));
#61177=CARTESIAN_POINT('Ctrl Pts',(-0.79181808259713,-0.000281894939852955,
-5.27313315082368));
#61178=CARTESIAN_POINT('Ctrl Pts',(-0.791967690484436,-0.0403014087066727,
-5.27152271033026));
#61179=CARTESIAN_POINT('Ctrl Pts',(-0.789021048451441,-0.0802810750128665,
-5.26991226983684));
#61180=CARTESIAN_POINT('Ctrl Pts',(-0.782864753571529,-0.119740599482619,
-5.26830182934342));
#61181=CARTESIAN_POINT('Ctrl Pts',(-0.742377865928075,-0.379246254236745,
-5.25771076368049));
#61182=CARTESIAN_POINT('Ctrl Pts',(-0.563072263542853,-0.616255575381294,
-5.24711969801757));
#61183=CARTESIAN_POINT('Ctrl Pts',(-0.324111150269872,-0.72319014623882,
-5.23652863235464));
#61184=CARTESIAN_POINT('Ctrl Pts',(-0.0851500369968912,-0.830124717096347,
-5.22593756669171));
#61185=CARTESIAN_POINT('Ctrl Pts',(0.213466587163831,-0.806984537666828,
-5.21534650102878));
#61186=CARTESIAN_POINT('Ctrl Pts',(0.43288697747365,-0.664007244543216,
-5.20475543536585));
#61187=CARTESIAN_POINT('Ctrl Pts',(0.652307367783463,-0.52102995141961,
-5.19416436970292));
#61188=CARTESIAN_POINT('Ctrl Pts',(0.792531524242369,-0.25821554460192,
-5.18357330403999));
#61189=CARTESIAN_POINT('Ctrl Pts',(0.791962104743775,0.00390623942245968,
-5.17298223837706));
#61190=CARTESIAN_POINT('Ctrl Pts',(0.791677394994479,0.134967131434653,
-5.1676867055456));
#61191=CARTESIAN_POINT('Ctrl Pts',(0.756194291255797,0.26585486774854,-5.16239117271413));
#61192=CARTESIAN_POINT('Ctrl Pts',(0.692385554167272,0.381506350855799,
-5.15709563988267));
#61193=CARTESIAN_POINT('Ctrl Pts',(0.628576817078747,0.497157833963058,
-5.1518001070512));
#61194=CARTESIAN_POINT('Ctrl Pts',(0.536442446640378,0.597573063863706,
-5.14650457421974));
#61195=CARTESIAN_POINT('Ctrl Pts',(0.425763601408166,0.667904669918289,
-5.14120904138828));
#61196=CARTESIAN_POINT('Ctrl Pts',(0.204405910943742,0.808567882027454,
-5.13061797572535));
#61197=CARTESIAN_POINT('Ctrl Pts',(-0.0911296786960406,0.828896598752346,
-5.12002691006241));
#61198=CARTESIAN_POINT('Ctrl Pts',(-0.330156313607016,0.719967457783326,
-5.10943584439948));
#61199=CARTESIAN_POINT('Ctrl Pts',(-0.449669631062504,0.665502887298816,
-5.10414031156802));
#61200=CARTESIAN_POINT('Ctrl Pts',(-0.555055709835787,0.578723852390829,
-5.09884477873656));
#61201=CARTESIAN_POINT('Ctrl Pts',(-0.633828647979511,0.47288053158344,
-5.0935492459051));
#61202=CARTESIAN_POINT('Ctrl Pts',(-0.712601586123234,0.36703721077605,
-5.08825371307363));
#61203=CARTESIAN_POINT('Ctrl Pts',(-0.764761383637394,0.242129604069261,
-5.08295818024217));
#61204=CARTESIAN_POINT('Ctrl Pts',(-0.783326391228992,0.112276517467586,
-5.0776626474107));
#61205=CARTESIAN_POINT('Ctrl Pts',(-0.788619540580868,0.075253544124127,
-5.07615281521503));
#61206=CARTESIAN_POINT('Ctrl Pts',(-0.791181763733698,0.0378285518770546,
-5.07464298301935));
#61207=CARTESIAN_POINT('Ctrl Pts',(-0.791078014336539,0.000374052597120995,
-5.07313315082368));
#61208=CARTESIAN_POINT('Origin',(0.,0.,-5.925));
#61209=CARTESIAN_POINT('',(-0.790607229746229,0.000210778082028613,-4.8446668491763));
#61210=CARTESIAN_POINT('',(-0.7911,-3.88467036316342E-13,-4.87313315082368));
#61211=CARTESIAN_POINT('',(-0.7911,-9.68818082805471E-17,-5.925));
#61212=CARTESIAN_POINT('Ctrl Pts',(-0.789880781196105,0.000521509970750122,
-4.8446668491763));
#61213=CARTESIAN_POINT('Ctrl Pts',(-0.790311297832213,0.109477148114268,
-4.84902881455317));
#61214=CARTESIAN_POINT('Ctrl Pts',(-0.769390262863306,0.218221643359569,
-4.85339077993004));
#61215=CARTESIAN_POINT('Ctrl Pts',(-0.72630816890144,0.317062248033498,
-4.8577527453069));
#61216=CARTESIAN_POINT('Ctrl Pts',(-0.621702733822472,0.557052079180901,
-4.86834381096983));
#61217=CARTESIAN_POINT('Ctrl Pts',(-0.386448505408363,0.738654296591801,
-4.87893487663277));
#61218=CARTESIAN_POINT('Ctrl Pts',(-0.127348890008807,0.781663158762513,
-4.88952594229569));
#61219=CARTESIAN_POINT('Ctrl Pts',(0.00220091769097169,0.803167589847869,
-4.89482147512716));
#61220=CARTESIAN_POINT('Ctrl Pts',(0.137712072137115,0.790023682123179,
-4.90011700795862));
#61221=CARTESIAN_POINT('Ctrl Pts',(0.262069525770256,0.746097149445568,
-4.90541254079008));
#61222=CARTESIAN_POINT('Ctrl Pts',(0.386426979403397,0.702170616767958,
-4.91070807362155));
#61223=CARTESIAN_POINT('Ctrl Pts',(0.499630732223539,0.627461459137427,
-4.91600360645302));
#61224=CARTESIAN_POINT('Ctrl Pts',(0.587536521468257,0.530101016327572,
-4.92129913928448));
#61225=CARTESIAN_POINT('Ctrl Pts',(0.675442310712974,0.432740573517717,
-4.92659467211595));
#61226=CARTESIAN_POINT('Ctrl Pts',(0.738050136382271,0.312728845528534,
-4.93189020494741));
#61227=CARTESIAN_POINT('Ctrl Pts',(0.768978010925335,0.184465635996092,
-4.93718573777887));
#61228=CARTESIAN_POINT('Ctrl Pts',(0.7999058854684,0.0562024264636513,-4.94248127061034));
#61229=CARTESIAN_POINT('Ctrl Pts',(0.799153808885237,-0.0803122646120308,
-4.9477768034418));
#61230=CARTESIAN_POINT('Ctrl Pts',(0.76452951145305,-0.207004728928604,
-4.95307233627327));
#61231=CARTESIAN_POINT('Ctrl Pts',(0.695280916588675,-0.460389657561749,
-4.9636634019362));
#61232=CARTESIAN_POINT('Ctrl Pts',(0.49054343832819,-0.674485679158382,
-4.97425446759912));
#61233=CARTESIAN_POINT('Ctrl Pts',(0.240801924961463,-0.754576520518603,
-4.98484553326205));
#61234=CARTESIAN_POINT('Ctrl Pts',(0.115931168278092,-0.794621941198716,
-4.99014106609352));
#61235=CARTESIAN_POINT('Ctrl Pts',(-0.020190597181845,-0.801166066819722,
-4.99543659892498));
#61236=CARTESIAN_POINT('Ctrl Pts',(-0.149894847527861,-0.776193523579221,
-5.00073213175645));
#61237=CARTESIAN_POINT('Ctrl Pts',(-0.27959909787387,-0.751220980338721,
-5.00602766458791));
#61238=CARTESIAN_POINT('Ctrl Pts',(-0.402885833105963,-0.694731768236716,
-5.01132319741938));
#61239=CARTESIAN_POINT('Ctrl Pts',(-0.503781863631195,-0.611083519606513,
-5.01661873025085));
#61240=CARTESIAN_POINT('Ctrl Pts',(-0.681915896808727,-0.463400802861689,
-5.025968103226));
#61241=CARTESIAN_POINT('Ctrl Pts',(-0.790256682995049,-0.231061646345439,
-5.03531747620115));
#61242=CARTESIAN_POINT('Ctrl Pts',(-0.792204594358573,0.000315518470781081,
-5.0446668491763));
#61243=CARTESIAN_POINT('Ctrl Pts',(-0.791078014336539,0.000374052597120995,
-5.07313315082368));
#61244=CARTESIAN_POINT('Ctrl Pts',(-0.790817876713358,-0.0935380537572494,
-5.06934745018789));
#61245=CARTESIAN_POINT('Ctrl Pts',(-0.773797089544038,-0.187635667286825,
-5.0655617495521));
#61246=CARTESIAN_POINT('Ctrl Pts',(-0.741039549927412,-0.276046695672426,
-5.0617760489163));
#61247=CARTESIAN_POINT('Ctrl Pts',(-0.695217483365202,-0.399718255714205,
-5.05648051608484));
#61248=CARTESIAN_POINT('Ctrl Pts',(-0.618603132571746,-0.512262809301205,
-5.05118498325337));
#61249=CARTESIAN_POINT('Ctrl Pts',(-0.519177958415979,-0.5980545803253,
-5.04588945042191));
#61250=CARTESIAN_POINT('Ctrl Pts',(-0.320327610104445,-0.769638122373489,
-5.03529838475898));
#61251=CARTESIAN_POINT('Ctrl Pts',(-0.030233968343667,-0.834210534170057,
-5.02470731909606));
#61252=CARTESIAN_POINT('Ctrl Pts',(0.221124351197595,-0.761023026358905,
-5.01411625343313));
#61253=CARTESIAN_POINT('Ctrl Pts',(0.472482670738857,-0.687835518547754,
-5.0035251877702));
#61254=CARTESIAN_POINT('Ctrl Pts',(0.685105668060603,-0.476888091128884,
-4.99293412210727));
#61255=CARTESIAN_POINT('Ctrl Pts',(0.759789177345915,-0.225869790057779,
-4.98234305644434));
#61256=CARTESIAN_POINT('Ctrl Pts',(0.834472686631226,0.025148511013326,
-4.97175199078141));
#61257=CARTESIAN_POINT('Ctrl Pts',(0.771216707880102,0.316237685736666,
-4.96116092511847));
#61258=CARTESIAN_POINT('Ctrl Pts',(0.601097529576061,0.515655887192186,
-4.95056985945555));
#61259=CARTESIAN_POINT('Ctrl Pts',(0.51603794042404,0.615364987919945,-4.94527432662408));
#61260=CARTESIAN_POINT('Ctrl Pts',(0.404262551383771,0.692156345330761,
-4.93997879379262));
#61261=CARTESIAN_POINT('Ctrl Pts',(0.280760850166947,0.738998103093141,
-4.93468326096116));
#61262=CARTESIAN_POINT('Ctrl Pts',(0.157259148950123,0.785839860855522,
-4.92938772812969));
#61263=CARTESIAN_POINT('Ctrl Pts',(0.0220311355567532,0.802732018969479,
-4.92409219529823));
#61264=CARTESIAN_POINT('Ctrl Pts',(-0.107856599431224,0.784689904575202,
-4.91879666246676));
#61265=CARTESIAN_POINT('Ctrl Pts',(-0.367632069407185,0.748605675786647,
-4.90820559680383));
#61266=CARTESIAN_POINT('Ctrl Pts',(-0.606046425761481,0.572784356965126,
-4.89761453114091));
#61267=CARTESIAN_POINT('Ctrl Pts',(-0.717714788418723,0.335025094830986,
-4.88702346547798));
#61268=CARTESIAN_POINT('Ctrl Pts',(-0.766532938345096,0.231083682697319,
-4.88239336059321));
#61269=CARTESIAN_POINT('Ctrl Pts',(-0.791127605893187,0.115304794406683,
-4.87776325570845));
#61270=CARTESIAN_POINT('Ctrl Pts',(-0.790871083339374,-0.000158561846635865,
-4.87313315082368));
#61271=CARTESIAN_POINT('Origin',(0.,0.,-5.925));
#61272=CARTESIAN_POINT('',(-0.790948977202054,-0.000261541659524338,-4.6446668491763));
#61273=CARTESIAN_POINT('',(-0.7911,-3.71369601737115E-13,-4.67313315082368));
#61274=CARTESIAN_POINT('',(-0.7911,-9.68818082805471E-17,-5.925));
#61275=CARTESIAN_POINT('Ctrl Pts',(-0.7911,1.95454763485259E-13,-4.6446668491763));
#61276=CARTESIAN_POINT('Ctrl Pts',(-0.791099999999946,0.220167589666875,
-4.65352559274958));
#61277=CARTESIAN_POINT('Ctrl Pts',(-0.69421457667226,0.43861041833886,-4.66238433632285));
#61278=CARTESIAN_POINT('Ctrl Pts',(-0.531017389080177,0.586395551223295,
-4.67124307989612));
#61279=CARTESIAN_POINT('Ctrl Pts',(-0.367820201488094,0.734180684107729,
-4.68010182346939));
#61280=CARTESIAN_POINT('Ctrl Pts',(-0.140868175871529,0.808992666571375,
-4.68896056704267));
#61281=CARTESIAN_POINT('Ctrl Pts',(0.0782205473249772,0.787223447298276,
-4.69781931061594));
#61282=CARTESIAN_POINT('Ctrl Pts',(0.297309270521483,0.765454228025177,
-4.70667805418921));
#61283=CARTESIAN_POINT('Ctrl Pts',(0.505102072675782,0.647444880834086,
-4.71553679776249));
#61284=CARTESIAN_POINT('Ctrl Pts',(0.636026795761869,0.470435038100788,
-4.72439554133576));
#61285=CARTESIAN_POINT('Ctrl Pts',(0.766951518847956,0.29342519536749,-4.73325428490903));
#61286=CARTESIAN_POINT('Ctrl Pts',(0.818956872247089,0.0601881960096812,
-4.7421130284823));
#61287=CARTESIAN_POINT('Ctrl Pts',(0.775631781004162,-0.155674501111492,
-4.75097177205558));
#61288=CARTESIAN_POINT('Ctrl Pts',(0.732306689761234,-0.371537198232665,
-4.75983051562885));
#61289=CARTESIAN_POINT('Ctrl Pts',(0.594329958850033,-0.566643518936689,
-4.76868925920212));
#61290=CARTESIAN_POINT('Ctrl Pts',(0.40524223024382,-0.679424716084876,
-4.77754800277539));
#61291=CARTESIAN_POINT('Ctrl Pts',(0.216154501637606,-0.792205913233064,
-4.78640674634867));
#61292=CARTESIAN_POINT('Ctrl Pts',(-0.0210816529302905,-0.820894963712997,
-4.79526548992194));
#61293=CARTESIAN_POINT('Ctrl Pts',(-0.231602780753473,-0.756438604215344,
-4.80412423349521));
#61294=CARTESIAN_POINT('Ctrl Pts',(-0.442123908576656,-0.691982244717692,
-4.81298297706848));
#61295=CARTESIAN_POINT('Ctrl Pts',(-0.62263162563436,-0.535390358803322,
-4.82184172064176));
#61296=CARTESIAN_POINT('Ctrl Pts',(-0.716163994722272,-0.336077881842049,
-4.83070046421503));
#61297=CARTESIAN_POINT('Ctrl Pts',(-0.765317280859552,-0.231334857514295,
-4.83535592586879));
#61298=CARTESIAN_POINT('Ctrl Pts',(-0.791100000000026,-0.115702837836315,
-4.84001138752255));
#61299=CARTESIAN_POINT('Ctrl Pts',(-0.7911,1.78468351208494E-13,-4.8446668491763));
#61300=CARTESIAN_POINT('Ctrl Pts',(-0.7911,-3.88467036316342E-13,-4.87313315082368));
#61301=CARTESIAN_POINT('Ctrl Pts',(-0.791099999999892,-0.220167589667068,
-4.86427440725041));
#61302=CARTESIAN_POINT('Ctrl Pts',(-0.694214576672153,-0.43861041833903,
-4.85541566367713));
#61303=CARTESIAN_POINT('Ctrl Pts',(-0.531017389080034,-0.586395551223424,
-4.84655692010386));
#61304=CARTESIAN_POINT('Ctrl Pts',(-0.367820201487915,-0.734180684107819,
-4.83769817653059));
#61305=CARTESIAN_POINT('Ctrl Pts',(-0.140868175871331,-0.808992666571409,
-4.82883943295732));
#61306=CARTESIAN_POINT('Ctrl Pts',(0.0782205473251693,-0.787223447298257,
-4.81998068938404));
#61307=CARTESIAN_POINT('Ctrl Pts',(0.29730927052167,-0.765454228025104,
-4.81112194581077));
#61308=CARTESIAN_POINT('Ctrl Pts',(0.50510207267594,-0.647444880833963,
-4.8022632022375));
#61309=CARTESIAN_POINT('Ctrl Pts',(0.636026795761984,-0.470435038100633,
-4.79340445866423));
#61310=CARTESIAN_POINT('Ctrl Pts',(0.766951518848027,-0.293425195367303,
-4.78454571509095));
#61311=CARTESIAN_POINT('Ctrl Pts',(0.818956872247104,-0.0601881960094816,
-4.77568697151768));
#61312=CARTESIAN_POINT('Ctrl Pts',(0.775631781004124,0.155674501111681,
-4.76682822794441));
#61313=CARTESIAN_POINT('Ctrl Pts',(0.732306689761144,0.371537198232844,
-4.75796948437114));
#61314=CARTESIAN_POINT('Ctrl Pts',(0.594329958849895,0.566643518936834,
-4.74911074079786));
#61315=CARTESIAN_POINT('Ctrl Pts',(0.405242230243654,0.679424716084975,
-4.74025199722459));
#61316=CARTESIAN_POINT('Ctrl Pts',(0.216154501637413,0.792205913233117,
-4.73139325365132));
#61317=CARTESIAN_POINT('Ctrl Pts',(-0.0210816529304906,0.820894963712992,
-4.72253451007804));
#61318=CARTESIAN_POINT('Ctrl Pts',(-0.231602780753658,0.756438604215288,
-4.71367576650477));
#61319=CARTESIAN_POINT('Ctrl Pts',(-0.442123908576825,0.691982244717585,
-4.7048170229315));
#61320=CARTESIAN_POINT('Ctrl Pts',(-0.62263162563449,0.535390358803171,
-4.69595827935823));
#61321=CARTESIAN_POINT('Ctrl Pts',(-0.716163994722354,0.336077881841874,
-4.68709953578495));
#61322=CARTESIAN_POINT('Ctrl Pts',(-0.765317280859606,0.231334857514115,
-4.6824440741312));
#61323=CARTESIAN_POINT('Ctrl Pts',(-0.791100000000051,0.115702837836137,
-4.67778861247744));
#61324=CARTESIAN_POINT('Ctrl Pts',(-0.7911,-3.48887585488455E-13,-4.67313315082368));
#61325=CARTESIAN_POINT('Origin',(0.,0.,-5.925));
#61326=CARTESIAN_POINT('',(-0.791966503588212,6.66945195454318E-6,-4.4446668491763));
#61327=CARTESIAN_POINT('',(-0.791525477886921,-8.44546748736536E-5,-4.47313315082368));
#61328=CARTESIAN_POINT('',(-0.7911,-9.68818082805471E-17,-5.925));
#61329=CARTESIAN_POINT('Ctrl Pts',(-0.791966503588212,6.66945195454318E-6,
-4.4446668491763));
#61330=CARTESIAN_POINT('Ctrl Pts',(-0.792369950221889,0.131611474342429,
-4.44997382709989));
#61331=CARTESIAN_POINT('Ctrl Pts',(-0.757450744888324,0.263526968080427,
-4.45528080502347));
#61332=CARTESIAN_POINT('Ctrl Pts',(-0.693836616678797,0.379383898055742,
-4.46058778294706));
#61333=CARTESIAN_POINT('Ctrl Pts',(-0.630359679459704,0.494990969588929,
-4.46588331577853));
#61334=CARTESIAN_POINT('Ctrl Pts',(-0.538311520124503,0.59460866003309,
-4.47117884860999));
#61335=CARTESIAN_POINT('Ctrl Pts',(-0.428005770805877,0.665595456510494,
-4.47647438144146));
#61336=CARTESIAN_POINT('Ctrl Pts',(-0.317700021487244,0.736582252987901,
-4.48176991427292));
#61337=CARTESIAN_POINT('Ctrl Pts',(-0.189136682185182,0.778938155498549,
-4.48706544710439));
#61338=CARTESIAN_POINT('Ctrl Pts',(-0.0575587042796079,0.78869623285,-4.49236097993585));
#61339=CARTESIAN_POINT('Ctrl Pts',(0.0740192736259514,0.798454310201449,
-4.49765651276731));
#61340=CARTESIAN_POINT('Ctrl Pts',(0.208611890135023,0.77561456239371,-4.50295204559878));
#61341=CARTESIAN_POINT('Ctrl Pts',(0.328028928417781,0.720939216440974,
-4.50824757843024));
#61342=CARTESIAN_POINT('Ctrl Pts',(0.566863004983317,0.611588524535494,
-4.51883864409317));
#61343=CARTESIAN_POINT('Ctrl Pts',(0.744994768643586,0.374895440050002,
-4.5294297097561));
#61344=CARTESIAN_POINT('Ctrl Pts',(0.783603804359831,0.115483203003332,
-4.54002077541903));
#61345=CARTESIAN_POINT('Ctrl Pts',(0.802908322217952,-0.0142229155199985,
-4.54531630825049));
#61346=CARTESIAN_POINT('Ctrl Pts',(0.78733215809007,-0.149608822183623,
-4.55061184108196));
#61347=CARTESIAN_POINT('Ctrl Pts',(0.741693763534813,-0.273560253866108,
-4.55590737391342));
#61348=CARTESIAN_POINT('Ctrl Pts',(0.696055368979556,-0.397511685548593,
-4.56120290674489));
#61349=CARTESIAN_POINT('Ctrl Pts',(0.620354743996924,-0.510028642249938,
-4.56649843957635));
#61350=CARTESIAN_POINT('Ctrl Pts',(0.521477628194601,-0.596053955066941,
-4.57179397240782));
#61351=CARTESIAN_POINT('Ctrl Pts',(0.323723396589961,-0.76810458070094,
-4.58238503807075));
#61352=CARTESIAN_POINT('Ctrl Pts',(0.0332632017065634,-0.834188630797575,
-4.59297610373368));
#61353=CARTESIAN_POINT('Ctrl Pts',(-0.21846958092695,-0.761949997232314,
-4.6035671693966));
#61354=CARTESIAN_POINT('Ctrl Pts',(-0.470202363560477,-0.68971136366705,
-4.61415823505953));
#61355=CARTESIAN_POINT('Ctrl Pts',(-0.683207733944114,-0.47915004643987,
-4.62474930072247));
#61356=CARTESIAN_POINT('Ctrl Pts',(-0.758836430659324,-0.228515419272388,
-4.63534036638539));
#61357=CARTESIAN_POINT('Ctrl Pts',(-0.781035951175385,-0.154945877689627,
-4.63844919398236));
#61358=CARTESIAN_POINT('Ctrl Pts',(-0.791398872216265,-0.0779235540097163,
-4.64155802157933));
#61359=CARTESIAN_POINT('Ctrl Pts',(-0.790670861719162,-0.000743182749338822,
-4.64466684917631));
#61360=CARTESIAN_POINT('Ctrl Pts',(-0.7911,-3.48887585488455E-13,-4.67313315082368));
#61361=CARTESIAN_POINT('Ctrl Pts',(-0.791099999999903,-0.220167589667021,
-4.66427440725041));
#61362=CARTESIAN_POINT('Ctrl Pts',(-0.694214576672182,-0.43861041833898,
-4.65541566367714));
#61363=CARTESIAN_POINT('Ctrl Pts',(-0.53101738908008,-0.586395551223383,
-4.64655692010386));
#61364=CARTESIAN_POINT('Ctrl Pts',(-0.367820201487978,-0.734180684107785,
-4.63769817653059));
#61365=CARTESIAN_POINT('Ctrl Pts',(-0.14086817587141,-0.808992666571393,
-4.62883943295732));
#61366=CARTESIAN_POINT('Ctrl Pts',(0.0782205473250852,-0.787223447298265,
-4.61998068938405));
#61367=CARTESIAN_POINT('Ctrl Pts',(0.297309270521581,-0.765454228025137,
-4.61112194581077));
#61368=CARTESIAN_POINT('Ctrl Pts',(0.505102072675857,-0.647444880834025,
-4.6022632022375));
#61369=CARTESIAN_POINT('Ctrl Pts',(0.63602679576192,-0.470435038100719,
-4.59340445866423));
#61370=CARTESIAN_POINT('Ctrl Pts',(0.766951518847983,-0.293425195367412,
-4.58454571509096));
#61371=CARTESIAN_POINT('Ctrl Pts',(0.818956872247093,-0.0601881960096083,
-4.57568697151769));
#61372=CARTESIAN_POINT('Ctrl Pts',(0.77563178100415,0.155674501111554,-4.56682822794441));
#61373=CARTESIAN_POINT('Ctrl Pts',(0.732306689761206,0.371537198232717,
-4.55796948437114));
#61374=CARTESIAN_POINT('Ctrl Pts',(0.594329958849998,0.566643518936723,
-4.54911074079787));
#61375=CARTESIAN_POINT('Ctrl Pts',(0.405242230243785,0.679424716084898,
-4.5402519972246));
#61376=CARTESIAN_POINT('Ctrl Pts',(0.216154501637572,0.792205913233072,
-4.53139325365132));
#61377=CARTESIAN_POINT('Ctrl Pts',(-0.0210816529303167,0.820894963712994,
-4.52253451007805));
#61378=CARTESIAN_POINT('Ctrl Pts',(-0.231602780753491,0.756438604215339,
-4.51367576650478));
#61379=CARTESIAN_POINT('Ctrl Pts',(-0.442123908576665,0.691982244717684,
-4.50481702293151));
#61380=CARTESIAN_POINT('Ctrl Pts',(-0.62263162563436,0.535390358803319,
-4.49595827935823));
#61381=CARTESIAN_POINT('Ctrl Pts',(-0.71616399472227,0.336077881842053,
-4.48709953578496));
#61382=CARTESIAN_POINT('Ctrl Pts',(-0.765317280859574,0.231334857514251,
-4.4824440741312));
#61383=CARTESIAN_POINT('Ctrl Pts',(-0.791100000000049,0.115702837836214,
-4.47778861247744));
#61384=CARTESIAN_POINT('Ctrl Pts',(-0.7911,-3.31845662060459E-13,-4.47313315082368));
#61385=CARTESIAN_POINT('Origin',(0.,0.,-5.925));
#61386=CARTESIAN_POINT('',(-0.791036741154233,7.90254580421569E-5,-4.24466684917631));
#61387=CARTESIAN_POINT('',(-0.790970110322915,0.00058332005030696,-4.27313315082368));
#61388=CARTESIAN_POINT('',(-0.7911,-9.68818082805471E-17,-5.925));
#61389=CARTESIAN_POINT('Ctrl Pts',(-0.790748515183379,0.000439088762327566,
-4.24466684917631));
#61390=CARTESIAN_POINT('Ctrl Pts',(-0.790835927644234,0.0782887347139587,
-4.24779856695752));
#61391=CARTESIAN_POINT('Ctrl Pts',(-0.779640960872226,0.156013699302697,
-4.25093028473873));
#61392=CARTESIAN_POINT('Ctrl Pts',(-0.75709689931653,0.230240171594448,
-4.25406200251995));
#61393=CARTESIAN_POINT('Ctrl Pts',(-0.718976344891441,0.355752350036183,
-4.25935753535141));
#61394=CARTESIAN_POINT('Ctrl Pts',(-0.648405744472263,0.471261419145324,
-4.26465306818287));
#61395=CARTESIAN_POINT('Ctrl Pts',(-0.554435133095759,0.563876258889497,
-4.26994860101434));
#61396=CARTESIAN_POINT('Ctrl Pts',(-0.460464521719244,0.65649109863368,
-4.2752441338458));
#61397=CARTESIAN_POINT('Ctrl Pts',(-0.343093899385398,0.726211709012889,
-4.28053966667727));
#61398=CARTESIAN_POINT('Ctrl Pts',(-0.216681111813741,0.761843571518856,
-4.28583519950874));
#61399=CARTESIAN_POINT('Ctrl Pts',(0.0361444633295574,0.833107296530785,
-4.29642626517167));
#61400=CARTESIAN_POINT('Ctrl Pts',(0.325138699424094,0.768016030049762,
-4.30701733083458));
#61401=CARTESIAN_POINT('Ctrl Pts',(0.522497292065463,0.59528805814275,-4.31760839649752));
#61402=CARTESIAN_POINT('Ctrl Pts',(0.621176588386148,0.508924072189243,
-4.32290392932898));
#61403=CARTESIAN_POINT('Ctrl Pts',(0.696946973843541,0.395650909879239,
-4.32819946216045));
#61404=CARTESIAN_POINT('Ctrl Pts',(0.742402068266281,0.271632141683701,
-4.33349499499192));
#61405=CARTESIAN_POINT('Ctrl Pts',(0.787857162689021,0.147613373488162,
-4.33879052782338));
#61406=CARTESIAN_POINT('Ctrl Pts',(0.802996966077109,0.0128489994070881,
-4.34408606065484));
#61407=CARTESIAN_POINT('Ctrl Pts',(0.783322431151289,-0.116727044482598,
-4.34938159348631));
#61408=CARTESIAN_POINT('Ctrl Pts',(0.743973361299652,-0.375879132261963,
-4.35997265914923));
#61409=CARTESIAN_POINT('Ctrl Pts',(0.565366938192395,-0.614277899275778,
-4.37056372481216));
#61410=CARTESIAN_POINT('Ctrl Pts',(0.326734668627864,-0.722178102956162,
-4.38115479047509));
#61411=CARTESIAN_POINT('Ctrl Pts',(0.0881023990633191,-0.830078306636553,
-4.39174585613802));
#61412=CARTESIAN_POINT('Ctrl Pts',(-0.210555716958507,-0.807479946983497,
-4.40233692180096));
#61413=CARTESIAN_POINT('Ctrl Pts',(-0.430448148214726,-0.665406955959684,
-4.41292798746388));
#61414=CARTESIAN_POINT('Ctrl Pts',(-0.650102955683813,-0.523487494195533,
-4.42350760803469));
#61415=CARTESIAN_POINT('Ctrl Pts',(-0.791162220554377,-0.262351478835906,
-4.43408722860549));
#61416=CARTESIAN_POINT('Ctrl Pts',(-0.791966503588212,6.66945195454318E-6,
-4.4446668491763));
#61417=CARTESIAN_POINT('Ctrl Pts',(-0.792015954376217,-0.000181811160338708,
-4.47313315082368));
#61418=CARTESIAN_POINT('Ctrl Pts',(-0.79106198746347,-0.255451043576872,
-4.46282166976077));
#61419=CARTESIAN_POINT('Ctrl Pts',(-0.657614632699196,-0.509262474217293,
-4.45251018869786));
#61420=CARTESIAN_POINT('Ctrl Pts',(-0.446783095806645,-0.654019263464673,
-4.44219870763495));
#61421=CARTESIAN_POINT('Ctrl Pts',(-0.338509093390211,-0.728360119580303,
-4.43690317480349));
#61422=CARTESIAN_POINT('Ctrl Pts',(-0.209825728930858,-0.773938823051294,
-4.43160764197202));
#61423=CARTESIAN_POINT('Ctrl Pts',(-0.0785231522652674,-0.786885548671759,
-4.42631210914056));
#61424=CARTESIAN_POINT('Ctrl Pts',(0.0527794244003236,-0.799832274292223,
-4.42101657630909));
#61425=CARTESIAN_POINT('Ctrl Pts',(0.186701213272174,-0.780147022062139,
-4.41572104347763));
#61426=CARTESIAN_POINT('Ctrl Pts',(0.307544825190331,-0.729124428385988,
-4.41042551064616));
#61427=CARTESIAN_POINT('Ctrl Pts',(0.428388437108489,-0.678101834709837,
-4.4051299778147));
#61428=CARTESIAN_POINT('Ctrl Pts',(0.536153872072984,-0.595741899587628,
-4.39983444498324));
#61429=CARTESIAN_POINT('Ctrl Pts',(0.618512723066843,-0.492730559385846,
-4.39453891215177));
#61430=CARTESIAN_POINT('Ctrl Pts',(0.700871574060708,-0.389719219184058,
-4.38924337932031));
#61431=CARTESIAN_POINT('Ctrl Pts',(0.757823841083915,-0.266056473902705,
-4.38394784648884));
#61432=CARTESIAN_POINT('Ctrl Pts',(0.780093353519537,-0.136635988479275,
-4.37865231365737));
#61433=CARTESIAN_POINT('Ctrl Pts',(0.824632378390776,0.12220498236757,-4.36806124799444));
#61434=CARTESIAN_POINT('Ctrl Pts',(0.730440384911687,0.40407691378272,-4.35747018233152));
#61435=CARTESIAN_POINT('Ctrl Pts',(0.53816407146517,0.581748620561365,-4.34687911666859));
#61436=CARTESIAN_POINT('Ctrl Pts',(0.345887758018658,0.759420327340004,
-4.33628805100566));
#61437=CARTESIAN_POINT('Ctrl Pts',(0.0555271246047256,0.832891809482146,
-4.32569698534273));
#61438=CARTESIAN_POINT('Ctrl Pts',(-0.198071796498553,0.767505256988222,
-4.3151059196798));
#61439=CARTESIAN_POINT('Ctrl Pts',(-0.451670717601839,0.702118704494297,
-4.30451485401687));
#61440=CARTESIAN_POINT('Ctrl Pts',(-0.668507926394469,0.497874117364298,
-4.29392378835394));
#61441=CARTESIAN_POINT('Ctrl Pts',(-0.751708375512725,0.249306542718858,
-4.28333272269101));
#61442=CARTESIAN_POINT('Ctrl Pts',(-0.778416703304708,0.169513412604227,
-4.2799328654019));
#61443=CARTESIAN_POINT('Ctrl Pts',(-0.791353951428056,0.0851528611175555,
-4.27653300811279));
#61444=CARTESIAN_POINT('Ctrl Pts',(-0.790970110322915,0.00058332005030696,
-4.27313315082368));
#61445=CARTESIAN_POINT('Origin',(0.,0.,-5.925));
#61446=CARTESIAN_POINT('',(-0.791030670713791,-9.38883850568749E-5,-4.04466684917631));
#61447=CARTESIAN_POINT('',(-0.789613844031706,-0.000310489881695122,-4.07313315082369));
#61448=CARTESIAN_POINT('',(-0.7911,-9.68818082805471E-17,-5.925));
#61449=CARTESIAN_POINT('Ctrl Pts',(-0.7911,2.69173572320369E-13,-4.04466684917631));
#61450=CARTESIAN_POINT('Ctrl Pts',(-0.791099999999925,0.220167589666956,
-4.05352559274958));
#61451=CARTESIAN_POINT('Ctrl Pts',(-0.694214576672213,0.43861041833894,
-4.06238433632285));
#61452=CARTESIAN_POINT('Ctrl Pts',(-0.531017389080106,0.586395551223359,
-4.07124307989613));
#61453=CARTESIAN_POINT('Ctrl Pts',(-0.367820201487999,0.734180684107779,
-4.0801018234694));
#61454=CARTESIAN_POINT('Ctrl Pts',(-0.140868175871415,0.808992666571397,
-4.08896056704267));
#61455=CARTESIAN_POINT('Ctrl Pts',(0.0782205473250954,0.787223447298264,
-4.09781931061594));
#61456=CARTESIAN_POINT('Ctrl Pts',(0.297309270521605,0.765454228025131,
-4.10667805418922));
#61457=CARTESIAN_POINT('Ctrl Pts',(0.505102072675893,0.647444880834002,
-4.11553679776249));
#61458=CARTESIAN_POINT('Ctrl Pts',(0.636026795761953,0.470435038100674,
-4.12439554133576));
#61459=CARTESIAN_POINT('Ctrl Pts',(0.766951518848012,0.293425195367347,
-4.13325428490904));
#61460=CARTESIAN_POINT('Ctrl Pts',(0.818956872247103,0.0601881960095193,
-4.14211302848231));
#61461=CARTESIAN_POINT('Ctrl Pts',(0.77563178100413,-0.155674501111652,
-4.15097177205558));
#61462=CARTESIAN_POINT('Ctrl Pts',(0.732306689761156,-0.371537198232824,
-4.15983051562886));
#61463=CARTESIAN_POINT('Ctrl Pts',(0.594329958849906,-0.566643518936825,
-4.16868925920213));
#61464=CARTESIAN_POINT('Ctrl Pts',(0.40524223024366,-0.679424716084972,
-4.1775480027754));
#61465=CARTESIAN_POINT('Ctrl Pts',(0.216154501637414,-0.792205913233119,
-4.18640674634868));
#61466=CARTESIAN_POINT('Ctrl Pts',(-0.0210816529304995,-0.820894963712993,
-4.19526548992195));
#61467=CARTESIAN_POINT('Ctrl Pts',(-0.231602780753673,-0.756438604215284,
-4.20412423349522));
#61468=CARTESIAN_POINT('Ctrl Pts',(-0.442123908576845,-0.691982244717574,
-4.21298297706849));
#61469=CARTESIAN_POINT('Ctrl Pts',(-0.622631625634513,-0.535390358803147,
-4.22184172064177));
#61470=CARTESIAN_POINT('Ctrl Pts',(-0.71616399472237,-0.33607788184184,
-4.23070046421504));
#61471=CARTESIAN_POINT('Ctrl Pts',(-0.765317280859594,-0.231334857514126,
-4.23535592586879));
#61472=CARTESIAN_POINT('Ctrl Pts',(-0.791100000000033,-0.115702837836204,
-4.24001138752255));
#61473=CARTESIAN_POINT('Ctrl Pts',(-0.7911,2.29594121492482E-13,-4.2446668491763));
#61474=CARTESIAN_POINT('Ctrl Pts',(-0.790970110322915,0.00058332005030696,
-4.27313315082368));
#61475=CARTESIAN_POINT('Ctrl Pts',(-0.790756090105803,-0.0465705446553784,
-4.27123747528133));
#61476=CARTESIAN_POINT('Ctrl Pts',(-0.786400677548894,-0.0937893821146618,
-4.26934179973898));
#61477=CARTESIAN_POINT('Ctrl Pts',(-0.777981876000496,-0.140317682337169,
-4.26744612419662));
#61478=CARTESIAN_POINT('Ctrl Pts',(-0.754464117288605,-0.270293585868894,
-4.26215059136516));
#61479=CARTESIAN_POINT('Ctrl Pts',(-0.699237565224288,-0.394880858730763,
-4.25685505853369));
#61480=CARTESIAN_POINT('Ctrl Pts',(-0.616827522050246,-0.496885399689367,
-4.25155952570223));
#61481=CARTESIAN_POINT('Ctrl Pts',(-0.452007435702166,-0.700894481606568,
-4.24096846003929));
#61482=CARTESIAN_POINT('Ctrl Pts',(-0.178453384915186,-0.814572635910709,
-4.23037739437637));
#61483=CARTESIAN_POINT('Ctrl Pts',(0.0828469823253125,-0.787713595922422,
-4.21978632871344));
#61484=CARTESIAN_POINT('Ctrl Pts',(0.213497165945573,-0.774284075928278,
-4.21449079588198));
#61485=CARTESIAN_POINT('Ctrl Pts',(0.341083928679213,-0.725720257361019,
-4.20919526305051));
#61486=CARTESIAN_POINT('Ctrl Pts',(0.449542640975874,-0.650589091588972,
-4.20389973021904));
#61487=CARTESIAN_POINT('Ctrl Pts',(0.558001353272529,-0.57545792581693,
-4.19860419738758));
#61488=CARTESIAN_POINT('Ctrl Pts',(0.647332015132223,-0.473759412840084,
-4.19330866455611));
#61489=CARTESIAN_POINT('Ctrl Pts',(0.706408306709897,-0.35664205554281,
-4.18801313172465));
#61490=CARTESIAN_POINT('Ctrl Pts',(0.765484598287572,-0.239524698245536,
-4.18271759889319));
#61491=CARTESIAN_POINT('Ctrl Pts',(0.794306519583243,-0.106988496627837,
-4.17742206606172));
#61492=CARTESIAN_POINT('Ctrl Pts',(0.790395038786528,0.0248410025943516,
-4.17212653323026));
#61493=CARTESIAN_POINT('Ctrl Pts',(0.786483557989814,0.156670501816548,
-4.16683100039879));
#61494=CARTESIAN_POINT('Ctrl Pts',(0.749838675100704,0.287793298643213,
-4.16153546756733));
#61495=CARTESIAN_POINT('Ctrl Pts',(0.683031628147731,0.400852626912842,
-4.15623993473586));
#61496=CARTESIAN_POINT('Ctrl Pts',(0.549417534241792,0.626971283452087,
-4.14564886907293));
#61497=CARTESIAN_POINT('Ctrl Pts',(0.295154784080413,0.780836065763196,
-4.13505780341001));
#61498=CARTESIAN_POINT('Ctrl Pts',(0.0335873339007514,0.791785271612486,
-4.12446673774708));
#61499=CARTESIAN_POINT('Ctrl Pts',(-0.227980116278903,0.802734477461776,
-4.11387567208415));
#61500=CARTESIAN_POINT('Ctrl Pts',(-0.49685226647684,0.670768106849258,
-4.10328460642122));
#61501=CARTESIAN_POINT('Ctrl Pts',(-0.647814891993137,0.456763200996579,
-4.09269354075829));
#61502=CARTESIAN_POINT('Ctrl Pts',(-0.740751332153453,0.325016326173946,
-4.08617341078009));
#61503=CARTESIAN_POINT('Ctrl Pts',(-0.789000682338518,0.162177277791855,
-4.07965328080189));
#61504=CARTESIAN_POINT('Ctrl Pts',(-0.789613844031706,-0.000310489881695122,
-4.07313315082369));
#61505=CARTESIAN_POINT('Origin',(0.,0.,-5.925));
#61506=CARTESIAN_POINT('',(-0.791171331530249,-5.58023572299298E-6,-3.84466684917632));
#61507=CARTESIAN_POINT('',(-0.791632884276151,-0.000316525830029703,-3.87313315082368));
#61508=CARTESIAN_POINT('',(-0.7911,-9.68818082805471E-17,-5.925));
#61509=CARTESIAN_POINT('Ctrl Pts',(-0.791516496870447,-3.25823843516648E-5,
-3.84466684917631));
#61510=CARTESIAN_POINT('Ctrl Pts',(-0.789509283147655,0.232306133060974,
-3.8540391123357));
#61511=CARTESIAN_POINT('Ctrl Pts',(-0.681965996973624,0.464363987367173,
-3.86341137549509));
#61512=CARTESIAN_POINT('Ctrl Pts',(-0.502861014580263,0.611965760805632,
-3.87278363865449));
#61513=CARTESIAN_POINT('Ctrl Pts',(-0.401662798267677,0.695363977856574,
-3.87807917148596));
#61514=CARTESIAN_POINT('Ctrl Pts',(-0.277618538052244,0.75179962368152,
-3.88337470431743));
#61515=CARTESIAN_POINT('Ctrl Pts',(-0.147877509951437,0.776580384385472,
-3.88867023714889));
#61516=CARTESIAN_POINT('Ctrl Pts',(-0.0181364818506448,0.801361145089422,
-3.89396576998036));
#61517=CARTESIAN_POINT('Ctrl Pts',(0.117301314135521,0.794487020672385,
-3.89926130281182));
#61518=CARTESIAN_POINT('Ctrl Pts',(0.24198381704612,0.754097517796073,-3.90455683564328));
#61519=CARTESIAN_POINT('Ctrl Pts',(0.491348822867332,0.673318512043445,
-3.91514790130621));
#61520=CARTESIAN_POINT('Ctrl Pts',(0.697692656386272,0.458477992453703,
-3.92573896696914));
#61521=CARTESIAN_POINT('Ctrl Pts',(0.765542558291149,0.205526999486113,
-3.93633003263207));
#61522=CARTESIAN_POINT('Ctrl Pts',(0.833392460196026,-0.0474239934814776,
-3.946921098295));
#61523=CARTESIAN_POINT('Ctrl Pts',(0.76274843048684,-0.338485459826917,
-3.95751216395792));
#61524=CARTESIAN_POINT('Ctrl Pts',(0.586955159983497,-0.532480671489366,
-3.96810322962085));
#61525=CARTESIAN_POINT('Ctrl Pts',(0.411161889480155,-0.726475883151815,
-3.97869429528378));
#61526=CARTESIAN_POINT('Ctrl Pts',(0.130219378182655,-0.823404840131275,
-3.98928536094672));
#61527=CARTESIAN_POINT('Ctrl Pts',(-0.129042526256825,-0.781385346657027,
-3.99987642660965));
#61528=CARTESIAN_POINT('Ctrl Pts',(-0.258673478476572,-0.760375599919902,
-4.00517195944111));
#61529=CARTESIAN_POINT('Ctrl Pts',(-0.382884278981814,-0.704628740569346,
-4.01046749227258));
#61530=CARTESIAN_POINT('Ctrl Pts',(-0.486691749451913,-0.623275648299921,
-4.01576302510404));
#61531=CARTESIAN_POINT('Ctrl Pts',(-0.590499219922001,-0.541922556030505,
-4.0210585579355));
#61532=CARTESIAN_POINT('Ctrl Pts',(-0.67390336035695,-0.434963230842226,
-4.02635409076697));
#61533=CARTESIAN_POINT('Ctrl Pts',(-0.726098836681858,-0.314621567823627,
-4.03164962359843));
#61534=CARTESIAN_POINT('Ctrl Pts',(-0.768866977999572,-0.216015527362374,
-4.03598869879106));
#61535=CARTESIAN_POINT('Ctrl Pts',(-0.790681926886867,-0.108424715917689,
-4.04032777398368));
#61536=CARTESIAN_POINT('Ctrl Pts',(-0.790747516019094,-0.000477347360857,
-4.04466684917631));
#61537=CARTESIAN_POINT('Ctrl Pts',(-0.789613844031706,-0.000310489881695122,
-4.07313315082369));
#61538=CARTESIAN_POINT('Ctrl Pts',(-0.789996680236759,-0.101762033633977,
-4.06906221513896));
#61539=CARTESIAN_POINT('Ctrl Pts',(-0.771809470400046,-0.203076637401392,
-4.06499127945423));
#61540=CARTESIAN_POINT('Ctrl Pts',(-0.734334414868844,-0.296601080911116,
-4.0609203437695));
#61541=CARTESIAN_POINT('Ctrl Pts',(-0.68558631313122,-0.418259048392196,
-4.05562481093804));
#61542=CARTESIAN_POINT('Ctrl Pts',(-0.604200885316122,-0.526735139340602,
-4.05032927810657));
#61543=CARTESIAN_POINT('Ctrl Pts',(-0.50213564953078,-0.610577301274807,
-4.04503374527511));
#61544=CARTESIAN_POINT('Ctrl Pts',(-0.400070413745437,-0.694419463209012,
-4.03973821244364));
#61545=CARTESIAN_POINT('Ctrl Pts',(-0.277325369989872,-0.753627696129009,
-4.03444267961218));
#61546=CARTESIAN_POINT('Ctrl Pts',(-0.148480305168211,-0.778026279350681,
-4.02914714678072));
#61547=CARTESIAN_POINT('Ctrl Pts',(0.109209824475106,-0.826823445794026,
-4.01855608111779));
#61548=CARTESIAN_POINT('Ctrl Pts',(0.391300038382742,-0.736382013444024,
-4.00796501545485));
#61549=CARTESIAN_POINT('Ctrl Pts',(0.573073513987495,-0.546756873982823,
-3.99737394979192));
#61550=CARTESIAN_POINT('Ctrl Pts',(0.663960251789879,-0.451944304252214,
-3.99207841696046));
#61551=CARTESIAN_POINT('Ctrl Pts',(0.729767805016544,-0.332335807743801,
-3.986782884129));
#61552=CARTESIAN_POINT('Ctrl Pts',(0.76379769728162,-0.204860512977544,
-3.98148735129753));
#61553=CARTESIAN_POINT('Ctrl Pts',(0.797827589546692,-0.0773852182113021,
-3.97619181846607));
#61554=CARTESIAN_POINT('Ctrl Pts',(0.800079820850182,0.0579568748127813,
-3.9708962856346));
#61555=CARTESIAN_POINT('Ctrl Pts',(0.769291022740716,0.185465829470251,
-3.96560075280314));
#61556=CARTESIAN_POINT('Ctrl Pts',(0.73850222463125,0.312974784127721,-3.96030521997167));
#61557=CARTESIAN_POINT('Ctrl Pts',(0.674672397108829,0.432650600418577,
-3.95500968714021));
#61558=CARTESIAN_POINT('Ctrl Pts',(0.586350956631833,0.530597727478346,
-3.94971415430875));
#61559=CARTESIAN_POINT('Ctrl Pts',(0.498029516154827,0.628544854538127,
-3.94441862147728));
#61560=CARTESIAN_POINT('Ctrl Pts',(0.385216462723241,0.704763292366816,
-3.93912308864582));
#61561=CARTESIAN_POINT('Ctrl Pts',(0.261107514977984,0.747688370362337,
-3.93382755581435));
#61562=CARTESIAN_POINT('Ctrl Pts',(0.0128896194874833,0.833538526353374,
-3.92323649015142));
#61563=CARTESIAN_POINT('Ctrl Pts',(-0.280511853257697,0.786215243011755,
-3.91264542448849));
#61564=CARTESIAN_POINT('Ctrl Pts',(-0.486964156575668,0.625234304522367,
-3.90205435882556));
#61565=CARTESIAN_POINT('Ctrl Pts',(-0.67488512684609,0.478703150983351,
-3.89241395615827));
#61566=CARTESIAN_POINT('Ctrl Pts',(-0.79076563914733,0.23800261569534,-3.88277355349098));
#61567=CARTESIAN_POINT('Ctrl Pts',(-0.792351145598852,-0.000743163040590685,
-3.87313315082368));
#61568=CARTESIAN_POINT('Origin',(0.,0.,-5.925));
#61569=CARTESIAN_POINT('',(-0.7911,2.80775402927702E-13,-3.64466684917631));
#61570=CARTESIAN_POINT('',(-0.7911,-2.86048962294672E-13,-3.67313315082368));
#61571=CARTESIAN_POINT('',(-0.7911,-9.68818082805471E-17,-5.925));
#61572=CARTESIAN_POINT('Ctrl Pts',(-0.7911,2.80775402927702E-13,-3.64466684917631));
#61573=CARTESIAN_POINT('Ctrl Pts',(-0.791099999999922,0.22016758966696,
-3.65352559274958));
#61574=CARTESIAN_POINT('Ctrl Pts',(-0.694214576672213,0.438610418338935,
-3.66238433632285));
#61575=CARTESIAN_POINT('Ctrl Pts',(-0.531017389080114,0.586395551223352,
-3.67124307989613));
#61576=CARTESIAN_POINT('Ctrl Pts',(-0.367820201488015,0.734180684107769,
-3.6801018234694));
#61577=CARTESIAN_POINT('Ctrl Pts',(-0.140868175871441,0.80899266657139,
-3.68896056704267));
#61578=CARTESIAN_POINT('Ctrl Pts',(0.0782205473250622,0.787223447298267,
-3.69781931061594));
#61579=CARTESIAN_POINT('Ctrl Pts',(0.297309270521566,0.765454228025144,
-3.70667805418922));
#61580=CARTESIAN_POINT('Ctrl Pts',(0.505102072675852,0.647444880834032,
-3.71553679776249));
#61581=CARTESIAN_POINT('Ctrl Pts',(0.63602679576192,0.470435038100719,-3.72439554133576));
#61582=CARTESIAN_POINT('Ctrl Pts',(0.766951518847987,0.293425195367407,
-3.73325428490903));
#61583=CARTESIAN_POINT('Ctrl Pts',(0.818956872247096,0.060188196009593,
-3.74211302848231));
#61584=CARTESIAN_POINT('Ctrl Pts',(0.775631781004145,-0.155674501111576,
-3.75097177205558));
#61585=CARTESIAN_POINT('Ctrl Pts',(0.732306689761194,-0.371537198232744,
-3.75983051562885));
#61586=CARTESIAN_POINT('Ctrl Pts',(0.594329958849972,-0.566643518936753,
-3.76868925920212));
#61587=CARTESIAN_POINT('Ctrl Pts',(0.405242230243747,-0.67942471608492,
-3.7775480027754));
#61588=CARTESIAN_POINT('Ctrl Pts',(0.216154501637521,-0.792205913233088,
-3.78640674634867));
#61589=CARTESIAN_POINT('Ctrl Pts',(-0.0210816529303789,-0.820894963712994,
-3.79526548992194));
#61590=CARTESIAN_POINT('Ctrl Pts',(-0.231602780753555,-0.756438604215319,
-3.80412423349522));
#61591=CARTESIAN_POINT('Ctrl Pts',(-0.44212390857673,-0.691982244717645,
-3.81298297706849));
#61592=CARTESIAN_POINT('Ctrl Pts',(-0.622631625634417,-0.535390358803255,
-3.82184172064176));
#61593=CARTESIAN_POINT('Ctrl Pts',(-0.716163994722308,-0.336077881841972,
-3.83070046421503));
#61594=CARTESIAN_POINT('Ctrl Pts',(-0.76531728085958,-0.231334857514206,
-3.83535592586879));
#61595=CARTESIAN_POINT('Ctrl Pts',(-0.791100000000042,-0.115702837836215,
-3.84001138752255));
#61596=CARTESIAN_POINT('Ctrl Pts',(-0.7911,2.86215495748365E-13,-3.84466684917631));
#61597=CARTESIAN_POINT('Ctrl Pts',(-0.7911,-3.0320190802513E-13,-3.87313315082368));
#61598=CARTESIAN_POINT('Ctrl Pts',(-0.791099999999916,-0.22016758966699,
-3.86427440725041));
#61599=CARTESIAN_POINT('Ctrl Pts',(-0.694214576672194,-0.43861041833897,
-3.85541566367714));
#61600=CARTESIAN_POINT('Ctrl Pts',(-0.531017389080081,-0.586395551223382,
-3.84655692010386));
#61601=CARTESIAN_POINT('Ctrl Pts',(-0.367820201487968,-0.734180684107795,
-3.83769817653059));
#61602=CARTESIAN_POINT('Ctrl Pts',(-0.14086817587138,-0.808992666571403,
-3.82883943295732));
#61603=CARTESIAN_POINT('Ctrl Pts',(0.0782205473251291,-0.787223447298261,
-3.81998068938405));
#61604=CARTESIAN_POINT('Ctrl Pts',(0.297309270521638,-0.765454228025119,
-3.81112194581077));
#61605=CARTESIAN_POINT('Ctrl Pts',(0.505102072675921,-0.64744488083398,
-3.8022632022375));
#61606=CARTESIAN_POINT('Ctrl Pts',(0.636026795761973,-0.470435038100647,
-3.79340445866423));
#61607=CARTESIAN_POINT('Ctrl Pts',(0.766951518848025,-0.293425195367314,
-3.78454571509095));
#61608=CARTESIAN_POINT('Ctrl Pts',(0.818956872247106,-0.0601881960094841,
-3.77568697151768));
#61609=CARTESIAN_POINT('Ctrl Pts',(0.775631781004123,0.155674501111686,
-3.76682822794441));
#61610=CARTESIAN_POINT('Ctrl Pts',(0.732306689761141,0.371537198232848,
-3.75796948437113));
#61611=CARTESIAN_POINT('Ctrl Pts',(0.594329958849892,0.566643518936837,
-3.74911074079786));
#61612=CARTESIAN_POINT('Ctrl Pts',(0.40524223024365,0.679424716084978,-3.74025199722459));
#61613=CARTESIAN_POINT('Ctrl Pts',(0.216154501637408,0.792205913233119,
-3.73139325365132));
#61614=CARTESIAN_POINT('Ctrl Pts',(-0.0210816529304954,0.820894963712992,
-3.72253451007804));
#61615=CARTESIAN_POINT('Ctrl Pts',(-0.231602780753662,0.756438604215287,
-3.71367576650477));
#61616=CARTESIAN_POINT('Ctrl Pts',(-0.442123908576829,0.691982244717582,
-3.7048170229315));
#61617=CARTESIAN_POINT('Ctrl Pts',(-0.622631625634493,0.535390358803167,
-3.69595827935823));
#61618=CARTESIAN_POINT('Ctrl Pts',(-0.716163994722355,0.33607788184187,
-3.68709953578495));
#61619=CARTESIAN_POINT('Ctrl Pts',(-0.765317280859597,0.231334857514131,
-3.6824440741312));
#61620=CARTESIAN_POINT('Ctrl Pts',(-0.791100000000042,0.115702837836177,
-3.67778861247744));
#61621=CARTESIAN_POINT('Ctrl Pts',(-0.7911,-2.86048962294672E-13,-3.67313315082368));
#61622=CARTESIAN_POINT('Origin',(0.,0.,-5.925));
#61623=CARTESIAN_POINT('',(-0.790808073136235,0.000138710378817367,-3.44466684917631));
#61624=CARTESIAN_POINT('',(-0.790458003125287,-0.000155518975336373,-3.47313315082369));
#61625=CARTESIAN_POINT('',(-0.7911,-9.68818082805471E-17,-5.925));
#61626=CARTESIAN_POINT('Ctrl Pts',(-0.7911,2.97872837506929E-13,-3.44466684917631));
#61627=CARTESIAN_POINT('Ctrl Pts',(-0.791099999999917,0.220167589666978,
-3.45352559274958));
#61628=CARTESIAN_POINT('Ctrl Pts',(-0.694214576672203,0.43861041833895,
-3.46238433632285));
#61629=CARTESIAN_POINT('Ctrl Pts',(-0.531017389080101,0.586395551223364,
-3.47124307989613));
#61630=CARTESIAN_POINT('Ctrl Pts',(-0.367820201487999,0.734180684107777,
-3.4801018234694));
#61631=CARTESIAN_POINT('Ctrl Pts',(-0.140868175871424,0.808992666571393,
-3.48896056704267));
#61632=CARTESIAN_POINT('Ctrl Pts',(0.078220547325079,0.787223447298266,
-3.49781931061594));
#61633=CARTESIAN_POINT('Ctrl Pts',(0.297309270521582,0.765454228025138,
-3.50667805418922));
#61634=CARTESIAN_POINT('Ctrl Pts',(0.505102072675866,0.647444880834021,
-3.51553679776249));
#61635=CARTESIAN_POINT('Ctrl Pts',(0.63602679576193,0.470435038100706,-3.52439554133576));
#61636=CARTESIAN_POINT('Ctrl Pts',(0.766951518847993,0.29342519536739,-3.53325428490903));
#61637=CARTESIAN_POINT('Ctrl Pts',(0.818956872247097,0.0601881960095753,
-3.54211302848231));
#61638=CARTESIAN_POINT('Ctrl Pts',(0.775631781004142,-0.155674501111592,
-3.55097177205558));
#61639=CARTESIAN_POINT('Ctrl Pts',(0.732306689761186,-0.37153719823276,
-3.55983051562885));
#61640=CARTESIAN_POINT('Ctrl Pts',(0.59432995884996,-0.566643518936766,
-3.56868925920213));
#61641=CARTESIAN_POINT('Ctrl Pts',(0.405242230243732,-0.679424716084929,
-3.5775480027754));
#61642=CARTESIAN_POINT('Ctrl Pts',(0.216154501637504,-0.792205913233092,
-3.58640674634867));
#61643=CARTESIAN_POINT('Ctrl Pts',(-0.0210816529303965,-0.820894963712994,
-3.59526548992194));
#61644=CARTESIAN_POINT('Ctrl Pts',(-0.231602780753571,-0.756438604215315,
-3.60412423349522));
#61645=CARTESIAN_POINT('Ctrl Pts',(-0.442123908576745,-0.691982244717635,
-3.61298297706849));
#61646=CARTESIAN_POINT('Ctrl Pts',(-0.622631625634429,-0.535390358803242,
-3.62184172064176));
#61647=CARTESIAN_POINT('Ctrl Pts',(-0.716163994722315,-0.336077881841956,
-3.63070046421503));
#61648=CARTESIAN_POINT('Ctrl Pts',(-0.765317280859582,-0.231334857514196,
-3.63535592586879));
#61649=CARTESIAN_POINT('Ctrl Pts',(-0.791100000000041,-0.115702837836213,
-3.64001138752255));
#61650=CARTESIAN_POINT('Ctrl Pts',(-0.7911,2.80775402927702E-13,-3.64466684917631));
#61651=CARTESIAN_POINT('Ctrl Pts',(-0.7911,-2.86048962294672E-13,-3.67313315082368));
#61652=CARTESIAN_POINT('Ctrl Pts',(-0.791099999999921,-0.220167589666966,
-3.66427440725041));
#61653=CARTESIAN_POINT('Ctrl Pts',(-0.69421457667221,-0.43861041833894,
-3.65541566367714));
#61654=CARTESIAN_POINT('Ctrl Pts',(-0.53101738908011,-0.586395551223356,
-3.64655692010387));
#61655=CARTESIAN_POINT('Ctrl Pts',(-0.36782020148801,-0.734180684107771,
-3.63769817653059));
#61656=CARTESIAN_POINT('Ctrl Pts',(-0.140868175871436,-0.808992666571391,
-3.62883943295732));
#61657=CARTESIAN_POINT('Ctrl Pts',(0.0782205473250674,-0.787223447298267,
-3.61998068938405));
#61658=CARTESIAN_POINT('Ctrl Pts',(0.297309270521571,-0.765454228025143,
-3.61112194581078));
#61659=CARTESIAN_POINT('Ctrl Pts',(0.505102072675857,-0.647444880834028,
-3.6022632022375));
#61660=CARTESIAN_POINT('Ctrl Pts',(0.636026795761923,-0.470435038100715,
-3.59340445866423));
#61661=CARTESIAN_POINT('Ctrl Pts',(0.766951518847989,-0.293425195367402,
-3.58454571509096));
#61662=CARTESIAN_POINT('Ctrl Pts',(0.818956872247096,-0.0601881960095875,
-3.57568697151768));
#61663=CARTESIAN_POINT('Ctrl Pts',(0.775631781004144,0.155674501111581,
-3.56682822794441));
#61664=CARTESIAN_POINT('Ctrl Pts',(0.732306689761192,0.371537198232749,
-3.55796948437114));
#61665=CARTESIAN_POINT('Ctrl Pts',(0.594329958849968,0.566643518936757,
-3.54911074079787));
#61666=CARTESIAN_POINT('Ctrl Pts',(0.405242230243742,0.679424716084923,
-3.54025199722459));
#61667=CARTESIAN_POINT('Ctrl Pts',(0.216154501637516,0.792205913233089,
-3.53139325365132));
#61668=CARTESIAN_POINT('Ctrl Pts',(-0.0210816529303844,0.820894963712995,
-3.52253451007805));
#61669=CARTESIAN_POINT('Ctrl Pts',(-0.23160278075356,0.756438604215318,
-3.51367576650478));
#61670=CARTESIAN_POINT('Ctrl Pts',(-0.442123908576735,0.691982244717642,
-3.5048170229315));
#61671=CARTESIAN_POINT('Ctrl Pts',(-0.622631625634421,0.535390358803251,
-3.49595827935823));
#61672=CARTESIAN_POINT('Ctrl Pts',(-0.71616399472231,0.336077881841967,
-3.48709953578496));
#61673=CARTESIAN_POINT('Ctrl Pts',(-0.765317280859573,0.231334857514221,
-3.4824440741312));
#61674=CARTESIAN_POINT('Ctrl Pts',(-0.791100000000033,0.115702837836254,
-3.47778861247744));
#61675=CARTESIAN_POINT('Ctrl Pts',(-0.7911,-2.24043006369357E-13,-3.47313315082369));
#61676=CARTESIAN_POINT('Origin',(0.,0.,-5.925));
#61677=CARTESIAN_POINT('',(-0.790501282281534,-0.000660443323588278,-3.24466684917631));
#61678=CARTESIAN_POINT('',(-0.791626275438383,-0.000301773140805729,-3.27313315082369));
#61679=CARTESIAN_POINT('',(-0.7911,-9.68818082805471E-17,-5.925));
#61680=CARTESIAN_POINT('Ctrl Pts',(-0.790501282281534,-0.000660443323588278,
-3.24466684917631));
#61681=CARTESIAN_POINT('Ctrl Pts',(-0.788726547930076,0.201687602482837,
-3.25280886474005));
#61682=CARTESIAN_POINT('Ctrl Pts',(-0.710464001792085,0.405146793643893,
-3.26095088030379));
#61683=CARTESIAN_POINT('Ctrl Pts',(-0.570712392114347,0.550076468829417,
-3.26909289586753));
#61684=CARTESIAN_POINT('Ctrl Pts',(-0.388924668545188,0.738599776649255,
-3.27968396153046));
#61685=CARTESIAN_POINT('Ctrl Pts',(-0.103093830595221,0.828087698747892,
-3.29027502719339));
#61686=CARTESIAN_POINT('Ctrl Pts',(0.153756508941375,0.777438718677672,
-3.30086609285632));
#61687=CARTESIAN_POINT('Ctrl Pts',(0.410606848477986,0.726789738607448,
-3.31145715851925));
#61688=CARTESIAN_POINT('Ctrl Pts',(0.638476689601239,0.536003856368347,
-3.32204822418218));
#61689=CARTESIAN_POINT('Ctrl Pts',(0.7361029627146,0.292177106967427,-3.33263928984511));
#61690=CARTESIAN_POINT('Ctrl Pts',(0.784916099271274,0.17026373226698,-3.33793482267657));
#61691=CARTESIAN_POINT('Ctrl Pts',(0.801168343825486,0.0350901407761204,
-3.34323035550804));
#61692=CARTESIAN_POINT('Ctrl Pts',(0.784961259371031,-0.0957977767742774,
-3.3485258883395));
#61693=CARTESIAN_POINT('Ctrl Pts',(0.768754174916574,-0.22668569432469,
-3.35382142117096));
#61694=CARTESIAN_POINT('Ctrl Pts',(0.720087761453432,-0.353287937934607,
-3.35911695400243));
#61695=CARTESIAN_POINT('Ctrl Pts',(0.643867493490231,-0.460044456979054,
-3.36441248683389));
#61696=CARTESIAN_POINT('Ctrl Pts',(0.56764722552703,-0.5668009760235,-3.36970801966536));
#61697=CARTESIAN_POINT('Ctrl Pts',(0.463873103063763,-0.653711770502485,
-3.37500355249682));
#61698=CARTESIAN_POINT('Ctrl Pts',(0.345239232099723,-0.711452475411619,
-3.38029908532829));
#61699=CARTESIAN_POINT('Ctrl Pts',(0.226605361135696,-0.769193180320747,
-3.38559461815975));
#61700=CARTESIAN_POINT('Ctrl Pts',(0.09311174167089,-0.797763795660035,
-3.39089015099122));
#61701=CARTESIAN_POINT('Ctrl Pts',(-0.0380598711096725,-0.791143335870662,
-3.39618568382268));
#61702=CARTESIAN_POINT('Ctrl Pts',(-0.300403096670812,-0.777902416291914,
-3.40677674948561));
#61703=CARTESIAN_POINT('Ctrl Pts',(-0.553458295495004,-0.623897196198503,
-3.41736781514854));
#61704=CARTESIAN_POINT('Ctrl Pts',(-0.685293196148034,-0.397170653115661,
-3.42795888081147));
#61705=CARTESIAN_POINT('Ctrl Pts',(-0.751210646474553,-0.283807381574233,
-3.43325441364294));
#61706=CARTESIAN_POINT('Ctrl Pts',(-0.786823022258281,-0.152263779285441,
-3.4385499464744));
#61707=CARTESIAN_POINT('Ctrl Pts',(-0.790275839006138,-0.0202225034273728,
-3.44384547930586));
#61708=CARTESIAN_POINT('Ctrl Pts',(-0.790454356745215,-0.0133956974447719,
-3.44411926926268));
#61709=CARTESIAN_POINT('Ctrl Pts',(-0.790546908669895,-0.00656756112944958,
-3.44439305921949));
#61710=CARTESIAN_POINT('Ctrl Pts',(-0.790553609093959,0.000259620127130655,
-3.44466684917631));
#61711=CARTESIAN_POINT('Ctrl Pts',(-0.789563719361682,-0.000372152575058701,
-3.47313315082369));
#61712=CARTESIAN_POINT('Ctrl Pts',(-0.789761280241986,-0.132415731864222,
-3.4678319675433));
#61713=CARTESIAN_POINT('Ctrl Pts',(-0.758600248492401,-0.264319284924409,
-3.46253078426292));
#61714=CARTESIAN_POINT('Ctrl Pts',(-0.695813536878054,-0.379335665655462,
-3.45722960098254));
#61715=CARTESIAN_POINT('Ctrl Pts',(-0.570373960410714,-0.609123238770098,
-3.44663853531961));
#61716=CARTESIAN_POINT('Ctrl Pts',(-0.318701195330903,-0.771506044022968,
-3.43604746965668));
#61717=CARTESIAN_POINT('Ctrl Pts',(-0.0575027298276114,-0.790563211979342,
-3.42545640399375));
#61718=CARTESIAN_POINT('Ctrl Pts',(0.20369573567568,-0.809620379935717,
-3.41486533833082));
#61719=CARTESIAN_POINT('Ctrl Pts',(0.474419901602451,-0.685351910595596,
-3.40427427266789));
#61720=CARTESIAN_POINT('Ctrl Pts',(0.632670215342768,-0.476390210517119,
-3.39368320700496));
#61721=CARTESIAN_POINT('Ctrl Pts',(0.711795372212922,-0.371909360477886,
-3.3883876741735));
#61722=CARTESIAN_POINT('Ctrl Pts',(0.762802066036466,-0.246255202754067,
-3.38309214134204));
#61723=CARTESIAN_POINT('Ctrl Pts',(0.782040115544297,-0.115577286008921,
-3.37779660851057));
#61724=CARTESIAN_POINT('Ctrl Pts',(0.80127816505213,0.0151006307362397,
-3.37250107567911));
#61725=CARTESIAN_POINT('Ctrl Pts',(0.788747570244242,0.150802306502729,
-3.36720554284764));
#61726=CARTESIAN_POINT('Ctrl Pts',(0.743243492909288,0.273788974633951,
-3.36191001001617));
#61727=CARTESIAN_POINT('Ctrl Pts',(0.652235338239384,0.519762310896381,
-3.35131894435324));
#61728=CARTESIAN_POINT('Ctrl Pts',(0.42933325346123,0.71487561661775,-3.34072787869032));
#61729=CARTESIAN_POINT('Ctrl Pts',(0.17314530709567,0.772901697703007,-3.33013681302739));
#61730=CARTESIAN_POINT('Ctrl Pts',(0.0450513339128974,0.801914738245634,
-3.32484128019593));
#61731=CARTESIAN_POINT('Ctrl Pts',(-0.0913641046667258,0.796655972629236,
-3.31954574736446));
#61732=CARTESIAN_POINT('Ctrl Pts',(-0.218141339923086,0.760111247099192,
-3.314250214533));
#61733=CARTESIAN_POINT('Ctrl Pts',(-0.344918575179461,0.723566521569144,
-3.30895468170153));
#61734=CARTESIAN_POINT('Ctrl Pts',(-0.462057607112571,0.655735836125442,
-3.30365914887007));
#61735=CARTESIAN_POINT('Ctrl Pts',(-0.555453563471992,0.563628947443981,
-3.2983636160386));
#61736=CARTESIAN_POINT('Ctrl Pts',(-0.648849519831414,0.47152205876252,
-3.29306808320714));
#61737=CARTESIAN_POINT('Ctrl Pts',(-0.718502400617147,0.355138966843301,
-3.28777255037567));
#61738=CARTESIAN_POINT('Ctrl Pts',(-0.756911456836638,0.228968205779075,
-3.28247701754421));
#61739=CARTESIAN_POINT('Ctrl Pts',(-0.779502139310456,0.15475957163837,
-3.27936239530403));
#61740=CARTESIAN_POINT('Ctrl Pts',(-0.791284565813894,0.0771650641309663,
-3.27624777306386));
#61741=CARTESIAN_POINT('Ctrl Pts',(-0.791626275438383,-0.000301773140805729,
-3.27313315082369));
#61742=CARTESIAN_POINT('Origin',(0.,0.,-5.925));
#61743=CARTESIAN_POINT('',(-0.792512397087544,4.98421984640521E-5,-3.04466684917631));
#61744=CARTESIAN_POINT('',(-0.791208548896392,0.000277519652998023,-3.07313315082369));
#61745=CARTESIAN_POINT('',(-0.7911,-9.68818082805471E-17,-5.925));
#61746=CARTESIAN_POINT('Ctrl Pts',(-0.792512397087544,4.98421984640521E-5,
-3.04466684917631));
#61747=CARTESIAN_POINT('Ctrl Pts',(-0.792602493697506,0.0166490096803601,
-3.04533807176621));
#61748=CARTESIAN_POINT('Ctrl Pts',(-0.792131796472667,0.033246426247799,
-3.04600929435612));
#61749=CARTESIAN_POINT('Ctrl Pts',(-0.79108507893974,0.0498111829976684,
-3.04668051694602));
#61750=CARTESIAN_POINT('Ctrl Pts',(-0.77456916560708,0.31118264019715,-3.05727158260895));
#61751=CARTESIAN_POINT('Ctrl Pts',(-0.61464174908658,0.564422798090375,
-3.06786264827188));
#61752=CARTESIAN_POINT('Ctrl Pts',(-0.386085039148666,0.692091300253508,
-3.07845371393481));
#61753=CARTESIAN_POINT('Ctrl Pts',(-0.157528329210766,0.819759802416634,
-3.08904477959774));
#61754=CARTESIAN_POINT('Ctrl Pts',(0.139657674144527,0.821856648849676,
-3.09963584526066));
#61755=CARTESIAN_POINT('Ctrl Pts',(0.371909359946098,0.699212744118375,
-3.11022691092359));
#61756=CARTESIAN_POINT('Ctrl Pts',(0.48803520284691,0.637890791752711,-3.11552244375506));
#61757=CARTESIAN_POINT('Ctrl Pts',(0.587927466359278,0.545383651595948,
-3.12081797658652));
#61758=CARTESIAN_POINT('Ctrl Pts',(0.660305185987155,0.43513038747796,-3.12611350941799));
#61759=CARTESIAN_POINT('Ctrl Pts',(0.732682905615016,0.324877123359996,
-3.13140904224946));
#61760=CARTESIAN_POINT('Ctrl Pts',(0.777546081358393,0.196877735280824,
-3.13670457508092));
#61761=CARTESIAN_POINT('Ctrl Pts',(0.788560784364571,0.0661675217374577,
-3.14200010791238));
#61762=CARTESIAN_POINT('Ctrl Pts',(0.799575487370749,-0.0645426918059086,
-3.14729564074385));
#61763=CARTESIAN_POINT('Ctrl Pts',(0.776741717639716,-0.1979637308135,-3.15259117357531));
#61764=CARTESIAN_POINT('Ctrl Pts',(0.72369865590798,-0.318771089635041,
-3.15788670640678));
#61765=CARTESIAN_POINT('Ctrl Pts',(0.670655594176238,-0.439578448456596,
-3.16318223923824));
#61766=CARTESIAN_POINT('Ctrl Pts',(0.587403240443787,-0.547772127092131,
-3.16847777206971));
#61767=CARTESIAN_POINT('Ctrl Pts',(0.483139671131421,-0.627640334794113,
-3.17377330490117));
#61768=CARTESIAN_POINT('Ctrl Pts',(0.274612532506713,-0.787376750198057,
-3.1843643705641));
#61769=CARTESIAN_POINT('Ctrl Pts',(-0.0179594684376078,-0.833811281867799,
-3.19495543622703));
#61770=CARTESIAN_POINT('Ctrl Pts',(-0.265214795997095,-0.746346035272733,
-3.20554650188996));
#61771=CARTESIAN_POINT('Ctrl Pts',(-0.388842459776839,-0.7026134119752,
-3.21084203472142));
#61772=CARTESIAN_POINT('Ctrl Pts',(-0.501140955210369,-0.625405844111466,
-3.21613756755288));
#61773=CARTESIAN_POINT('Ctrl Pts',(-0.589249900279902,-0.527000385561387,
-3.22143310038435));
#61774=CARTESIAN_POINT('Ctrl Pts',(-0.677358845349455,-0.428594927011285,
-3.22672863321581));
#61775=CARTESIAN_POINT('Ctrl Pts',(-0.741278240054995,-0.308991577774832,
-3.23202416604728));
#61776=CARTESIAN_POINT('Ctrl Pts',(-0.770933734993954,-0.181329562693679,
-3.23731969887875));
#61777=CARTESIAN_POINT('Ctrl Pts',(-0.784648651912265,-0.122289107153613,
-3.23976874897794));
#61778=CARTESIAN_POINT('Ctrl Pts',(-0.791035107512577,-0.06152504101114,
-3.24221779907712));
#61779=CARTESIAN_POINT('Ctrl Pts',(-0.790501282281534,-0.000660443323588278,
-3.24466684917631));
#61780=CARTESIAN_POINT('Ctrl Pts',(-0.791626275438383,-0.000301773140805729,
-3.27313315082369));
#61781=CARTESIAN_POINT('Ctrl Pts',(-0.791865546233275,-0.0545453483971053,
-3.2709522402324));
#61782=CARTESIAN_POINT('Ctrl Pts',(-0.786495393900723,-0.1087263264945,
-3.26877132964111));
#61783=CARTESIAN_POINT('Ctrl Pts',(-0.775298682791673,-0.161638442254814,
-3.26659041904982));
#61784=CARTESIAN_POINT('Ctrl Pts',(-0.72092455895627,-0.418593355775735,
-3.25599935338689));
#61785=CARTESIAN_POINT('Ctrl Pts',(-0.529141260837061,-0.645624375501621,
-3.24540828772396));
#61786=CARTESIAN_POINT('Ctrl Pts',(-0.284778825431726,-0.739562739682541,
-3.23481722206103));
#61787=CARTESIAN_POINT('Ctrl Pts',(-0.0404163900263632,-0.833501103863472,
-3.2242261563981));
#61788=CARTESIAN_POINT('Ctrl Pts',(0.256525182665126,-0.794346812499395,
-3.21363509073517));
#61789=CARTESIAN_POINT('Ctrl Pts',(0.467944958166465,-0.639784551391566,
-3.20304402507224));
#61790=CARTESIAN_POINT('Ctrl Pts',(0.679364733667791,-0.485222290283745,
-3.19245295940931));
#61791=CARTESIAN_POINT('Ctrl Pts',(0.805262711978977,-0.215252059432152,
-3.18186189374638));
#61792=CARTESIAN_POINT('Ctrl Pts',(0.790607784950011,0.0464603533655111,
-3.17127082808345));
#61793=CARTESIAN_POINT('Ctrl Pts',(0.783280321435528,0.177316559764335,
-3.16597529525199));
#61794=CARTESIAN_POINT('Ctrl Pts',(0.74081463158602,0.306108311649677,-3.16067976242052));
#61795=CARTESIAN_POINT('Ctrl Pts',(0.670883030216598,0.418163617653569,
-3.15538422958906));
#61796=CARTESIAN_POINT('Ctrl Pts',(0.600951428847175,0.53021892365746,-3.15008869675759));
#61797=CARTESIAN_POINT('Ctrl Pts',(0.503553915957842,0.625537783779891,
-3.14479316392613));
#61798=CARTESIAN_POINT('Ctrl Pts',(0.389255408503693,0.689819918046538,
-3.13949763109466));
#61799=CARTESIAN_POINT('Ctrl Pts',(0.160658393595382,0.818384186579839,
-3.12890656543173));
#61800=CARTESIAN_POINT('Ctrl Pts',(-0.135542599572178,0.822801551689975,
-3.11831549976881));
#61801=CARTESIAN_POINT('Ctrl Pts',(-0.368370023734614,0.701184609995972,
-3.10772443410588));
#61802=CARTESIAN_POINT('Ctrl Pts',(-0.484783735815838,0.640376139148968,
-3.10242890127441));
#61803=CARTESIAN_POINT('Ctrl Pts',(-0.585354055645775,0.548059091600927,
-3.09713336844295));
#61804=CARTESIAN_POINT('Ctrl Pts',(-0.65832518346277,0.438135487000128,
-3.09183783561148));
#61805=CARTESIAN_POINT('Ctrl Pts',(-0.731296311279756,0.328211882399341,
-3.08654230278002));
#61806=CARTESIAN_POINT('Ctrl Pts',(-0.776668247083802,0.200681720745806,
-3.08124676994855));
#61807=CARTESIAN_POINT('Ctrl Pts',(-0.7882281697482,0.0700185974291656,
-3.07595123711709));
#61808=CARTESIAN_POINT('Ctrl Pts',(-0.7902787572056,0.0468405737004255,
-3.07501187501929));
#61809=CARTESIAN_POINT('Ctrl Pts',(-0.791265403124425,0.0235639670201663,
-3.07407251292149));
#61810=CARTESIAN_POINT('Ctrl Pts',(-0.791208548896392,0.000277519652998023,
-3.07313315082369));
#61811=CARTESIAN_POINT('Origin',(0.,0.,-5.925));
#61812=CARTESIAN_POINT('',(-0.79070696665834,0.000316758284698436,-2.84466684917631));
#61813=CARTESIAN_POINT('',(-0.7911,-2.17936779733918E-13,-2.87313315082369));
#61814=CARTESIAN_POINT('',(-0.7911,-9.68818082805471E-17,-5.925));
#61815=CARTESIAN_POINT('Ctrl Pts',(-0.790135803578584,0.000777077086083156,
-2.84466684917631));
#61816=CARTESIAN_POINT('Ctrl Pts',(-0.790729188995581,0.0953959190884639,
-2.8484583444553));
#61817=CARTESIAN_POINT('Ctrl Pts',(-0.775074050339769,0.189770316634575,
-2.8522498397343));
#61818=CARTESIAN_POINT('Ctrl Pts',(-0.742297451277547,0.277572547576085,
-2.85604133501329));
#61819=CARTESIAN_POINT('Ctrl Pts',(-0.650740140155824,0.522837047417337,
-2.86663240067622));
#61820=CARTESIAN_POINT('Ctrl Pts',(-0.425585096270472,0.716819323845514,
-2.87722346633915));
#61821=CARTESIAN_POINT('Ctrl Pts',(-0.169171165385708,0.77368995751212,
-2.88781453200208));
#61822=CARTESIAN_POINT('Ctrl Pts',(-0.040964199943333,0.802125274345422,
-2.89311006483355));
#61823=CARTESIAN_POINT('Ctrl Pts',(0.0950574872488943,0.796282680488336,
-2.89840559766501));
#61824=CARTESIAN_POINT('Ctrl Pts',(0.221595838120345,0.75910254727276,-2.90370113049647));
#61825=CARTESIAN_POINT('Ctrl Pts',(0.348134188991795,0.721922414057184,
-2.90899666332794));
#61826=CARTESIAN_POINT('Ctrl Pts',(0.465189203542468,0.65340474148312,-2.9142921961594));
#61827=CARTESIAN_POINT('Ctrl Pts',(0.558200082457864,0.560909011796547,
-2.91958772899087));
#61828=CARTESIAN_POINT('Ctrl Pts',(0.651210961373282,0.468413282109953,
-2.92488326182233));
#61829=CARTESIAN_POINT('Ctrl Pts',(0.72017770465341,0.351939495310839,-2.9301787946538));
#61830=CARTESIAN_POINT('Ctrl Pts',(0.757953706571736,0.225523681338111,
-2.93547432748526));
#61831=CARTESIAN_POINT('Ctrl Pts',(0.795729708490053,0.0991078673654118,
-2.94076986031673));
#61832=CARTESIAN_POINT('Ctrl Pts',(0.802314969046581,-0.0372499737808963,
-2.94606539314819));
#61833=CARTESIAN_POINT('Ctrl Pts',(0.774549111808285,-0.165620062427354,
-2.95136092597966));
#61834=CARTESIAN_POINT('Ctrl Pts',(0.71901739733169,-0.422360239720285,
-2.96195199164259));
#61835=CARTESIAN_POINT('Ctrl Pts',(0.526081211675783,-0.647149407013813,
-2.97254305730551));
#61836=CARTESIAN_POINT('Ctrl Pts',(0.281004632411375,-0.740545534688081,
-2.98313412296844));
#61837=CARTESIAN_POINT('Ctrl Pts',(0.158466342779164,-0.787243598525218,
-2.98842965579991));
#61838=CARTESIAN_POINT('Ctrl Pts',(0.0228929547448268,-0.801093402457536,
-2.99372518863137));
#61839=CARTESIAN_POINT('Ctrl Pts',(-0.107965886047362,-0.78312720474501,
-2.99902072146284));
#61840=CARTESIAN_POINT('Ctrl Pts',(-0.238824726839536,-0.765161007032487,
-3.0043162542943));
#61841=CARTESIAN_POINT('Ctrl Pts',(-0.364969020389562,-0.715378807675126,
-3.00961178712577));
#61842=CARTESIAN_POINT('Ctrl Pts',(-0.470214481065443,-0.637273548685935,
-3.01490731995723));
#61843=CARTESIAN_POINT('Ctrl Pts',(-0.667365265940161,-0.49096307587624,
-3.02482716303026));
#61844=CARTESIAN_POINT('Ctrl Pts',(-0.791180880172482,-0.245265406483679,
-3.03474700610328));
#61845=CARTESIAN_POINT('Ctrl Pts',(-0.792512397087544,4.98421984640521E-5,
-3.04466684917631));
#61846=CARTESIAN_POINT('Ctrl Pts',(-0.791208548896392,0.000277519652998023,
-3.07313315082369));
#61847=CARTESIAN_POINT('Ctrl Pts',(-0.790944894737022,-0.107710380592565,
-3.06877698009002));
#61848=CARTESIAN_POINT('Ctrl Pts',(-0.768240549118296,-0.215909906892349,
-3.06442080935636));
#61849=CARTESIAN_POINT('Ctrl Pts',(-0.725134083974273,-0.315471001848098,
-3.0600646386227));
#61850=CARTESIAN_POINT('Ctrl Pts',(-0.672732166011195,-0.436501392828995,
-3.05476910579123));
#61851=CARTESIAN_POINT('Ctrl Pts',(-0.590180420560288,-0.544766089811032,
-3.04947357295977));
#61852=CARTESIAN_POINT('Ctrl Pts',(-0.486288498717086,-0.625090817056648,
-3.0441780401283));
#61853=CARTESIAN_POINT('Ctrl Pts',(-0.278504655030694,-0.78574027154787,
-3.03358697446538));
#61854=CARTESIAN_POINT('Ctrl Pts',(0.0146398942248702,-0.83462984709342,
-3.02299590880244));
#61855=CARTESIAN_POINT('Ctrl Pts',(0.261701926009823,-0.748040190941482,
-3.01240484313951));
#61856=CARTESIAN_POINT('Ctrl Pts',(0.508763957794776,-0.661450534789544,
-3.00181377747658));
#61857=CARTESIAN_POINT('Ctrl Pts',(0.709743472109117,-0.439381646940117,
-2.99122271181366));
#61858=CARTESIAN_POINT('Ctrl Pts',(0.770829429168333,-0.184712607043331,
-2.98063164615073));
#61859=CARTESIAN_POINT('Ctrl Pts',(0.831915386227548,0.0699564328534561,
-2.9700405804878));
#61860=CARTESIAN_POINT('Ctrl Pts',(0.753107786031637,0.357225624797604,
-2.95944951482487));
#61861=CARTESIAN_POINT('Ctrl Pts',(0.572517770699919,0.547213519835908,
-2.94885844916194));
#61862=CARTESIAN_POINT('Ctrl Pts',(0.482222763034065,0.642207467355056,
-2.94356291633048));
#61863=CARTESIAN_POINT('Ctrl Pts',(0.366482151584262,0.712881090647745,
-2.93826738349901));
#61864=CARTESIAN_POINT('Ctrl Pts',(0.240641653404015,0.75301822422084,-2.93297185066755));
#61865=CARTESIAN_POINT('Ctrl Pts',(0.114801155223755,0.793155357793939,
-2.92767631783608));
#61866=CARTESIAN_POINT('Ctrl Pts',(-0.0211392296869517,0.802756001647437,
-2.92238078500462));
#61867=CARTESIAN_POINT('Ctrl Pts',(-0.149869697759458,0.777759838302671,
-2.91708525217315));
#61868=CARTESIAN_POINT('Ctrl Pts',(-0.407330633904457,0.727767511613141,
-2.90649418651022));
#61869=CARTESIAN_POINT('Ctrl Pts',(-0.635951902696659,0.539387956130569,
-2.8959031208473));
#61870=CARTESIAN_POINT('Ctrl Pts',(-0.734681805311768,0.295971242902559,
-2.88531205518437));
#61871=CARTESIAN_POINT('Ctrl Pts',(-0.772525716389172,0.202667793733097,
-2.88125242039747));
#61872=CARTESIAN_POINT('Ctrl Pts',(-0.791285386387945,0.101278030456626,
-2.87719278561058));
#61873=CARTESIAN_POINT('Ctrl Pts',(-0.790978541062857,4.5186565332119E-6,
-2.87313315082368));
#61874=CARTESIAN_POINT('Origin',(0.,0.,-5.925));
#61875=CARTESIAN_POINT('',(-0.790765068286233,-0.000289649196591382,-2.64466684917631));
#61876=CARTESIAN_POINT('',(-0.79086137551975,-3.96814382399647E-5,-2.67313315082369));
#61877=CARTESIAN_POINT('',(-0.7911,-9.68818082805471E-17,-5.925));
#61878=CARTESIAN_POINT('Ctrl Pts',(-0.7911,3.66040531218914E-13,-2.64466684917631));
#61879=CARTESIAN_POINT('Ctrl Pts',(-0.791099999999898,0.220167589667046,
-2.65352559274958));
#61880=CARTESIAN_POINT('Ctrl Pts',(-0.694214576672165,0.43861041833901,
-2.66238433632286));
#61881=CARTESIAN_POINT('Ctrl Pts',(-0.531017389080051,0.586395551223409,
-2.67124307989613));
#61882=CARTESIAN_POINT('Ctrl Pts',(-0.367820201487936,0.734180684107808,
-2.6801018234694));
#61883=CARTESIAN_POINT('Ctrl Pts',(-0.140868175871354,0.808992666571405,
-2.68896056704267));
#61884=CARTESIAN_POINT('Ctrl Pts',(0.078220547325147,0.787223447298259,
-2.69781931061595));
#61885=CARTESIAN_POINT('Ctrl Pts',(0.297309270521648,0.765454228025112,
-2.70667805418922));
#61886=CARTESIAN_POINT('Ctrl Pts',(0.505102072675922,0.647444880833977,
-2.71553679776249));
#61887=CARTESIAN_POINT('Ctrl Pts',(0.63602679576197,0.470435038100651,-2.72439554133577));
#61888=CARTESIAN_POINT('Ctrl Pts',(0.766951518848019,0.293425195367324,
-2.73325428490904));
#61889=CARTESIAN_POINT('Ctrl Pts',(0.818956872247102,0.0601881960095046,
-2.74211302848231));
#61890=CARTESIAN_POINT('Ctrl Pts',(0.775631781004128,-0.155674501111659,
-2.75097177205558));
#61891=CARTESIAN_POINT('Ctrl Pts',(0.732306689761154,-0.371537198232823,
-2.75983051562886));
#61892=CARTESIAN_POINT('Ctrl Pts',(0.594329958849911,-0.566643518936817,
-2.76868925920213));
#61893=CARTESIAN_POINT('Ctrl Pts',(0.405242230243673,-0.679424716084964,
-2.7775480027754));
#61894=CARTESIAN_POINT('Ctrl Pts',(0.216154501637436,-0.792205913233111,
-2.78640674634867));
#61895=CARTESIAN_POINT('Ctrl Pts',(-0.0210816529304674,-0.820894963712992,
-2.79526548992195));
#61896=CARTESIAN_POINT('Ctrl Pts',(-0.231602780753636,-0.756438604215295,
-2.80412423349522));
#61897=CARTESIAN_POINT('Ctrl Pts',(-0.442123908576805,-0.691982244717597,
-2.81298297706849));
#61898=CARTESIAN_POINT('Ctrl Pts',(-0.622631625634475,-0.535390358803188,
-2.82184172064176));
#61899=CARTESIAN_POINT('Ctrl Pts',(-0.716163994722344,-0.336077881841895,
-2.83070046421504));
#61900=CARTESIAN_POINT('Ctrl Pts',(-0.765317280859602,-0.23133485751413,
-2.83535592586879));
#61901=CARTESIAN_POINT('Ctrl Pts',(-0.791100000000051,-0.115702837836144,
-2.84001138752255));
#61902=CARTESIAN_POINT('Ctrl Pts',(-0.7911,3.48998607790918E-13,-2.84466684917631));
#61903=CARTESIAN_POINT('Ctrl Pts',(-0.7911,-2.17936779733918E-13,-2.87313315082369));
#61904=CARTESIAN_POINT('Ctrl Pts',(-0.79109999999994,-0.220167589666883,
-2.86427440725041));
#61905=CARTESIAN_POINT('Ctrl Pts',(-0.694214576672262,-0.438610418338851,
-2.85541566367714));
#61906=CARTESIAN_POINT('Ctrl Pts',(-0.531017389080194,-0.58639555122328,
-2.84655692010387));
#61907=CARTESIAN_POINT('Ctrl Pts',(-0.367820201488126,-0.734180684107709,
-2.8376981765306));
#61908=CARTESIAN_POINT('Ctrl Pts',(-0.140868175871583,-0.808992666571361,
-2.82883943295733));
#61909=CARTESIAN_POINT('Ctrl Pts',(0.07822054732491,-0.787223447298283,
-2.81998068938405));
#61910=CARTESIAN_POINT('Ctrl Pts',(0.297309270521403,-0.765454228025204,
-2.81112194581078));
#61911=CARTESIAN_POINT('Ctrl Pts',(0.505102072675699,-0.647444880834146,
-2.80226320223751));
#61912=CARTESIAN_POINT('Ctrl Pts',(0.636026795761802,-0.470435038100878,
-2.79340445866424));
#61913=CARTESIAN_POINT('Ctrl Pts',(0.766951518847905,-0.293425195367611,
-2.78454571509097));
#61914=CARTESIAN_POINT('Ctrl Pts',(0.818956872247075,-0.0601881960098297,
-2.77568697151769));
#61915=CARTESIAN_POINT('Ctrl Pts',(0.775631781004193,0.155674501111338,
-2.76682822794442));
#61916=CARTESIAN_POINT('Ctrl Pts',(0.732306689761311,0.371537198232505,
-2.75796948437115));
#61917=CARTESIAN_POINT('Ctrl Pts',(0.594329958850165,0.566643518936544,
-2.74911074079788));
#61918=CARTESIAN_POINT('Ctrl Pts',(0.405242230243994,0.679424716084773,
-2.74025199722461));
#61919=CARTESIAN_POINT('Ctrl Pts',(0.216154501637822,0.792205913233001,
-2.73139325365133));
#61920=CARTESIAN_POINT('Ctrl Pts',(-0.021081652930048,0.820894963712999,
-2.72253451007806));
#61921=CARTESIAN_POINT('Ctrl Pts',(-0.231602780753237,0.756438604215417,
-2.71367576650479));
#61922=CARTESIAN_POINT('Ctrl Pts',(-0.442123908576425,0.691982244717835,
-2.70481702293152));
#61923=CARTESIAN_POINT('Ctrl Pts',(-0.622631625634168,0.535390358803539,
-2.69595827935824));
#61924=CARTESIAN_POINT('Ctrl Pts',(-0.716163994722147,0.336077881842314,
-2.68709953578497));
#61925=CARTESIAN_POINT('Ctrl Pts',(-0.765317280859505,0.231334857514496,
-2.68244407413121));
#61926=CARTESIAN_POINT('Ctrl Pts',(-0.791100000000023,0.115702837836428,
-2.67778861247745));
#61927=CARTESIAN_POINT('Ctrl Pts',(-0.7911,-1.55819801506141E-13,-2.67313315082369));
#61928=CARTESIAN_POINT('Origin',(0.,0.,-5.925));
#61929=CARTESIAN_POINT('',(-0.792018129320091,-0.000125529594581231,-2.44466684917631));
#61930=CARTESIAN_POINT('',(-0.792074714116757,-0.00038587903788701,-2.47313315082369));
#61931=CARTESIAN_POINT('',(-0.7911,-9.68818082805471E-17,-5.925));
#61932=CARTESIAN_POINT('Ctrl Pts',(-0.792018129320091,-0.000125529594581231,
-2.44466684917631));
#61933=CARTESIAN_POINT('Ctrl Pts',(-0.791984392204006,0.11739493153915,
-2.44940335700203));
#61934=CARTESIAN_POINT('Ctrl Pts',(-0.764359052987853,0.23524448466125,
-2.45413986482774));
#61935=CARTESIAN_POINT('Ctrl Pts',(-0.713221964095025,0.341549151193039,
-2.45887637265346));
#61936=CARTESIAN_POINT('Ctrl Pts',(-0.656049434648901,0.460400396133606,
-2.46417190548492));
#61937=CARTESIAN_POINT('Ctrl Pts',(-0.569487705445131,0.564820772132129,
-2.46946743831638));
#61938=CARTESIAN_POINT('Ctrl Pts',(-0.463156154873996,0.641632782651323,
-2.47476297114785));
#61939=CARTESIAN_POINT('Ctrl Pts',(-0.356824604302849,0.718444793170525,
-2.48005850397931));
#61940=CARTESIAN_POINT('Ctrl Pts',(-0.23072323236434,0.767648438210387,
-2.48535403681077));
#61941=CARTESIAN_POINT('Ctrl Pts',(-0.0998597826367812,0.784463368145296,
-2.49064956964224));
#61942=CARTESIAN_POINT('Ctrl Pts',(0.0310036670907922,0.801278298080207,
-2.4959451024737));
#61943=CARTESIAN_POINT('Ctrl Pts',(0.166629194607407,0.785704512910156,
-2.50124063530517));
#61944=CARTESIAN_POINT('Ctrl Pts',(0.288811906477642,0.737525602510308,
-2.50653616813664));
#61945=CARTESIAN_POINT('Ctrl Pts',(0.533177330218084,0.641167781710625,
-2.51712723379956));
#61946=CARTESIAN_POINT('Ctrl Pts',(0.72377149137302,0.414389459991754,-2.52771829946249));
#61947=CARTESIAN_POINT('Ctrl Pts',(0.776265456590592,0.157426914113526,
-2.53830936512542));
#61948=CARTESIAN_POINT('Ctrl Pts',(0.802512439199381,0.0289456411743981,
-2.54360489795689));
#61949=CARTESIAN_POINT('Ctrl Pts',(0.794234372823836,-0.107081687804533,
-2.54890043078835));
#61950=CARTESIAN_POINT('Ctrl Pts',(0.755323031929162,-0.23330659827588,
-2.55419596361981));
#61951=CARTESIAN_POINT('Ctrl Pts',(0.716411691034492,-0.359531508747212,
-2.55949149645128));
#61952=CARTESIAN_POINT('Ctrl Pts',(0.646867075620673,-0.475954000710952,
-2.56478702928274));
#61953=CARTESIAN_POINT('Ctrl Pts',(0.5527558084356,-0.56716862598271,-2.57008256211421));
#61954=CARTESIAN_POINT('Ctrl Pts',(0.364533274065442,-0.749597876526237,
-2.58067362777714));
#61955=CARTESIAN_POINT('Ctrl Pts',(0.0780441326101909,-0.831195660301974,
-2.59126469344007));
#61956=CARTESIAN_POINT('Ctrl Pts',(-0.177206969668502,-0.772589442054205,
-2.601855759103));
#61957=CARTESIAN_POINT('Ctrl Pts',(-0.432458071947195,-0.713983223806436,
-2.61244682476593));
#61958=CARTESIAN_POINT('Ctrl Pts',(-0.656471135049315,-0.515173003535163,
-2.62303789042885));
#61959=CARTESIAN_POINT('Ctrl Pts',(-0.745459561574409,-0.268964806988401,
-2.63362895609178));
#61960=CARTESIAN_POINT('Ctrl Pts',(-0.7763738173256,-0.183432974891788,
-2.63730825378663));
#61961=CARTESIAN_POINT('Ctrl Pts',(-0.790992728343168,-0.0921809543713075,
-2.64098755148147));
#61962=CARTESIAN_POINT('Ctrl Pts',(-0.790257091081424,-0.000728948263829188,
-2.64466684917631));
#61963=CARTESIAN_POINT('Ctrl Pts',(-0.789984210644415,-0.000185547291381985,
-2.67313315082369));
#61964=CARTESIAN_POINT('Ctrl Pts',(-0.790630089050473,-0.0849598024118021,
-2.66972199263674));
#61965=CARTESIAN_POINT('Ctrl Pts',(-0.778080687464463,-0.169671162325107,
-2.6663108344498));
#61966=CARTESIAN_POINT('Ctrl Pts',(-0.751565426157115,-0.250011483509697,
-2.66289967626285));
#61967=CARTESIAN_POINT('Ctrl Pts',(-0.710402739147965,-0.374732996030462,
-2.65760414343139));
#61968=CARTESIAN_POINT('Ctrl Pts',(-0.63558244117862,-0.488920339945901,
-2.65230861059992));
#61969=CARTESIAN_POINT('Ctrl Pts',(-0.538920306497888,-0.578722433809465,
-2.64701307776846));
#61970=CARTESIAN_POINT('Ctrl Pts',(-0.442258171817167,-0.668524527673019,
-2.64171754493699));
#61971=CARTESIAN_POINT('Ctrl Pts',(-0.323754200425058,-0.733941371484708,
-2.63642201210553));
#61972=CARTESIAN_POINT('Ctrl Pts',(-0.196685444636518,-0.766499241642599,
-2.63112647927406));
#61973=CARTESIAN_POINT('Ctrl Pts',(-0.0696166888479782,-0.79905711180049,
-2.6258309464426));
#61974=CARTESIAN_POINT('Ctrl Pts',(0.0660168513370011,-0.798756008304586,
-2.62053541361114));
#61975=CARTESIAN_POINT('Ctrl Pts',(0.193933392624089,-0.766636310106404,
-2.61523988077967));
#61976=CARTESIAN_POINT('Ctrl Pts',(0.321849933911193,-0.734516611908218,
-2.60994434794821));
#61977=CARTESIAN_POINT('Ctrl Pts',(0.442049476300412,-0.670578319007744,
-2.60464881511674));
#61978=CARTESIAN_POINT('Ctrl Pts',(0.538131844813672,-0.581058646911393,
-2.59935328228528));
#61979=CARTESIAN_POINT('Ctrl Pts',(0.730296581840193,-0.402019302718692,
-2.58876221662235));
#61980=CARTESIAN_POINT('Ctrl Pts',(0.82599262336289,-0.12065444174251,-2.57817115095942));
#61981=CARTESIAN_POINT('Ctrl Pts',(0.780536751463461,0.137165611418776,
-2.56758008529649));
#61982=CARTESIAN_POINT('Ctrl Pts',(0.735080879564037,0.394985664580032,
-2.55698901963356));
#61983=CARTESIAN_POINT('Ctrl Pts',(0.548473094242492,0.629260909926376,
-2.54639795397063));
#61984=CARTESIAN_POINT('Ctrl Pts',(0.307050557510526,0.730764470404245,
-2.53580688830771));
#61985=CARTESIAN_POINT('Ctrl Pts',(0.065628020778533,0.832268030882126,
-2.52521582264478));
#61986=CARTESIAN_POINT('Ctrl Pts',(-0.230609267363913,0.800999906491504,
-2.51462475698184));
#61987=CARTESIAN_POINT('Ctrl Pts',(-0.447323677468425,0.653544766358459,
-2.50403369131891));
#61988=CARTESIAN_POINT('Ctrl Pts',(-0.555680882520669,0.579817196291946,
-2.49873815848745));
#61989=CARTESIAN_POINT('Ctrl Pts',(-0.644157368063439,0.47704287228983,
-2.49344262565599));
#61990=CARTESIAN_POINT('Ctrl Pts',(-0.704134940177837,0.359358925563953,
-2.48814709282452));
#61991=CARTESIAN_POINT('Ctrl Pts',(-0.760817922969531,0.248139399798586,
-2.48314244549091));
#61992=CARTESIAN_POINT('Ctrl Pts',(-0.792046912168715,0.123603245585912,
-2.4781377981573));
#61993=CARTESIAN_POINT('Ctrl Pts',(-0.792074714116757,-0.00038587903788701,
-2.47313315082369));
#61994=CARTESIAN_POINT('Origin',(0.,0.,-5.925));
#61995=CARTESIAN_POINT('',(-0.791060221705291,6.8858939410166E-5,-2.24466684917632));
#61996=CARTESIAN_POINT('',(-0.791211456379323,0.000596892318849943,-2.27313315082369));
#61997=CARTESIAN_POINT('',(-0.7911,-9.68818082805471E-17,-5.925));
#61998=CARTESIAN_POINT('Ctrl Pts',(-0.790839757919185,0.000450496766933234,
-2.24466684917631));
#61999=CARTESIAN_POINT('Ctrl Pts',(-0.790967177237201,0.0640755268736169,
-2.24722809685965));
#62000=CARTESIAN_POINT('Ctrl Pts',(-0.783524433324388,0.127612789595849,
-2.24978934454299));
#62001=CARTESIAN_POINT('Ctrl Pts',(-0.768375904261664,0.189221355350329,
-2.25235059222633));
#62002=CARTESIAN_POINT('Ctrl Pts',(-0.737055414048305,0.31660075124959,
-2.2576461250578));
#62003=CARTESIAN_POINT('Ctrl Pts',(-0.672794205261668,0.435735346289252,
-2.26294165788926));
#62004=CARTESIAN_POINT('Ctrl Pts',(-0.583936471318637,0.533266302717569,
-2.26823719072073));
#62005=CARTESIAN_POINT('Ctrl Pts',(-0.495078737375595,0.630797259145896,
-2.27353272355219));
#62006=CARTESIAN_POINT('Ctrl Pts',(-0.381624478276152,0.706724576962874,
-2.27882825638366));
#62007=CARTESIAN_POINT('Ctrl Pts',(-0.257309202990711,0.749098328484138,
-2.28412378921512));
#62008=CARTESIAN_POINT('Ctrl Pts',(-0.00867865241984256,0.833845831526662,
-2.29471485487805));
#62009=CARTESIAN_POINT('Ctrl Pts',(0.283395962895014,0.78437906938635,-2.30530592054098));
#62010=CARTESIAN_POINT('Ctrl Pts',(0.489751707774617,0.62250667234573,-2.31589698620391));
#62011=CARTESIAN_POINT('Ctrl Pts',(0.592929580214424,0.541570473825415,
-2.32119251903537));
#62012=CARTESIAN_POINT('Ctrl Pts',(0.674677735045415,0.43253286658002,-2.32648805186684));
#62013=CARTESIAN_POINT('Ctrl Pts',(0.726731869991776,0.311136048216823,
-2.3317835846983));
#62014=CARTESIAN_POINT('Ctrl Pts',(0.778786004938132,0.189739229853641,
-2.33707911752977));
#62015=CARTESIAN_POINT('Ctrl Pts',(0.801146119999865,0.0559832003726588,
-2.34237465036123));
#62016=CARTESIAN_POINT('Ctrl Pts',(0.788463385113155,-0.074462906163491,
-2.3476701831927));
#62017=CARTESIAN_POINT('Ctrl Pts',(0.763097915339735,-0.335355119235806,
-2.35826124885562));
#62018=CARTESIAN_POINT('Ctrl Pts',(0.597561045772532,-0.583007640528791,
-2.36885231451856));
#62019=CARTESIAN_POINT('Ctrl Pts',(0.365072122371674,-0.70357593871576,
-2.37944338018149));
#62020=CARTESIAN_POINT('Ctrl Pts',(0.132583198970817,-0.824144236902728,
-2.39003444584441));
#62021=CARTESIAN_POINT('Ctrl Pts',(-0.166857778263693,-0.817628311983679,
-2.40062551150734));
#62022=CARTESIAN_POINT('Ctrl Pts',(-0.394067412302621,-0.687577559190332,
-2.41121657717027));
#62023=CARTESIAN_POINT('Ctrl Pts',(-0.621277046341549,-0.557526806396985,
-2.4218076428332));
#62024=CARTESIAN_POINT('Ctrl Pts',(-0.776255337184895,-0.303941225729339,
-2.43239870849613));
#62025=CARTESIAN_POINT('Ctrl Pts',(-0.790870327881392,-0.0417032136632777,
-2.44298977415906));
#62026=CARTESIAN_POINT('Ctrl Pts',(-0.791641746501405,-0.0278615842306018,
-2.44354879916481));
#62027=CARTESIAN_POINT('Ctrl Pts',(-0.792022111133741,-0.0139958490110292,
-2.44410782417056));
#62028=CARTESIAN_POINT('Ctrl Pts',(-0.792018129320091,-0.000125529594581231,
-2.44466684917631));
#62029=CARTESIAN_POINT('Ctrl Pts',(-0.792074714116757,-0.00038587903788701,
-2.47313315082369));
#62030=CARTESIAN_POINT('Ctrl Pts',(-0.792076330051498,-0.00759250836469937,
-2.47284226532584));
#62031=CARTESIAN_POINT('Ctrl Pts',(-0.791972539265708,-0.0147972896658409,
-2.47255137982798));
#62032=CARTESIAN_POINT('Ctrl Pts',(-0.791762213259279,-0.02199750071887,
-2.47226049433013));
#62033=CARTESIAN_POINT('Ctrl Pts',(-0.784104297821294,-0.284155320933407,
-2.4616694286672));
#62034=CARTESIAN_POINT('Ctrl Pts',(-0.635215916763238,-0.540254503778407,
-2.45107836300427));
#62035=CARTESIAN_POINT('Ctrl Pts',(-0.410990726089976,-0.67708415632732,
-2.44048729734134));
#62036=CARTESIAN_POINT('Ctrl Pts',(-0.298878130753351,-0.745498982601772,
-2.43519176450988));
#62037=CARTESIAN_POINT('Ctrl Pts',(-0.167931333012931,-0.784096426302203,
-2.42989623167841));
#62038=CARTESIAN_POINT('Ctrl Pts',(-0.0361227386238225,-0.789968290442371,
-2.42460069884695));
#62039=CARTESIAN_POINT('Ctrl Pts',(0.0956858557653013,-0.79584015458254,
-2.41930516601548));
#62040=CARTESIAN_POINT('Ctrl Pts',(0.228356246803106,-0.768986439162439,
-2.41400963318402));
#62041=CARTESIAN_POINT('Ctrl Pts',(0.346283301642012,-0.711543481857892,
-2.40871410035255));
#62042=CARTESIAN_POINT('Ctrl Pts',(0.464210356480919,-0.654100524553346,
-2.40341856752109));
#62043=CARTESIAN_POINT('Ctrl Pts',(0.567394075120918,-0.566068325364358,
-2.39812303468962));
#62044=CARTESIAN_POINT('Ctrl Pts',(0.644098123696367,-0.458779903438533,
-2.39282750185816));
#62045=CARTESIAN_POINT('Ctrl Pts',(0.720802172271807,-0.35149148151272,
-2.38753196902669));
#62046=CARTESIAN_POINT('Ctrl Pts',(0.771026550782695,-0.224946836850083,
-2.38223643619523));
#62047=CARTESIAN_POINT('Ctrl Pts',(0.786308873044694,-0.0945166108377294,
-2.37694090336377));
#62048=CARTESIAN_POINT('Ctrl Pts',(0.816873517568692,0.166343841186993,
-2.36634983770084));
#62049=CARTESIAN_POINT('Ctrl Pts',(0.707669937097088,0.442746618610588,
-2.35575877203791));
#62050=CARTESIAN_POINT('Ctrl Pts',(0.506123452891804,0.609828726589603,
-2.34516770637498));
#62051=CARTESIAN_POINT('Ctrl Pts',(0.304576968686531,0.776910834568609,
-2.33457664071205));
#62052=CARTESIAN_POINT('Ctrl Pts',(0.0106875807475982,0.834672273103086,
-2.32398557504912));
#62053=CARTESIAN_POINT('Ctrl Pts',(-0.239031035420305,0.755751890621927,
-2.31339450938619));
#62054=CARTESIAN_POINT('Ctrl Pts',(-0.488749651588223,0.676831508140765,
-2.30280344372326));
#62055=CARTESIAN_POINT('Ctrl Pts',(-0.694297495985092,0.461229304643954,
-2.29221237806033));
#62056=CARTESIAN_POINT('Ctrl Pts',(-0.764019786897861,0.208549752545901,
-2.2816213123974));
#62057=CARTESIAN_POINT('Ctrl Pts',(-0.782645991581197,0.141046791942381,
-2.27879192520617));
#62058=CARTESIAN_POINT('Ctrl Pts',(-0.791578555337622,0.0708976834333845,
-2.27596253801493));
#62059=CARTESIAN_POINT('Ctrl Pts',(-0.791211456379323,0.000596892318849943,
-2.27313315082369));
#62060=CARTESIAN_POINT('Origin',(0.,0.,-5.925));
#62061=CARTESIAN_POINT('',(-0.7911,4.17277323805365E-13,-2.04466684917631));
#62062=CARTESIAN_POINT('',(-0.78949630379784,-0.000100922603766505,-2.07313315082369));
#62063=CARTESIAN_POINT('',(-0.7911,-9.68818082805471E-17,-5.925));
#62064=CARTESIAN_POINT('Ctrl Pts',(-0.7911,4.17277323805365E-13,-2.04466684917631));
#62065=CARTESIAN_POINT('Ctrl Pts',(-0.791099999999884,0.220167589667097,
-2.05352559274959));
#62066=CARTESIAN_POINT('Ctrl Pts',(-0.694214576672137,0.438610418339055,
-2.06238433632286));
#62067=CARTESIAN_POINT('Ctrl Pts',(-0.531017389080013,0.586395551223444,
-2.07124307989613));
#62068=CARTESIAN_POINT('Ctrl Pts',(-0.367820201487889,0.734180684107832,
-2.0801018234694));
#62069=CARTESIAN_POINT('Ctrl Pts',(-0.140868175871302,0.808992666571414,
-2.08896056704268));
#62070=CARTESIAN_POINT('Ctrl Pts',(0.0782205473251979,0.787223447298254,
-2.09781931061595));
#62071=CARTESIAN_POINT('Ctrl Pts',(0.297309270521698,0.765454228025093,
-2.10667805418922));
#62072=CARTESIAN_POINT('Ctrl Pts',(0.505102072675964,0.647444880833945,
-2.11553679776249));
#62073=CARTESIAN_POINT('Ctrl Pts',(0.636026795762001,0.47043503810061,-2.12439554133577));
#62074=CARTESIAN_POINT('Ctrl Pts',(0.766951518848038,0.293425195367275,
-2.13325428490904));
#62075=CARTESIAN_POINT('Ctrl Pts',(0.818956872247106,0.0601881960094517,
-2.14211302848231));
#62076=CARTESIAN_POINT('Ctrl Pts',(0.775631781004118,-0.155674501111709,
-2.15097177205558));
#62077=CARTESIAN_POINT('Ctrl Pts',(0.73230668976113,-0.371537198232871,
-2.15983051562886));
#62078=CARTESIAN_POINT('Ctrl Pts',(0.594329958849874,-0.566643518936855,
-2.16868925920213));
#62079=CARTESIAN_POINT('Ctrl Pts',(0.405242230243629,-0.67942471608499,
-2.1775480027754));
#62080=CARTESIAN_POINT('Ctrl Pts',(0.216154501637384,-0.792205913233125,
-2.18640674634868));
#62081=CARTESIAN_POINT('Ctrl Pts',(-0.0210816529305205,-0.820894963712991,
-2.19526548992195));
#62082=CARTESIAN_POINT('Ctrl Pts',(-0.231602780753685,-0.75643860421528,
-2.20412423349522));
#62083=CARTESIAN_POINT('Ctrl Pts',(-0.44212390857685,-0.691982244717568,
-2.21298297706849));
#62084=CARTESIAN_POINT('Ctrl Pts',(-0.62263162563451,-0.535390358803148,
-2.22184172064177));
#62085=CARTESIAN_POINT('Ctrl Pts',(-0.716163994722366,-0.336077881841848,
-2.23070046421504));
#62086=CARTESIAN_POINT('Ctrl Pts',(-0.765317280859623,-0.231334857514067,
-2.2353559258688));
#62087=CARTESIAN_POINT('Ctrl Pts',(-0.791100000000065,-0.115702837836063,
-2.24001138752256));
#62088=CARTESIAN_POINT('Ctrl Pts',(-0.7911,4.45199432874688E-13,-2.24466684917631));
#62089=CARTESIAN_POINT('Ctrl Pts',(-0.791211456379323,0.000596892318849943,
-2.27313315082369));
#62090=CARTESIAN_POINT('Ctrl Pts',(-0.790891486211103,-0.0606785633870678,
-2.27066700518346));
#62091=CARTESIAN_POINT('Ctrl Pts',(-0.783506390675429,-0.122069255167356,
-2.26820085954324));
#62092=CARTESIAN_POINT('Ctrl Pts',(-0.769317056038747,-0.181923386758272,
-2.26573471390301));
#62093=CARTESIAN_POINT('Ctrl Pts',(-0.738848422637895,-0.310447636814053,
-2.26043918107154));
#62094=CARTESIAN_POINT('Ctrl Pts',(-0.677006398750834,-0.431887023726298,
-2.25514364824008));
#62095=CARTESIAN_POINT('Ctrl Pts',(-0.589233752287982,-0.529315480170128,
-2.24984811540861));
#62096=CARTESIAN_POINT('Ctrl Pts',(-0.413688459362257,-0.724172393057811,
-2.23925704974568));
#62097=CARTESIAN_POINT('Ctrl Pts',(-0.134420676133361,-0.822985584071841,
-2.22866598408276));
#62098=CARTESIAN_POINT('Ctrl Pts',(0.125058712097984,-0.782123168183783,
-2.21807491841983));
#62099=CARTESIAN_POINT('Ctrl Pts',(0.254798406213642,-0.761691960239756,
-2.21277938558836));
#62100=CARTESIAN_POINT('Ctrl Pts',(0.37959100157991,-0.706341850570208,
-2.2074838527569));
#62101=CARTESIAN_POINT('Ctrl Pts',(0.48385546721716,-0.625490718551596,
-2.20218831992543));
#62102=CARTESIAN_POINT('Ctrl Pts',(0.588119932854422,-0.544639586532975,
-2.19689278709397));
#62103=CARTESIAN_POINT('Ctrl Pts',(0.671856268762669,-0.438287432165276,
-2.19159725426251));
#62104=CARTESIAN_POINT('Ctrl Pts',(0.724553349368237,-0.318164572964707,
-2.18630172143104));
#62105=CARTESIAN_POINT('Ctrl Pts',(0.777250429973799,-0.198041713764152,
-2.18100618859958));
#62106=CARTESIAN_POINT('Ctrl Pts',(0.798908255276695,-0.0641481497307185,
-2.17571065576811));
#62107=CARTESIAN_POINT('Ctrl Pts',(0.787917956791281,0.0672806518555208,
-2.17041512293665));
#62108=CARTESIAN_POINT('Ctrl Pts',(0.776927658305866,0.198709453441775,
-2.16511959010518));
#62109=CARTESIAN_POINT('Ctrl Pts',(0.733289236032133,0.327673492580847,
-2.15982405727372));
#62110=CARTESIAN_POINT('Ctrl Pts',(0.660502958879976,0.436979261365872,
-2.15452852444225));
#62111=CARTESIAN_POINT('Ctrl Pts',(0.514930404575669,0.655590798935909,
-2.14393745877932));
#62112=CARTESIAN_POINT('Ctrl Pts',(0.252766430757701,0.79556925508978,-2.1333463931164));
#62113=CARTESIAN_POINT('Ctrl Pts',(-0.00901145599943075,0.792446098483543,
-2.12275532745347));
#62114=CARTESIAN_POINT('Ctrl Pts',(-0.270789342756577,0.789322941877306,
-2.11216426179054));
#62115=CARTESIAN_POINT('Ctrl Pts',(-0.532181142452879,0.643098172510908,
-2.10157319612761));
#62116=CARTESIAN_POINT('Ctrl Pts',(-0.671425077549028,0.421289830533569,
-2.09098213046468));
#62117=CARTESIAN_POINT('Ctrl Pts',(-0.749647050727828,0.296686298142697,
-2.08503247058435));
#62118=CARTESIAN_POINT('Ctrl Pts',(-0.789322001462229,0.148230349834439,
-2.07908281070402));
#62119=CARTESIAN_POINT('Ctrl Pts',(-0.78949630379784,-0.000100922603766505,
-2.07313315082369));
#62120=CARTESIAN_POINT('Origin',(0.,0.,-5.925));
#62121=CARTESIAN_POINT('',(-0.7911,4.34319247233361E-13,-1.84466684917631));
#62122=CARTESIAN_POINT('',(-0.7914071948316,-0.000324170431651095,-1.87313315082369));
#62123=CARTESIAN_POINT('',(-0.7911,-9.68818082805471E-17,-5.925));
#62124=CARTESIAN_POINT('Ctrl Pts',(-0.7911,4.34319247233361E-13,-1.84466684917631));
#62125=CARTESIAN_POINT('Ctrl Pts',(-0.791099999999879,0.220167589667114,
-1.85352559274959));
#62126=CARTESIAN_POINT('Ctrl Pts',(-0.694214576672128,0.43861041833907,
-1.86238433632286));
#62127=CARTESIAN_POINT('Ctrl Pts',(-0.53101738908,0.586395551223455,-1.87124307989613));
#62128=CARTESIAN_POINT('Ctrl Pts',(-0.367820201487873,0.73418068410784,
-1.8801018234694));
#62129=CARTESIAN_POINT('Ctrl Pts',(-0.140868175871284,0.808992666571417,
-1.88896056704268));
#62130=CARTESIAN_POINT('Ctrl Pts',(0.0782205473252149,0.787223447298252,
-1.89781931061595));
#62131=CARTESIAN_POINT('Ctrl Pts',(0.297309270521714,0.765454228025087,
-1.90667805418922));
#62132=CARTESIAN_POINT('Ctrl Pts',(0.505102072675978,0.647444880833934,
-1.9155367977625));
#62133=CARTESIAN_POINT('Ctrl Pts',(0.636026795762011,0.470435038100596,
-1.92439554133577));
#62134=CARTESIAN_POINT('Ctrl Pts',(0.766951518848044,0.293425195367258,
-1.93325428490904));
#62135=CARTESIAN_POINT('Ctrl Pts',(0.818956872247108,0.060188196009434,
-1.94211302848231));
#62136=CARTESIAN_POINT('Ctrl Pts',(0.775631781004115,-0.155674501111726,
-1.95097177205558));
#62137=CARTESIAN_POINT('Ctrl Pts',(0.732306689761122,-0.371537198232887,
-1.95983051562886));
#62138=CARTESIAN_POINT('Ctrl Pts',(0.594329958849862,-0.566643518936868,
-1.96868925920213));
#62139=CARTESIAN_POINT('Ctrl Pts',(0.405242230243615,-0.679424716084999,
-1.9775480027754));
#62140=CARTESIAN_POINT('Ctrl Pts',(0.216154501637367,-0.79220591323313,
-1.98640674634868));
#62141=CARTESIAN_POINT('Ctrl Pts',(-0.0210816529305382,-0.82089496371299,
-1.99526548992195));
#62142=CARTESIAN_POINT('Ctrl Pts',(-0.231602780753701,-0.756438604215275,
-2.00412423349522));
#62143=CARTESIAN_POINT('Ctrl Pts',(-0.442123908576865,-0.691982244717559,
-2.0129829770685));
#62144=CARTESIAN_POINT('Ctrl Pts',(-0.622631625634521,-0.535390358803134,
-2.02184172064177));
#62145=CARTESIAN_POINT('Ctrl Pts',(-0.716163994722373,-0.336077881841833,
-2.03070046421504));
#62146=CARTESIAN_POINT('Ctrl Pts',(-0.765317280859622,-0.231334857514064,
-2.0353559258688));
#62147=CARTESIAN_POINT('Ctrl Pts',(-0.791100000000061,-0.115702837836076,
-2.04001138752256));
#62148=CARTESIAN_POINT('Ctrl Pts',(-0.7911,4.17277323805365E-13,-2.04466684917631));
#62149=CARTESIAN_POINT('Ctrl Pts',(-0.78949630379784,-0.000100922603766505,
-2.07313315082369));
#62150=CARTESIAN_POINT('Ctrl Pts',(-0.78963227927958,-0.115816045734007,
-2.06849174504109));
#62151=CARTESIAN_POINT('Ctrl Pts',(-0.765729109396082,-0.23145529412585,
-2.06385033925849));
#62152=CARTESIAN_POINT('Ctrl Pts',(-0.717334052693458,-0.33563535407461,
-2.05920893347589));
#62153=CARTESIAN_POINT('Ctrl Pts',(-0.662118537469595,-0.454497818095894,
-2.05391340064442));
#62154=CARTESIAN_POINT('Ctrl Pts',(-0.575021247009803,-0.558443535480751,
-2.04861786781296));
#62155=CARTESIAN_POINT('Ctrl Pts',(-0.468597849765866,-0.636679594895684,
-2.0433223349815));
#62156=CARTESIAN_POINT('Ctrl Pts',(-0.362174452521929,-0.714915654310618,
-2.03802680215003));
#62157=CARTESIAN_POINT('Ctrl Pts',(-0.23642494849386,-0.767442055755619,
-2.03273126931857));
#62158=CARTESIAN_POINT('Ctrl Pts',(-0.106454896091932,-0.784881295153073,
-2.0274357364871));
#62159=CARTESIAN_POINT('Ctrl Pts',(0.15348520871194,-0.819759773947982,
-2.01684467082417));
#62160=CARTESIAN_POINT('Ctrl Pts',(0.430307507011247,-0.71428960455265,
-2.00625360516124));
#62161=CARTESIAN_POINT('Ctrl Pts',(0.60162792982051,-0.515170035756479,
-1.99566253949832));
#62162=CARTESIAN_POINT('Ctrl Pts',(0.687288141225137,-0.415610251358399,
-1.99036700666685));
#62163=CARTESIAN_POINT('Ctrl Pts',(0.746572883757262,-0.292638117110115,
-1.98507147383539));
#62164=CARTESIAN_POINT('Ctrl Pts',(0.773703125728235,-0.163518272338253,
-1.97977594100392));
#62165=CARTESIAN_POINT('Ctrl Pts',(0.800833367699212,-0.0343984275663764,
-1.97448040817246));
#62166=CARTESIAN_POINT('Ctrl Pts',(0.795809109109027,0.100869127729068,
-1.96918487534099));
#62167=CARTESIAN_POINT('Ctrl Pts',(0.758212516041847,0.226539250656562,
-1.96388934250953));
#62168=CARTESIAN_POINT('Ctrl Pts',(0.720615922974666,0.352209373584056,
-1.95859380967806));
#62169=CARTESIAN_POINT('Ctrl Pts',(0.650446995430492,0.468282064143586,
-1.9532982768466));
#62170=CARTESIAN_POINT('Ctrl Pts',(0.556989537706041,0.561341293362837,
-1.94800274401513));
#62171=CARTESIAN_POINT('Ctrl Pts',(0.46353207998161,0.654400522582066,-1.94270721118367));
#62172=CARTESIAN_POINT('Ctrl Pts',(0.346786092076882,0.724446290461038,
-1.9374116783522));
#62173=CARTESIAN_POINT('Ctrl Pts',(0.220549705811982,0.760639770732056,
-1.93211614552074));
#62174=CARTESIAN_POINT('Ctrl Pts',(-0.0319230667178758,0.833026731274109,
-1.92152507985781));
#62175=CARTESIAN_POINT('Ctrl Pts',(-0.322357432688538,0.77000454138438,
-1.91093401419488));
#62176=CARTESIAN_POINT('Ctrl Pts',(-0.519860350901303,0.598161550838729,
-1.90034294853195));
#62177=CARTESIAN_POINT('Ctrl Pts',(-0.688997074953855,0.450999368450243,
-1.89127301596253));
#62178=CARTESIAN_POINT('Ctrl Pts',(-0.78997977571041,0.224030236294755,
-1.88220308339311));
#62179=CARTESIAN_POINT('Ctrl Pts',(-0.791972689379438,-0.000920914233180042,
-1.87313315082369));
#62180=CARTESIAN_POINT('Origin',(0.,0.,-5.925));
#62181=CARTESIAN_POINT('',(-0.7911,4.51416681812589E-13,-1.64466684917631));
#62182=CARTESIAN_POINT('',(-0.7911,-1.15518705712248E-13,-1.67313315082369));
#62183=CARTESIAN_POINT('',(-0.7911,-9.68818082805471E-17,-5.925));
#62184=CARTESIAN_POINT('Ctrl Pts',(-0.7911,4.51416681812589E-13,-1.64466684917631));
#62185=CARTESIAN_POINT('Ctrl Pts',(-0.791099999999874,0.220167589667131,
-1.65352559274959));
#62186=CARTESIAN_POINT('Ctrl Pts',(-0.694214576672118,0.438610418339085,
-1.66238433632286));
#62187=CARTESIAN_POINT('Ctrl Pts',(-0.531017389079988,0.586395551223466,
-1.67124307989613));
#62188=CARTESIAN_POINT('Ctrl Pts',(-0.367820201487857,0.734180684107848,
-1.6801018234694));
#62189=CARTESIAN_POINT('Ctrl Pts',(-0.140868175871267,0.80899266657142,
-1.68896056704268));
#62190=CARTESIAN_POINT('Ctrl Pts',(0.0782205473252319,0.78722344729825,
-1.69781931061595));
#62191=CARTESIAN_POINT('Ctrl Pts',(0.297309270521731,0.76545422802508,-1.70667805418922));
#62192=CARTESIAN_POINT('Ctrl Pts',(0.505102072675992,0.647444880833923,
-1.7155367977625));
#62193=CARTESIAN_POINT('Ctrl Pts',(0.636026795762021,0.470435038100582,
-1.72439554133577));
#62194=CARTESIAN_POINT('Ctrl Pts',(0.76695151884805,0.293425195367242,-1.73325428490904));
#62195=CARTESIAN_POINT('Ctrl Pts',(0.818956872247109,0.0601881960094164,
-1.74211302848231));
#62196=CARTESIAN_POINT('Ctrl Pts',(0.775631781004111,-0.155674501111743,
-1.75097177205559));
#62197=CARTESIAN_POINT('Ctrl Pts',(0.732306689761114,-0.371537198232902,
-1.75983051562886));
#62198=CARTESIAN_POINT('Ctrl Pts',(0.59432995884985,-0.566643518936881,
-1.76868925920213));
#62199=CARTESIAN_POINT('Ctrl Pts',(0.4052422302436,-0.679424716085008,-1.7775480027754));
#62200=CARTESIAN_POINT('Ctrl Pts',(0.21615450163735,-0.792205913233134,
-1.78640674634868));
#62201=CARTESIAN_POINT('Ctrl Pts',(-0.021081652930556,-0.82089496371299,
-1.79526548992195));
#62202=CARTESIAN_POINT('Ctrl Pts',(-0.231602780753718,-0.75643860421527,
-1.80412423349522));
#62203=CARTESIAN_POINT('Ctrl Pts',(-0.44212390857688,-0.691982244717549,
-1.8129829770685));
#62204=CARTESIAN_POINT('Ctrl Pts',(-0.622631625634533,-0.535390358803121,
-1.82184172064177));
#62205=CARTESIAN_POINT('Ctrl Pts',(-0.71616399472238,-0.336077881841817,
-1.83070046421504));
#62206=CARTESIAN_POINT('Ctrl Pts',(-0.765317280859627,-0.231334857514047,
-1.8353559258688));
#62207=CARTESIAN_POINT('Ctrl Pts',(-0.791100000000064,-0.115702837836059,
-1.84001138752256));
#62208=CARTESIAN_POINT('Ctrl Pts',(-0.7911,4.34319247233361E-13,-1.84466684917631));
#62209=CARTESIAN_POINT('Ctrl Pts',(-0.7911,-8.75965966429249E-14,-1.87313315082369));
#62210=CARTESIAN_POINT('Ctrl Pts',(-0.791099999999976,-0.220167589666752,
-1.86427440725042));
#62211=CARTESIAN_POINT('Ctrl Pts',(-0.694214576672334,-0.438610418338736,
-1.85541566367715));
#62212=CARTESIAN_POINT('Ctrl Pts',(-0.531017389080291,-0.586395551223192,
-1.84655692010388));
#62213=CARTESIAN_POINT('Ctrl Pts',(-0.367820201488247,-0.734180684107648,
-1.8376981765306));
#62214=CARTESIAN_POINT('Ctrl Pts',(-0.140868175871716,-0.808992666571338,
-1.82883943295733));
#62215=CARTESIAN_POINT('Ctrl Pts',(0.0782205473247804,-0.787223447298295,
-1.81998068938406));
#62216=CARTESIAN_POINT('Ctrl Pts',(0.297309270521277,-0.765454228025253,
-1.81112194581079));
#62217=CARTESIAN_POINT('Ctrl Pts',(0.505102072675593,-0.647444880834229,
-1.80226320223752));
#62218=CARTESIAN_POINT('Ctrl Pts',(0.636026795761725,-0.470435038100983,
-1.79340445866424));
#62219=CARTESIAN_POINT('Ctrl Pts',(0.766951518847857,-0.293425195367737,
-1.78454571509097));
#62220=CARTESIAN_POINT('Ctrl Pts',(0.818956872247065,-0.0601881960099645,
-1.7756869715177));
#62221=CARTESIAN_POINT('Ctrl Pts',(0.775631781004219,0.15567450111121,-1.76682822794443));
#62222=CARTESIAN_POINT('Ctrl Pts',(0.732306689761372,0.371537198232384,
-1.75796948437115));
#62223=CARTESIAN_POINT('Ctrl Pts',(0.594329958850259,0.566643518936446,
-1.74911074079788));
#62224=CARTESIAN_POINT('Ctrl Pts',(0.405242230244105,0.679424716084706,
-1.74025199722461));
#62225=CARTESIAN_POINT('Ctrl Pts',(0.216154501637952,0.792205913232966,
-1.73139325365134));
#62226=CARTESIAN_POINT('Ctrl Pts',(-0.0210816529299128,0.820894963713003,
-1.72253451007807));
#62227=CARTESIAN_POINT('Ctrl Pts',(-0.231602780753112,0.756438604215455,
-1.71367576650479));
#62228=CARTESIAN_POINT('Ctrl Pts',(-0.442123908576311,0.691982244717908,
-1.70481702293152));
#62229=CARTESIAN_POINT('Ctrl Pts',(-0.62263162563408,0.535390358803641,
-1.69595827935825));
#62230=CARTESIAN_POINT('Ctrl Pts',(-0.716163994722092,0.336077881842432,
-1.68709953578498));
#62231=CARTESIAN_POINT('Ctrl Pts',(-0.765317280859473,0.231334857514609,
-1.68244407413122));
#62232=CARTESIAN_POINT('Ctrl Pts',(-0.79110000000001,0.115702837836528,
-1.67778861247745));
#62233=CARTESIAN_POINT('Ctrl Pts',(-0.7911,-7.05546732149287E-14,-1.67313315082369));
#62234=CARTESIAN_POINT('Origin',(0.,0.,-5.925));
#62235=CARTESIAN_POINT('',(-0.790643101388239,0.000413675204086472,-1.44466684917632));
#62236=CARTESIAN_POINT('',(-0.790455823492844,-7.84331714051887E-5,-1.4731331508237));
#62237=CARTESIAN_POINT('',(-0.7911,-9.68818082805471E-17,-5.925));
#62238=CARTESIAN_POINT('Ctrl Pts',(-0.790643101388239,0.000413675204086472,
-1.44466684917632));
#62239=CARTESIAN_POINT('Ctrl Pts',(-0.790904615161135,0.111330088002923,
-1.44911812195309));
#62240=CARTESIAN_POINT('Ctrl Pts',(-0.76848813566008,0.22195367907901,-1.45356939472987));
#62241=CARTESIAN_POINT('Ctrl Pts',(-0.723356415587075,0.322451128215468,
-1.45802066750665));
#62242=CARTESIAN_POINT('Ctrl Pts',(-0.615972969380901,0.561568148478508,
-1.46861173316958));
#62243=CARTESIAN_POINT('Ctrl Pts',(-0.379993291021312,0.743358736491673,
-1.47920279883251));
#62244=CARTESIAN_POINT('Ctrl Pts',(-0.121169674969144,0.783335602370142,
-1.48979386449544));
#62245=CARTESIAN_POINT('Ctrl Pts',(0.137653941083039,0.823312468248613,
-1.50038493015837));
#62246=CARTESIAN_POINT('Ctrl Pts',(0.419321494827788,0.721475611992372,
-1.51097599582129));
#62247=CARTESIAN_POINT('Ctrl Pts',(0.593077223590446,0.525653338426826,
-1.52156706148422));
#62248=CARTESIAN_POINT('Ctrl Pts',(0.766832952353103,0.329831064861279,
-1.53215812714715));
#62249=CARTESIAN_POINT('Ctrl Pts',(0.832676856133661,0.0400233739863956,
-1.54274919281008));
#62250=CARTESIAN_POINT('Ctrl Pts',(0.76274880853202,-0.213141475635434,
-1.55334025847301));
#62251=CARTESIAN_POINT('Ctrl Pts',(0.727784784731201,-0.339723900446341,
-1.55863579130448));
#62252=CARTESIAN_POINT('Ctrl Pts',(0.658877773084845,-0.457145614943989,
-1.56393132413594));
#62253=CARTESIAN_POINT('Ctrl Pts',(0.566731889921311,-0.551503724098459,
-1.5692268569674));
#62254=CARTESIAN_POINT('Ctrl Pts',(0.474586006757777,-0.64586183325293,
-1.57452238979887));
#62255=CARTESIAN_POINT('Ctrl Pts',(0.359201252077072,-0.717156337064215,
-1.57981792263033));
#62256=CARTESIAN_POINT('Ctrl Pts',(0.233902728280942,-0.755973389262662,
-1.5851134554618));
#62257=CARTESIAN_POINT('Ctrl Pts',(0.108604204484811,-0.794790441461109,
-1.59040898829326));
#62258=CARTESIAN_POINT('Ctrl Pts',(-0.0266080884267369,-0.801130042046715,
-1.59570452112473));
#62259=CARTESIAN_POINT('Ctrl Pts',(-0.155985688497453,-0.775256871710341,
-1.60100005395619));
#62260=CARTESIAN_POINT('Ctrl Pts',(-0.285363288568183,-0.749383701373963,
-1.60629558678765));
#62261=CARTESIAN_POINT('Ctrl Pts',(-0.408906195798072,-0.691297760115601,
-1.61159111961912));
#62262=CARTESIAN_POINT('Ctrl Pts',(-0.509294381945595,-0.606609894578137,
-1.61688665245058));
#62263=CARTESIAN_POINT('Ctrl Pts',(-0.684838791977828,-0.458519945320396,
-1.62614671802583));
#62264=CARTESIAN_POINT('Ctrl Pts',(-0.789580741841121,-0.229086684800661,
-1.63540678360107));
#62265=CARTESIAN_POINT('Ctrl Pts',(-0.79151332369587,0.000198305622813172,
-1.64466684917632));
#62266=CARTESIAN_POINT('Ctrl Pts',(-0.7911,-7.05546732149287E-14,-1.67313315082369));
#62267=CARTESIAN_POINT('Ctrl Pts',(-0.79109999999998,-0.22016758966675,
-1.66427440725042));
#62268=CARTESIAN_POINT('Ctrl Pts',(-0.694214576672329,-0.438610418338751,
-1.65541566367715));
#62269=CARTESIAN_POINT('Ctrl Pts',(-0.53101738908027,-0.586395551223211,
-1.64655692010387));
#62270=CARTESIAN_POINT('Ctrl Pts',(-0.36782020148821,-0.734180684107671,
-1.6376981765306));
#62271=CARTESIAN_POINT('Ctrl Pts',(-0.140868175871656,-0.808992666571353,
-1.62883943295733));
#62272=CARTESIAN_POINT('Ctrl Pts',(0.078220547324853,-0.787223447298288,
-1.61998068938406));
#62273=CARTESIAN_POINT('Ctrl Pts',(0.297309270521362,-0.765454228025224,
-1.61112194581078));
#62274=CARTESIAN_POINT('Ctrl Pts',(0.50510207267568,-0.647444880834166,
-1.60226320223751));
#62275=CARTESIAN_POINT('Ctrl Pts',(0.636026795761795,-0.470435038100888,
-1.59340445866424));
#62276=CARTESIAN_POINT('Ctrl Pts',(0.766951518847909,-0.293425195367611,
-1.58454571509097));
#62277=CARTESIAN_POINT('Ctrl Pts',(0.81895687224708,-0.0601881960098106,
-1.57568697151769));
#62278=CARTESIAN_POINT('Ctrl Pts',(0.775631781004187,0.15567450111137,-1.56682822794442));
#62279=CARTESIAN_POINT('Ctrl Pts',(0.732306689761293,0.37153719823255,-1.55796948437115));
#62280=CARTESIAN_POINT('Ctrl Pts',(0.594329958850123,0.566643518936595,
-1.54911074079787));
#62281=CARTESIAN_POINT('Ctrl Pts',(0.405242230243927,0.679424716084813,
-1.5402519972246));
#62282=CARTESIAN_POINT('Ctrl Pts',(0.216154501637731,0.79220591323303,-1.53139325365133));
#62283=CARTESIAN_POINT('Ctrl Pts',(-0.0210816529301607,0.820894963713,-1.52253451007806));
#62284=CARTESIAN_POINT('Ctrl Pts',(-0.231602780753354,0.756438604215381,
-1.51367576650478));
#62285=CARTESIAN_POINT('Ctrl Pts',(-0.442123908576547,0.691982244717762,
-1.50481702293151));
#62286=CARTESIAN_POINT('Ctrl Pts',(-0.622631625634275,0.535390358803421,
-1.49595827935824));
#62287=CARTESIAN_POINT('Ctrl Pts',(-0.716163994722218,0.336077881842162,
-1.48709953578497));
#62288=CARTESIAN_POINT('Ctrl Pts',(-0.765317280859516,0.231334857514416,
-1.48244407413121));
#62289=CARTESIAN_POINT('Ctrl Pts',(-0.791100000000008,0.11570283783644,
-1.47778861247745));
#62290=CARTESIAN_POINT('Ctrl Pts',(-0.7911,-5.35127497869325E-14,-1.47313315082369));
#62291=CARTESIAN_POINT('Origin',(0.,0.,-5.925));
#62292=CARTESIAN_POINT('',(-0.790116780300585,-0.000593511115090206,-1.24466684917632));
#62293=CARTESIAN_POINT('',(-0.791419810366198,-0.000275355779050857,-1.27313315082369));
#62294=CARTESIAN_POINT('',(-0.7911,-9.68818082805471E-17,-5.925));
#62295=CARTESIAN_POINT('Ctrl Pts',(-0.790116780300585,-0.000593511115090206,
-1.24466684917632));
#62296=CARTESIAN_POINT('Ctrl Pts',(-0.788689659215958,0.187798474330122,
-1.25223839464219));
#62297=CARTESIAN_POINT('Ctrl Pts',(-0.721977966372551,0.377047291568571,
-1.25980994010805));
#62298=CARTESIAN_POINT('Ctrl Pts',(-0.599448613644661,0.518611719566975,
-1.26738148557392));
#62299=CARTESIAN_POINT('Ctrl Pts',(-0.428054751423635,0.716631814569354,
-1.27797255123685));
#62300=CARTESIAN_POINT('Ctrl Pts',(-0.147445993055172,0.821350871343271,
-1.28856361689978));
#62301=CARTESIAN_POINT('Ctrl Pts',(0.111755050952167,0.784578124808293,
-1.29915468256271));
#62302=CARTESIAN_POINT('Ctrl Pts',(0.370956094959505,0.747805378273315,
-1.30974574822564));
#62303=CARTESIAN_POINT('Ctrl Pts',(0.608749424605719,0.569540828429441,
-1.32033681388857));
#62304=CARTESIAN_POINT('Ctrl Pts',(0.719337787722662,0.331312813979979,
-1.3309278795515));
#62305=CARTESIAN_POINT('Ctrl Pts',(0.774631969281131,0.212198806755254,
-1.33622341238296));
#62306=CARTESIAN_POINT('Ctrl Pts',(0.798124909207285,0.0780939333791335,
-1.34151894521443));
#62307=CARTESIAN_POINT('Ctrl Pts',(0.788975113880318,-0.0534758115954189,
-1.34681447804589));
#62308=CARTESIAN_POINT('Ctrl Pts',(0.77982531855335,-0.185045556570001,
-1.35211001087735));
#62309=CARTESIAN_POINT('Ctrl Pts',(0.738032787973245,-0.314080173143015,
-1.35740554370882));
#62310=CARTESIAN_POINT('Ctrl Pts',(0.66765971662573,-0.424778476815616,
-1.36270107654029));
#62311=CARTESIAN_POINT('Ctrl Pts',(0.597286645278231,-0.535476780488192,
-1.36799660937175));
#62312=CARTESIAN_POINT('Ctrl Pts',(0.498333033163336,-0.627838771260365,
-1.37329214220321));
#62313=CARTESIAN_POINT('Ctrl Pts',(0.382973555042227,-0.691871381319134,
-1.37858767503468));
#62314=CARTESIAN_POINT('Ctrl Pts',(0.267614076921119,-0.755903991377902,
-1.38388320786614));
#62315=CARTESIAN_POINT('Ctrl Pts',(0.135848732793798,-0.791607220723266,
-1.38917874069761));
#62316=CARTESIAN_POINT('Ctrl Pts',(0.00451088429379835,-0.792045442890957,
-1.39447427352907));
#62317=CARTESIAN_POINT('Ctrl Pts',(-0.258164812706215,-0.792921887226339,
-1.405065339192));
#62318=CARTESIAN_POINT('Ctrl Pts',(-0.519130527196939,-0.652738302851012,
-1.41565640485493));
#62319=CARTESIAN_POINT('Ctrl Pts',(-0.66295912681962,-0.433424143939486,
-1.42624747051786));
#62320=CARTESIAN_POINT('Ctrl Pts',(-0.734873426630964,-0.323767064483717,
-1.43154300334932));
#62321=CARTESIAN_POINT('Ctrl Pts',(-0.777503447725295,-0.194327341393895,
-1.43683853618079));
#62322=CARTESIAN_POINT('Ctrl Pts',(-0.788047125740096,-0.0626624207519821,
-1.44213406901225));
#62323=CARTESIAN_POINT('Ctrl Pts',(-0.789728090897084,-0.0416712501485153,
-1.44297832906694));
#62324=CARTESIAN_POINT('Ctrl Pts',(-0.790593500826045,-0.0206235205444637,
-1.44382258912163));
#62325=CARTESIAN_POINT('Ctrl Pts',(-0.790643101388239,0.000413675204086472,
-1.44466684917632));
#62326=CARTESIAN_POINT('Ctrl Pts',(-0.78954155091179,-0.000189752502548938,
-1.47313315082369));
#62327=CARTESIAN_POINT('Ctrl Pts',(-0.789371393251466,-0.146463581773617,
-1.46726149744544));
#62328=CARTESIAN_POINT('Ctrl Pts',(-0.750711606351124,-0.292708100538373,
-1.46138984406718));
#62329=CARTESIAN_POINT('Ctrl Pts',(-0.67442271127103,-0.416180287691346,
-1.45551819068893));
#62330=CARTESIAN_POINT('Ctrl Pts',(-0.536815695819837,-0.638894735810089,
-1.444927125026));
#62331=CARTESIAN_POINT('Ctrl Pts',(-0.276780209019268,-0.78751809107129,
-1.43433605936307));
#62332=CARTESIAN_POINT('Ctrl Pts',(-0.0149350547827386,-0.792511009520599,
-1.42374499370014));
#62333=CARTESIAN_POINT('Ctrl Pts',(0.246910099453776,-0.797503927969907,
-1.41315392803721));
#62334=CARTESIAN_POINT('Ctrl Pts',(0.510564921126274,-0.658866409607309,
-1.40256286237428));
#62335=CARTESIAN_POINT('Ctrl Pts',(0.657357033665679,-0.441702348135788,
-1.39197179671135));
#62336=CARTESIAN_POINT('Ctrl Pts',(0.73075308993539,-0.333120317400014,
-1.38667626387989));
#62337=CARTESIAN_POINT('Ctrl Pts',(0.774933468921821,-0.204906650887048,
-1.38138073104843));
#62338=CARTESIAN_POINT('Ctrl Pts',(0.787121134869292,-0.0733837202913743,
-1.37608519821696));
#62339=CARTESIAN_POINT('Ctrl Pts',(0.799308800816764,0.0581392103042997,
-1.3707896653855));
#62340=CARTESIAN_POINT('Ctrl Pts',(0.779503753725249,0.192971404982673,
-1.36549413255403));
#62341=CARTESIAN_POINT('Ctrl Pts',(0.727456171333946,0.313334982361156,
-1.36019859972257));
#62342=CARTESIAN_POINT('Ctrl Pts',(0.623361006551351,0.554062137118093,
-1.34960753405964));
#62343=CARTESIAN_POINT('Ctrl Pts',(0.390295700569642,0.736914822675632,
-1.33901646839671));
#62344=CARTESIAN_POINT('Ctrl Pts',(0.131359649808987,0.781089606948847,
-1.32842540273378));
#62345=CARTESIAN_POINT('Ctrl Pts',(0.00189162442864507,0.803176999085456,
-1.32312986990231));
#62346=CARTESIAN_POINT('Ctrl Pts',(-0.134044087146429,0.790594915900975,
-1.31783433707085));
#62347=CARTESIAN_POINT('Ctrl Pts',(-0.258674226552509,0.747290035172147,
-1.31253880423938));
#62348=CARTESIAN_POINT('Ctrl Pts',(-0.383304365958575,0.703985154443324,
-1.30724327140792));
#62349=CARTESIAN_POINT('Ctrl Pts',(-0.496628933195643,0.629957476170163,
-1.30194773857646));
#62350=CARTESIAN_POINT('Ctrl Pts',(-0.584940139616044,0.53296461855972,
-1.29665220574499));
#62351=CARTESIAN_POINT('Ctrl Pts',(-0.673251346036456,0.435971760949266,
-1.29135667291353));
#62352=CARTESIAN_POINT('Ctrl Pts',(-0.736549191640189,0.316013724001529,
-1.28606114008206));
#62353=CARTESIAN_POINT('Ctrl Pts',(-0.768122374764371,0.187961193161232,
-1.2807656072506));
#62354=CARTESIAN_POINT('Ctrl Pts',(-0.783291194228088,0.126440448973076,
-1.2782214551083));
#62355=CARTESIAN_POINT('Ctrl Pts',(-0.791137438528416,0.0630513621358539,
-1.27567730296599));
#62356=CARTESIAN_POINT('Ctrl Pts',(-0.791419810366198,-0.000275355779050857,
-1.27313315082369));
#62357=CARTESIAN_POINT('Origin',(0.,0.,-5.925));
#62358=CARTESIAN_POINT('',(-0.792649648621414,-0.000247240842943735,-1.04466684917632));
#62359=CARTESIAN_POINT('',(-0.791304392674353,0.000147799391554101,-1.07313315082369));
#62360=CARTESIAN_POINT('',(-0.7911,-9.68818082805471E-17,-5.925));
#62361=CARTESIAN_POINT('Ctrl Pts',(-0.792649648621414,-0.000247240842943735,
-1.04466684917632));
#62362=CARTESIAN_POINT('Ctrl Pts',(-0.792652320571416,0.00224400151945376,
-1.04476760166835));
#62363=CARTESIAN_POINT('Ctrl Pts',(-0.792642050515285,0.00473530815100578,
-1.04486835416038));
#62364=CARTESIAN_POINT('Ctrl Pts',(-0.792618781414662,0.00722657743760985,
-1.04496910665241));
#62365=CARTESIAN_POINT('Ctrl Pts',(-0.790172741940626,0.269107907285088,
-1.05556017231534));
#62366=CARTESIAN_POINT('Ctrl Pts',(-0.644085458455419,0.530576570280527,
-1.06615123797827));
#62367=CARTESIAN_POINT('Ctrl Pts',(-0.422719876558179,0.670343144444435,
-1.0767423036412));
#62368=CARTESIAN_POINT('Ctrl Pts',(-0.20135429466094,0.810109718608342,
-1.08733336930413));
#62369=CARTESIAN_POINT('Ctrl Pts',(0.0952895856483443,0.828174203940726,
-1.09792443496705));
#62370=CARTESIAN_POINT('Ctrl Pts',(0.333796502775129,0.718188643942634,
-1.10851550062998));
#62371=CARTESIAN_POINT('Ctrl Pts',(0.453049961338528,0.663195863943586,
-1.11381103346145));
#62372=CARTESIAN_POINT('Ctrl Pts',(0.557769179106307,0.576190572611911,
-1.11910656629292));
#62373=CARTESIAN_POINT('Ctrl Pts',(0.635967282330499,0.469986179108929,
-1.12440209912438));
#62374=CARTESIAN_POINT('Ctrl Pts',(0.714165385554682,0.363781785605958,
-1.12969763195584));
#62375=CARTESIAN_POINT('Ctrl Pts',(0.765842374235291,0.238378289931675,
-1.13499316478731));
#62376=CARTESIAN_POINT('Ctrl Pts',(0.783865480633038,0.10844888124126,-1.14028869761877));
#62377=CARTESIAN_POINT('Ctrl Pts',(0.801888587030786,-0.0214805274491695,
-1.14558423045024));
#62378=CARTESIAN_POINT('Ctrl Pts',(0.786257811145676,-0.155935849155701,
-1.1508797632817));
#62379=CARTESIAN_POINT('Ctrl Pts',(0.739783541611409,-0.27941915415914,
-1.15617529611317));
#62380=CARTESIAN_POINT('Ctrl Pts',(0.693309272077147,-0.402902459162565,
-1.16147082894463));
#62381=CARTESIAN_POINT('Ctrl Pts',(0.615991508893732,-0.515413747462867,
-1.16676636177609));
#62382=CARTESIAN_POINT('Ctrl Pts',(0.516170691110303,-0.600769630823793,
-1.17206189460756));
#62383=CARTESIAN_POINT('Ctrl Pts',(0.316529055543421,-0.771481397545664,
-1.18265296027049));
#62384=CARTESIAN_POINT('Ctrl Pts',(0.0268752015764362,-0.833571544510021,
-1.19324402593342));
#62385=CARTESIAN_POINT('Ctrl Pts',(-0.224723188338764,-0.759520099145486,
-1.20383509159635));
#62386=CARTESIAN_POINT('Ctrl Pts',(-0.35052238329635,-0.722494376463222,
-1.20913062442781));
#62387=CARTESIAN_POINT('Ctrl Pts',(-0.466807712240998,-0.651433255698741,
-1.21442615725928));
#62388=CARTESIAN_POINT('Ctrl Pts',(-0.560077612187121,-0.557904937859935,
-1.21972169009074));
#62389=CARTESIAN_POINT('Ctrl Pts',(-0.653347512133266,-0.464376620021107,
-1.22501722292221));
#62390=CARTESIAN_POINT('Ctrl Pts',(-0.723601983080881,-0.348381105107937,
-1.23031275575367));
#62391=CARTESIAN_POINT('Ctrl Pts',(-0.760075136033682,-0.222497239627344,
-1.23560828858514));
#62392=CARTESIAN_POINT('Ctrl Pts',(-0.780872178653654,-0.150718084176908,
-1.2386278087822));
#62393=CARTESIAN_POINT('Ctrl Pts',(-0.790685913901923,-0.0757239329794748,
-1.24164732897926));
#62394=CARTESIAN_POINT('Ctrl Pts',(-0.790116780300585,-0.000593511115090206,
-1.24466684917632));
#62395=CARTESIAN_POINT('Ctrl Pts',(-0.791419810366198,-0.000275355779050857,
-1.27313315082369));
#62396=CARTESIAN_POINT('Ctrl Pts',(-0.791725182206475,-0.0687602179388454,
-1.27038177013453));
#62397=CARTESIAN_POINT('Ctrl Pts',(-0.783184299960073,-0.137172137127078,
-1.26763038944537));
#62398=CARTESIAN_POINT('Ctrl Pts',(-0.76549197012783,-0.2030691439458,-1.26487900875621));
#62399=CARTESIAN_POINT('Ctrl Pts',(-0.697387753317123,-0.456730707013651,
-1.25428794309328));
#62400=CARTESIAN_POINT('Ctrl Pts',(-0.493681020306463,-0.673127297285795,
-1.24369687743035));
#62401=CARTESIAN_POINT('Ctrl Pts',(-0.244623479252935,-0.753797969444869,
-1.23310581176742));
#62402=CARTESIAN_POINT('Ctrl Pts',(0.00443406180057812,-0.834468641603939,
-1.22251474610449));
#62403=CARTESIAN_POINT('Ctrl Pts',(0.298842410896965,-0.779413395649963,
-1.21192368044156));
#62404=CARTESIAN_POINT('Ctrl Pts',(0.501650560616659,-0.613712857210694,
-1.20133261477863));
#62405=CARTESIAN_POINT('Ctrl Pts',(0.704458710336341,-0.448012318771434,
-1.1907415491157));
#62406=CARTESIAN_POINT('Ctrl Pts',(0.815666660679348,-0.171666487846932,
-1.18015048345277));
#62407=CARTESIAN_POINT('Ctrl Pts',(0.786968579401671,0.0888801951670066,
-1.16955941778984));
#62408=CARTESIAN_POINT('Ctrl Pts',(0.772619538762829,0.219153536674006,
-1.16426388495838));
#62409=CARTESIAN_POINT('Ctrl Pts',(0.723293990218791,0.345477091203361,
-1.15896835212691));
#62410=CARTESIAN_POINT('Ctrl Pts',(0.647441629484383,0.453612376123417,
-1.15367281929545));
#62411=CARTESIAN_POINT('Ctrl Pts',(0.571589268749992,0.561747661043449,
-1.14837728646398));
#62412=CARTESIAN_POINT('Ctrl Pts',(0.469210095825238,0.651694676354199,
-1.14308175363252));
#62413=CARTESIAN_POINT('Ctrl Pts',(0.351622253064786,0.709741561085972,
-1.13778622080105));
#62414=CARTESIAN_POINT('Ctrl Pts',(0.116446567543868,0.825835330549523,
-1.12719515513813));
#62415=CARTESIAN_POINT('Ctrl Pts',(-0.179563797319874,0.814328577697159,
-1.11660408947519));
#62416=CARTESIAN_POINT('Ctrl Pts',(-0.40551913086259,0.680375312739883,
-1.10601302381227));
#62417=CARTESIAN_POINT('Ctrl Pts',(-0.518496797633955,0.613398680261241,
-1.1007174909808));
#62418=CARTESIAN_POINT('Ctrl Pts',(-0.613960706575066,0.515810419756364,
-1.09542195814934));
#62419=CARTESIAN_POINT('Ctrl Pts',(-0.680919134805824,0.402124214646937,
-1.09012642531787));
#62420=CARTESIAN_POINT('Ctrl Pts',(-0.747877563036576,0.288438009537523,
-1.08483089248641));
#62421=CARTESIAN_POINT('Ctrl Pts',(-0.786330510556985,0.158653859823556,
-1.07953535965494));
#62422=CARTESIAN_POINT('Ctrl Pts',(-0.790851939689893,0.0275583210533076,
-1.07423982682348));
#62423=CARTESIAN_POINT('Ctrl Pts',(-0.791166906868543,0.0184260775156362,
-1.07387093482355));
#62424=CARTESIAN_POINT('Ctrl Pts',(-0.791317216198072,0.00928747026329368,
-1.07350204282362));
#62425=CARTESIAN_POINT('Ctrl Pts',(-0.791304392674353,0.000147799391554101,
-1.07313315082369));
#62426=CARTESIAN_POINT('Origin',(0.,0.,-5.925));
#62427=CARTESIAN_POINT('',(-0.790929060525409,0.000272143640698088,-0.844666849176317));
#62428=CARTESIAN_POINT('',(-0.7911,-2.33146835171283E-15,-0.873133150823696));
#62429=CARTESIAN_POINT('',(-0.7911,-9.68818082805471E-17,-5.925));
#62430=CARTESIAN_POINT('Ctrl Pts',(-0.790491490569074,0.000968775477774575,
-0.844666849176317));
#62431=CARTESIAN_POINT('Ctrl Pts',(-0.791140089290106,0.0812481867562639,
-0.84788787435744));
#62432=CARTESIAN_POINT('Ctrl Pts',(-0.779937728478808,0.161300589550352,
-0.851108899538562));
#62433=CARTESIAN_POINT('Ctrl Pts',(-0.756141466551346,0.237280652184228,
-0.854329924719685));
#62434=CARTESIAN_POINT('Ctrl Pts',(-0.677896883403394,0.487110997238635,
-0.864920990382615));
#62435=CARTESIAN_POINT('Ctrl Pts',(-0.463491730456965,0.692912716729475,
-0.875512056045544));
#62436=CARTESIAN_POINT('Ctrl Pts',(-0.210504529835239,0.763480763656139,
-0.886103121708472));
#62437=CARTESIAN_POINT('Ctrl Pts',(-0.0840109295243834,0.79876478711947,
-0.891398654539936));
#62438=CARTESIAN_POINT('Ctrl Pts',(0.0521281827052891,0.800240392441759,
-0.8966941873714));
#62439=CARTESIAN_POINT('Ctrl Pts',(0.18048173029882,0.769914110648867,-0.901989720202864));
#62440=CARTESIAN_POINT('Ctrl Pts',(0.308835277892352,0.739587828855975,
-0.907285253034329));
#62441=CARTESIAN_POINT('Ctrl Pts',(0.429403260849733,0.677459659947905,
-0.912580785865794));
#62442=CARTESIAN_POINT('Ctrl Pts',(0.527250424553959,0.590095959466128,
-0.917876318697259));
#62443=CARTESIAN_POINT('Ctrl Pts',(0.625097588258208,0.502732258984331,
-0.923171851528724));
#62444=CARTESIAN_POINT('Ctrl Pts',(0.700223932709283,0.390133026928822,
-0.928467384360189));
#62445=CARTESIAN_POINT('Ctrl Pts',(0.744738887959545,0.265929954895926,
-0.933762917191654));
#62446=CARTESIAN_POINT('Ctrl Pts',(0.789253843209797,0.141726882863057,
-0.939058450023118));
#62447=CARTESIAN_POINT('Ctrl Pts',(0.803157409259246,0.00591997085281483,
-0.944353982854583));
#62448=CARTESIAN_POINT('Ctrl Pts',(0.782330236569644,-0.123756747817209,
-0.949649515686047));
#62449=CARTESIAN_POINT('Ctrl Pts',(0.740675891190436,-0.383110185157272,
-0.960240581348976));
#62450=CARTESIAN_POINT('Ctrl Pts',(0.560098590854975,-0.617942849136481,
-0.970831647011908));
#62451=CARTESIAN_POINT('Ctrl Pts',(0.320395226075553,-0.724374344859862,
-0.981422712674837));
#62452=CARTESIAN_POINT('Ctrl Pts',(0.200543543685848,-0.777590092721549,
-0.986718245506301));
#62453=CARTESIAN_POINT('Ctrl Pts',(0.0659103451851567,-0.798705548519292,
-0.992013778337765));
#62454=CARTESIAN_POINT('Ctrl Pts',(-0.0657248991611227,-0.787797619310929,
-0.997309311169229));
#62455=CARTESIAN_POINT('Ctrl Pts',(-0.197360143507402,-0.776889690102566,
-1.00260484400069));
#62456=CARTESIAN_POINT('Ctrl Pts',(-0.325997433699261,-0.733958375888098,
-1.00790037683216));
#62457=CARTESIAN_POINT('Ctrl Pts',(-0.435288161250025,-0.661621833628534,
-1.01319590966362));
#62458=CARTESIAN_POINT('Ctrl Pts',(-0.651790257483054,-0.518325019851074,
-1.02368622283452));
#62459=CARTESIAN_POINT('Ctrl Pts',(-0.792371446149874,-0.259634498065135,
-1.03417653600542));
#62460=CARTESIAN_POINT('Ctrl Pts',(-0.792649648621414,-0.000247240842943735,
-1.04466684917632));
#62461=CARTESIAN_POINT('Ctrl Pts',(-0.791304392674353,0.000147799391554101,
-1.07313315082369));
#62462=CARTESIAN_POINT('Ctrl Pts',(-0.791133131450012,-0.121914689662786,
-1.06820650999216));
#62463=CARTESIAN_POINT('Ctrl Pts',(-0.761865101488357,-0.244166888435379,
-1.06327986916062));
#62464=CARTESIAN_POINT('Ctrl Pts',(-0.707132953686239,-0.353983585155056,
-1.05835322832909));
#62465=CARTESIAN_POINT('Ctrl Pts',(-0.648302627804268,-0.472023024766635,
-1.05305769549762));
#62466=CARTESIAN_POINT('Ctrl Pts',(-0.560052065294921,-0.575694976163254,
-1.04776216266616));
#62467=CARTESIAN_POINT('Ctrl Pts',(-0.451993647262742,-0.650320518196367,
-1.04246662983469));
#62468=CARTESIAN_POINT('Ctrl Pts',(-0.235876811198358,-0.799571602262608,
-1.03187556417176));
#62469=CARTESIAN_POINT('Ctrl Pts',(0.0594714469573586,-0.832637048874779,
-1.02128449850883));
#62470=CARTESIAN_POINT('Ctrl Pts',(0.301523172572088,-0.732895491692423,
-1.0106934328459));
#62471=CARTESIAN_POINT('Ctrl Pts',(0.54357489818679,-0.633153934510077,
-1.00010236718298));
#62472=CARTESIAN_POINT('Ctrl Pts',(0.732330091260526,-0.400605373533196,
-0.989511301520047));
#62473=CARTESIAN_POINT('Ctrl Pts',(0.779641955417371,-0.143021597759585,
-0.978920235857118));
#62474=CARTESIAN_POINT('Ctrl Pts',(0.826953819574218,0.114562178014041,
-0.968329170194189));
#62475=CARTESIAN_POINT('Ctrl Pts',(0.732822354814194,0.397181168584429,
-0.957738104531258));
#62476=CARTESIAN_POINT('Ctrl Pts',(0.542283414281508,0.577189685158702,
-0.947147038868329));
#62477=CARTESIAN_POINT('Ctrl Pts',(0.447013944015171,0.667193943445833,
-0.941851506036865));
#62478=CARTESIAN_POINT('Ctrl Pts',(0.327642604805676,0.731545583233934,
-0.936555973205402));
#62479=CARTESIAN_POINT('Ctrl Pts',(0.199826993358222,0.764862094816524,
-0.931260440373937));
#62480=CARTESIAN_POINT('Ctrl Pts',(0.072011381910739,0.798178606399122,
-0.925964907542472));
#62481=CARTESIAN_POINT('Ctrl Pts',(-0.0642485017746986,0.800459989776192,
-0.920669374711006));
#62482=CARTESIAN_POINT('Ctrl Pts',(-0.191449667115583,0.768582017317925,
-0.915373841879541));
#62483=CARTESIAN_POINT('Ctrl Pts',(-0.445851997797293,0.704826072401405,
-0.904782776216612));
#62484=CARTESIAN_POINT('Ctrl Pts',(-0.664019455100784,0.504432704143612,
-0.894191710553685));
#62485=CARTESIAN_POINT('Ctrl Pts',(-0.749525564601939,0.25606202313024,
-0.883600644890755));
#62486=CARTESIAN_POINT('Ctrl Pts',(-0.777695052683879,0.174237753735608,
-0.880111480201735));
#62487=CARTESIAN_POINT('Ctrl Pts',(-0.791466346747543,0.0872063409719881,
-0.876622315512715));
#62488=CARTESIAN_POINT('Ctrl Pts',(-0.791130549170082,0.000167441804084007,
-0.873133150823694));
#62489=CARTESIAN_POINT('Origin',(0.,0.,-5.925));
#62490=CARTESIAN_POINT('',(-0.790728689320429,-0.000203321923638479,-0.64466684917632));
#62491=CARTESIAN_POINT('',(-0.790791327823967,-2.33035369215209E-5,-0.673133150823699));
#62492=CARTESIAN_POINT('',(-0.7911,-9.68818082805471E-17,-5.925));
#62493=CARTESIAN_POINT('Ctrl Pts',(-0.7911,5.8164584260112E-13,-0.644666849176319));
#62494=CARTESIAN_POINT('Ctrl Pts',(-0.791099999999838,0.220167589667276,
-0.653525592749593));
#62495=CARTESIAN_POINT('Ctrl Pts',(-0.694214576672032,0.438610418339229,
-0.662384336322865));
#62496=CARTESIAN_POINT('Ctrl Pts',(-0.531017389079858,0.586395551223584,
-0.671243079896138));
#62497=CARTESIAN_POINT('Ctrl Pts',(-0.367820201487683,0.73418068410794,
-0.680101823469412));
#62498=CARTESIAN_POINT('Ctrl Pts',(-0.140868175871057,0.808992666571461,
-0.688960567042685));
#62499=CARTESIAN_POINT('Ctrl Pts',(0.0782205473254509,0.787223447298229,
-0.697819310615959));
#62500=CARTESIAN_POINT('Ctrl Pts',(0.297309270521959,0.765454228024996,
-0.706678054189232));
#62501=CARTESIAN_POINT('Ctrl Pts',(0.5051020726762,0.647444880833766,-0.715536797762506));
#62502=CARTESIAN_POINT('Ctrl Pts',(0.636026795762179,0.470435038100369,
-0.724395541335779));
#62503=CARTESIAN_POINT('Ctrl Pts',(0.766951518848158,0.293425195366972,
-0.733254284909053));
#62504=CARTESIAN_POINT('Ctrl Pts',(0.818956872247135,0.06018819600911,-0.742113028482325));
#62505=CARTESIAN_POINT('Ctrl Pts',(0.77563178100405,-0.155674501112047,
-0.750971772055598));
#62506=CARTESIAN_POINT('Ctrl Pts',(0.732306689760965,-0.371537198233204,
-0.759830515628871));
#62507=CARTESIAN_POINT('Ctrl Pts',(0.594329958849608,-0.56664351893714,
-0.768689259202145));
#62508=CARTESIAN_POINT('Ctrl Pts',(0.405242230243295,-0.679424716085189,
-0.777548002775418));
#62509=CARTESIAN_POINT('Ctrl Pts',(0.216154501636982,-0.792205913233239,
-0.786406746348692));
#62510=CARTESIAN_POINT('Ctrl Pts',(-0.0210816529309567,-0.820894963712984,
-0.795265489921966));
#62511=CARTESIAN_POINT('Ctrl Pts',(-0.2316027807541,-0.756438604215153,
-0.804124233495239));
#62512=CARTESIAN_POINT('Ctrl Pts',(-0.442123908577244,-0.691982244717321,
-0.812982977068512));
#62513=CARTESIAN_POINT('Ctrl Pts',(-0.622631625634828,-0.535390358802784,
-0.821841720641784));
#62514=CARTESIAN_POINT('Ctrl Pts',(-0.716163994722569,-0.336077881841415,
-0.830700464215058));
#62515=CARTESIAN_POINT('Ctrl Pts',(-0.765317280859706,-0.231334857513725,
-0.83535592586881));
#62516=CARTESIAN_POINT('Ctrl Pts',(-0.791100000000076,-0.115702837835854,
-0.840011387522564));
#62517=CARTESIAN_POINT('Ctrl Pts',(-0.7911,5.19639886675805E-13,-0.844666849176317));
#62518=CARTESIAN_POINT('Ctrl Pts',(-0.7911,-2.33146835171283E-15,-0.873133150823696));
#62519=CARTESIAN_POINT('Ctrl Pts',(-0.791099999999999,-0.220167589666667,
-0.864274407250424));
#62520=CARTESIAN_POINT('Ctrl Pts',(-0.694214576672381,-0.438610418338662,
-0.855415663677151));
#62521=CARTESIAN_POINT('Ctrl Pts',(-0.531017389080354,-0.586395551223135,
-0.846556920103879));
#62522=CARTESIAN_POINT('Ctrl Pts',(-0.367820201488326,-0.734180684107609,
-0.837698176530607));
#62523=CARTESIAN_POINT('Ctrl Pts',(-0.140868175871803,-0.808992666571323,
-0.828839432957334));
#62524=CARTESIAN_POINT('Ctrl Pts',(0.0782205473246955,-0.787223447298304,
-0.819980689384062));
#62525=CARTESIAN_POINT('Ctrl Pts',(0.297309270521194,-0.765454228025285,
-0.81112194581079));
#62526=CARTESIAN_POINT('Ctrl Pts',(0.505102072675523,-0.647444880834284,
-0.802263202237519));
#62527=CARTESIAN_POINT('Ctrl Pts',(0.636026795761674,-0.470435038101052,
-0.793404458664247));
#62528=CARTESIAN_POINT('Ctrl Pts',(0.766951518847825,-0.29342519536782,
-0.784545715090975));
#62529=CARTESIAN_POINT('Ctrl Pts',(0.818956872247058,-0.0601881960100528,
-0.775686971517702));
#62530=CARTESIAN_POINT('Ctrl Pts',(0.775631781004235,0.155674501111126,
-0.76682822794443));
#62531=CARTESIAN_POINT('Ctrl Pts',(0.732306689761412,0.371537198232305,
-0.757969484371158));
#62532=CARTESIAN_POINT('Ctrl Pts',(0.59432995885032,0.566643518936382,-0.749110740797887));
#62533=CARTESIAN_POINT('Ctrl Pts',(0.405242230244179,0.679424716084662,
-0.740251997224615));
#62534=CARTESIAN_POINT('Ctrl Pts',(0.216154501638038,0.792205913232943,
-0.731393253651343));
#62535=CARTESIAN_POINT('Ctrl Pts',(-0.0210816529298243,0.820894963713005,
-0.72253451007807));
#62536=CARTESIAN_POINT('Ctrl Pts',(-0.23160278075303,0.75643860421548,-0.713675766504798));
#62537=CARTESIAN_POINT('Ctrl Pts',(-0.442123908576237,0.691982244717956,
-0.704817022931526));
#62538=CARTESIAN_POINT('Ctrl Pts',(-0.622631625634022,0.535390358803709,
-0.695958279358253));
#62539=CARTESIAN_POINT('Ctrl Pts',(-0.716163994722056,0.336077881842509,
-0.687099535784981));
#62540=CARTESIAN_POINT('Ctrl Pts',(-0.765317280859448,0.231334857514691,
-0.682444074131219));
#62541=CARTESIAN_POINT('Ctrl Pts',(-0.791099999999998,0.115702837836613,
-0.677788612477458));
#62542=CARTESIAN_POINT('Ctrl Pts',(-0.7911,1.47104550762833E-14,-0.673133150823697));
#62543=CARTESIAN_POINT('Origin',(0.,0.,-5.925));
#62544=CARTESIAN_POINT('',(-0.791944510864312,-0.00022813924889703,-0.444666849176321));
#62545=CARTESIAN_POINT('',(-0.791972558534597,-0.000546350253884251,-0.473133150823699));
#62546=CARTESIAN_POINT('',(-0.7911,-9.68818082805471E-17,-5.925));
#62547=CARTESIAN_POINT('Ctrl Pts',(-0.791944510864312,-0.00022813924889703,
-0.444666849176321));
#62548=CARTESIAN_POINT('Ctrl Pts',(-0.791679905405434,0.103219919931978,
-0.448832886904162));
#62549=CARTESIAN_POINT('Ctrl Pts',(-0.770434409145543,0.206944064816135,
-0.452998924632003));
#62550=CARTESIAN_POINT('Ctrl Pts',(-0.730546028063464,0.302727261406224,
-0.457164962359844));
#62551=CARTESIAN_POINT('Ctrl Pts',(-0.679843119109353,0.424479174226344,
-0.462460495191308));
#62552=CARTESIAN_POINT('Ctrl Pts',(-0.599018054451231,0.533400536236713,
-0.467756028022773));
#62553=CARTESIAN_POINT('Ctrl Pts',(-0.496968020873342,0.61581579008526,
-0.473051560854237));
#62554=CARTESIAN_POINT('Ctrl Pts',(-0.394917987295454,0.698231043933806,
-0.478347093685701));
#62555=CARTESIAN_POINT('Ctrl Pts',(-0.271642984797799,0.75414018962053,
-0.483642626517165));
#62556=CARTESIAN_POINT('Ctrl Pts',(-0.141872253513096,0.777963364750619,
-0.488938159348629));
#62557=CARTESIAN_POINT('Ctrl Pts',(-0.0121015222283782,0.80178653988071,
-0.494233692180094));
#62558=CARTESIAN_POINT('Ctrl Pts',(0.124164937843389,0.793523744454159,
-0.499529225011559));
#62559=CARTESIAN_POINT('Ctrl Pts',(0.248760203786074,0.75198051656646,-0.504824757843024));
#62560=CARTESIAN_POINT('Ctrl Pts',(0.497950735671431,0.668894060791067,
-0.515415823505954));
#62561=CARTESIAN_POINT('Ctrl Pts',(0.700456491040463,0.452685875171097,
-0.526006889168883));
#62562=CARTESIAN_POINT('Ctrl Pts',(0.766683676846839,0.19891565103887,-0.536597954831812));
#62563=CARTESIAN_POINT('Ctrl Pts',(0.799797269750025,0.0720305389727643,
-0.541893487663276));
#62564=CARTESIAN_POINT('Ctrl Pts',(0.798841220262551,-0.0642450827214051,
-0.54718902049474));
#62565=CARTESIAN_POINT('Ctrl Pts',(0.76676938702351,-0.19237867589465,-0.552484553326204));
#62566=CARTESIAN_POINT('Ctrl Pts',(0.734697553784463,-0.320512269067924,
-0.55778008615767));
#62567=CARTESIAN_POINT('Ctrl Pts',(0.671509936793835,-0.440503833720271,
-0.563075618989136));
#62568=CARTESIAN_POINT('Ctrl Pts',(0.58243650440451,-0.536644159129025,
-0.568371151820601));
#62569=CARTESIAN_POINT('Ctrl Pts',(0.4042896396259,-0.728924809946489,-0.57896221748353));
#62570=CARTESIAN_POINT('Ctrl Pts',(0.122599513252553,-0.825800503789633,
-0.589553283146457));
#62571=CARTESIAN_POINT('Ctrl Pts',(-0.135432224195654,-0.780996074233637,
-0.600144348809386));
#62572=CARTESIAN_POINT('Ctrl Pts',(-0.393463961643877,-0.736191644677638,
-0.610735414472315));
#62573=CARTESIAN_POINT('Ctrl Pts',(-0.627837310166959,-0.549707091722483,
-0.621326480135245));
#62574=CARTESIAN_POINT('Ctrl Pts',(-0.729928286435418,-0.308636876853086,
-0.631917545798174));
#62575=CARTESIAN_POINT('Ctrl Pts',(-0.770893280580547,-0.211905115617681,
-0.63616731359089));
#62576=CARTESIAN_POINT('Ctrl Pts',(-0.79055957674958,-0.106384552767054,
-0.640417081383606));
#62577=CARTESIAN_POINT('Ctrl Pts',(-0.789917699687958,-0.00064740280164427,
-0.644666849176321));
#62578=CARTESIAN_POINT('Ctrl Pts',(-0.789692040475088,-0.000106295414249275,
-0.673133150823697));
#62579=CARTESIAN_POINT('Ctrl Pts',(-0.790252451913751,-0.0991149986681245,
-0.669151522538878));
#62580=CARTESIAN_POINT('Ctrl Pts',(-0.772988227439065,-0.198061641529546,
-0.665169894254059));
#62581=CARTESIAN_POINT('Ctrl Pts',(-0.737043873044512,-0.290039067860967,
-0.661188265969241));
#62582=CARTESIAN_POINT('Ctrl Pts',(-0.689238177689206,-0.412368287479148,
-0.655892733137777));
#62583=CARTESIAN_POINT('Ctrl Pts',(-0.608389609690481,-0.522369812631978,
-0.650597200306314));
#62584=CARTESIAN_POINT('Ctrl Pts',(-0.50704122135461,-0.60684755250419,
-0.64530166747485));
#62585=CARTESIAN_POINT('Ctrl Pts',(-0.405692833018717,-0.691325292376421,
-0.640006134643385));
#62586=CARTESIAN_POINT('Ctrl Pts',(-0.283844624345669,-0.750279246968022,
-0.63471060181192));
#62587=CARTESIAN_POINT('Ctrl Pts',(-0.155209837063072,-0.775961441139558,
-0.629415068980455));
#62588=CARTESIAN_POINT('Ctrl Pts',(-0.0265750497804897,-0.80164363531109,
-0.62411953614899));
#62589=CARTESIAN_POINT('Ctrl Pts',(0.10884631611164,-0.794054069062565,
-0.618824003317526));
#62590=CARTESIAN_POINT('Ctrl Pts',(0.234851914639674,-0.75510659557873,
-0.613528470486062));
#62591=CARTESIAN_POINT('Ctrl Pts',(0.360857513167722,-0.71615912209489,
-0.608232937654597));
#62592=CARTESIAN_POINT('Ctrl Pts',(0.477447344331671,-0.645853741375732,
-0.602937404823133));
#62593=CARTESIAN_POINT('Ctrl Pts',(0.568580117099377,-0.551299994986477,
-0.597641871991668));
#62594=CARTESIAN_POINT('Ctrl Pts',(0.750845662634779,-0.362192502207977,
-0.587050806328739));
#62595=CARTESIAN_POINT('Ctrl Pts',(0.83128297458522,-0.0760915467490993,
-0.576459740665809));
#62596=CARTESIAN_POINT('Ctrl Pts',(0.772037630551969,0.178913169173971,
-0.56586867500288));
#62597=CARTESIAN_POINT('Ctrl Pts',(0.712792286518719,0.433917885097042,
-0.55527760933995));
#62598=CARTESIAN_POINT('Ctrl Pts',(0.513864286501777,0.657826361484306,
-0.544686543677022));
#62599=CARTESIAN_POINT('Ctrl Pts',(0.267335844472759,0.746209288054612,
-0.534095478014093));
#62600=CARTESIAN_POINT('Ctrl Pts',(0.0208074024437416,0.834592214624919,
-0.523504412351164));
#62601=CARTESIAN_POINT('Ctrl Pts',(-0.273321481597352,0.787449591378269,
-0.512913346688235));
#62602=CARTESIAN_POINT('Ctrl Pts',(-0.481798547418916,0.628561369235547,
-0.502322281025305));
#62603=CARTESIAN_POINT('Ctrl Pts',(-0.586037080329692,0.54911725816419,
-0.497026748193841));
#62604=CARTESIAN_POINT('Ctrl Pts',(-0.668862658685588,0.441736747368818,
-0.491731215362376));
#62605=CARTESIAN_POINT('Ctrl Pts',(-0.722429270106406,0.320999684593171,
-0.486435682530912));
#62606=CARTESIAN_POINT('Ctrl Pts',(-0.767282896080836,0.219901352790059,
-0.482001505295174));
#62607=CARTESIAN_POINT('Ctrl Pts',(-0.79162179447004,0.10943816453247,-0.477567328059436));
#62608=CARTESIAN_POINT('Ctrl Pts',(-0.791972558534597,-0.000546350253884251,
-0.473133150823699));
#62609=CARTESIAN_POINT('Origin',(0.,0.,-5.925));
#62610=CARTESIAN_POINT('',(-0.7911,5.70765656959793E-13,-0.244666849176319));
#62611=CARTESIAN_POINT('',(-0.791468851257481,0.000547557155766596,-0.273133150823697));
#62612=CARTESIAN_POINT('',(-0.7911,-9.68818082805471E-17,-5.925));
#62613=CARTESIAN_POINT('Ctrl Pts',(-0.790957246177156,0.000419304332940074,
-0.244666849176318));
#62614=CARTESIAN_POINT('Ctrl Pts',(-0.791091484198145,0.0498428586940881,
-0.246657626761787));
#62615=CARTESIAN_POINT('Ctrl Pts',(-0.786624458151161,0.0992128624228036,
-0.248648404347256));
#62616=CARTESIAN_POINT('Ctrl Pts',(-0.777442989937871,0.147665862313506,
-0.250639181932724));
#62617=CARTESIAN_POINT('Ctrl Pts',(-0.753019987228064,0.276552410754211,
-0.255934714764189));
#62618=CARTESIAN_POINT('Ctrl Pts',(-0.695238665495522,0.398950448890937,
-0.261230247595654));
#62619=CARTESIAN_POINT('Ctrl Pts',(-0.611746352354572,0.501110679595837,
-0.266525780427119));
#62620=CARTESIAN_POINT('Ctrl Pts',(-0.528254039213631,0.603270910300727,
-0.271821313258583));
#62621=CARTESIAN_POINT('Ctrl Pts',(-0.419050734664292,0.68519333357379,
-0.277116846090047));
#62622=CARTESIAN_POINT('Ctrl Pts',(-0.297195225769133,0.734189991186984,
-0.282412378921512));
#62623=CARTESIAN_POINT('Ctrl Pts',(-0.0534842079788134,0.832183306413372,
-0.293003444584441));
#62624=CARTESIAN_POINT('Ctrl Pts',(0.240835627194766,0.798473559000276,
-0.303594510247369));
#62625=CARTESIAN_POINT('Ctrl Pts',(0.455592400909156,0.647924259310542,
-0.314185575910298));
#62626=CARTESIAN_POINT('Ctrl Pts',(0.562970787766375,0.572649609465658,
-0.319481108741763));
#62627=CARTESIAN_POINT('Ctrl Pts',(0.650458409258781,0.468165071551605,
-0.324776641573228));
#62628=CARTESIAN_POINT('Ctrl Pts',(0.708960624034482,0.349741654396658,
-0.330072174404694));
#62629=CARTESIAN_POINT('Ctrl Pts',(0.767462838810163,0.231318237241752,
-0.335367707236158));
#62630=CARTESIAN_POINT('Ctrl Pts',(0.79697964686916,0.0989559408459271,
-0.340663240067623));
#62631=CARTESIAN_POINT('Ctrl Pts',(0.791325851080046,-0.0319838013192029,
-0.345958772899087));
#62632=CARTESIAN_POINT('Ctrl Pts',(0.780018259501817,-0.293863285649508,
-0.356549838562016));
#62633=CARTESIAN_POINT('Ctrl Pts',(0.628028252531147,-0.55005255305717,
-0.367140904224945));
#62634=CARTESIAN_POINT('Ctrl Pts',(0.402354296443651,-0.682940171345567,
-0.377731969887874));
#62635=CARTESIAN_POINT('Ctrl Pts',(0.176680340356142,-0.815827789633971,
-0.388323035550804));
#62636=CARTESIAN_POINT('Ctrl Pts',(-0.122677564848187,-0.825413758803086,
-0.398914101213734));
#62637=CARTESIAN_POINT('Ctrl Pts',(-0.356547662793433,-0.707761206253896,
-0.409505166876663));
#62638=CARTESIAN_POINT('Ctrl Pts',(-0.590417760738652,-0.59010865370472,
-0.420096232539592));
#62639=CARTESIAN_POINT('Ctrl Pts',(-0.758800051424793,-0.345217579437281,
-0.43068729820252));
#62640=CARTESIAN_POINT('Ctrl Pts',(-0.78748647732005,-0.0841439365083014,
-0.441278363865449));
#62641=CARTESIAN_POINT('Ctrl Pts',(-0.790545770749094,-0.0563014690212264,
-0.442407858969073));
#62642=CARTESIAN_POINT('Ctrl Pts',(-0.79201625062994,-0.0282749511016459,
-0.443537354072697));
#62643=CARTESIAN_POINT('Ctrl Pts',(-0.791944510864312,-0.00022813924889703,
-0.444666849176321));
#62644=CARTESIAN_POINT('Ctrl Pts',(-0.791972558534597,-0.000546350253884251,
-0.473133150823699));
#62645=CARTESIAN_POINT('Ctrl Pts',(-0.792040695772629,-0.021911255673313,
-0.472271795227972));
#62646=CARTESIAN_POINT('Ctrl Pts',(-0.791203652207818,-0.0432580985777029,
-0.471410439632245));
#62647=CARTESIAN_POINT('Ctrl Pts',(-0.789435967515537,-0.0645147251750589,
-0.470549084036518));
#62648=CARTESIAN_POINT('Ctrl Pts',(-0.767700850520675,-0.325882189648303,
-0.459958018373589));
#62649=CARTESIAN_POINT('Ctrl Pts',(-0.605264921593145,-0.573610124044309,
-0.449366952710658));
#62650=CARTESIAN_POINT('Ctrl Pts',(-0.37401057509831,-0.698192255756164,
-0.438775887047729));
#62651=CARTESIAN_POINT('Ctrl Pts',(-0.258383401850899,-0.760483321612088,
-0.433480354216265));
#62652=CARTESIAN_POINT('Ctrl Pts',(-0.125551624211664,-0.791987936796978,
-0.428184821384802));
#62653=CARTESIAN_POINT('Ctrl Pts',(0.00638206399365039,-0.790767982704263,
-0.422889288553338));
#62654=CARTESIAN_POINT('Ctrl Pts',(0.138315752198995,-0.789548028611547,
-0.417593755721872));
#62655=CARTESIAN_POINT('Ctrl Pts',(0.269351350970419,-0.755603505241211,
-0.412298222890406));
#62656=CARTESIAN_POINT('Ctrl Pts',(0.384021022517093,-0.691906175253571,
-0.40700269005894));
#62657=CARTESIAN_POINT('Ctrl Pts',(0.498690694063741,-0.628208845265947,
-0.401707157227476));
#62658=CARTESIAN_POINT('Ctrl Pts',(0.596994438385647,-0.534758708661034,
-0.396411624396013));
#62659=CARTESIAN_POINT('Ctrl Pts',(0.667822021137814,-0.423503296328635,
-0.391116091564548));
#62660=CARTESIAN_POINT('Ctrl Pts',(0.738649603889981,-0.312247883996236,
-0.385820558733084));
#62661=CARTESIAN_POINT('Ctrl Pts',(0.782001025072408,-0.183187195936352,
-0.380525025901619));
#62662=CARTESIAN_POINT('Ctrl Pts',(0.790251999425748,-0.0521241922399114,
-0.375229493070155));
#62663=CARTESIAN_POINT('Ctrl Pts',(0.80675394813243,0.210001815152985,-0.364638427407225));
#62664=CARTESIAN_POINT('Ctrl Pts',(0.682854109522748,0.480137085092108,
-0.354047361744297));
#62665=CARTESIAN_POINT('Ctrl Pts',(0.472620005630473,0.636146595683167,
-0.343456296081368));
#62666=CARTESIAN_POINT('Ctrl Pts',(0.262385901738198,0.792156106274226,
-0.332865230418439));
#62667=CARTESIAN_POINT('Ctrl Pts',(-0.034182467436671,0.83403985751722,
-0.322274164755509));
#62668=CARTESIAN_POINT('Ctrl Pts',(-0.279299302753248,0.741814098670096,
-0.31168309909258));
#62669=CARTESIAN_POINT('Ctrl Pts',(-0.524416138069826,0.649588339822972,
-0.301092033429651));
#62670=CARTESIAN_POINT('Ctrl Pts',(-0.718081439528112,0.423253070885729,
-0.290500967766722));
#62671=CARTESIAN_POINT('Ctrl Pts',(-0.774123310097696,0.167190510788659,
-0.279909902103793));
#62672=CARTESIAN_POINT('Ctrl Pts',(-0.786076209211229,0.112576167682588,
-0.277650985010427));
#62673=CARTESIAN_POINT('Ctrl Pts',(-0.791768541684542,0.0566095135191815,
-0.275392067917062));
#62674=CARTESIAN_POINT('Ctrl Pts',(-0.791468851257481,0.000547557155766596,
-0.273133150823697));
#62675=CARTESIAN_POINT('Origin',(0.,0.,-5.925));
#62676=CARTESIAN_POINT('',(-0.7911,-9.68818082805471E-17,-0.0599999999999969));
#62677=CARTESIAN_POINT('',(-0.789664670674245,0.000390155355157968,-0.0731331508236992));
#62678=CARTESIAN_POINT('',(-0.7911,-9.68818082805471E-17,-5.925));
#62679=CARTESIAN_POINT('',(-0.701077753000047,0.366509473613445,-0.0599999999999987));
#62680=CARTESIAN_POINT('Origin',(0.,0.,-0.0599999999999996));
#62681=CARTESIAN_POINT('Ctrl Pts',(-0.701077753000086,0.366509473613371,
-0.0599999999999969));
#62682=CARTESIAN_POINT('Ctrl Pts',(-0.599076100370241,0.561623364457742,
-0.0688587435732708));
#62683=CARTESIAN_POINT('Ctrl Pts',(-0.41201304761304,0.710322621163273,
-0.0777174871465436));
#62684=CARTESIAN_POINT('Ctrl Pts',(-0.198919167149933,0.765682946747789,
-0.0865762307198175));
#62685=CARTESIAN_POINT('Ctrl Pts',(0.0141747133131744,0.821043272332304,
-0.0954349742930914));
#62686=CARTESIAN_POINT('Ctrl Pts',(0.249960728318654,0.782197297258215,
-0.104293717866366));
#62687=CARTESIAN_POINT('Ctrl Pts',(0.434033038607528,0.661403455840016,
-0.11315246143964));
#62688=CARTESIAN_POINT('Ctrl Pts',(0.618105348896402,0.540609614421817,
-0.122011205012914));
#62689=CARTESIAN_POINT('Ctrl Pts',(0.747579962856046,0.339760469560251,
-0.130869948586188));
#62690=CARTESIAN_POINT('Ctrl Pts',(0.781599209966111,0.12223700331876,-0.139728692159462));
#62691=CARTESIAN_POINT('Ctrl Pts',(0.815618457076177,-0.0952864629227309,
-0.148587435732736));
#62692=CARTESIAN_POINT('Ctrl Pts',(0.753649333631875,-0.32607615591435,
-0.157446179306009));
#62693=CARTESIAN_POINT('Ctrl Pts',(0.615247132757394,-0.497302901292367,
-0.166304922879283));
#62694=CARTESIAN_POINT('Ctrl Pts',(0.476844931882912,-0.668529646670385,
-0.175163666452556));
#62695=CARTESIAN_POINT('Ctrl Pts',(0.264178099151975,-0.777510713410496,
-0.184022410025831));
#62696=CARTESIAN_POINT('Ctrl Pts',(0.0443568665752726,-0.789855479431284,
-0.192881153599105));
#62697=CARTESIAN_POINT('Ctrl Pts',(-0.17546436600143,-0.802200245452072,
-0.201739897172379));
#62698=CARTESIAN_POINT('Ctrl Pts',(-0.398995903057064,-0.717715296537093,
-0.210598640745653));
#62699=CARTESIAN_POINT('Ctrl Pts',(-0.555698990988761,-0.563061134703926,
-0.219457384318927));
#62700=CARTESIAN_POINT('Ctrl Pts',(-0.70434313206,-0.416360547292378,-0.227860539271391));
#62701=CARTESIAN_POINT('Ctrl Pts',(-0.791100000000151,-0.20884478212649,
-0.236263694223855));
#62702=CARTESIAN_POINT('Ctrl Pts',(-0.7911,5.70765656959793E-13,-0.244666849176319));
#62703=CARTESIAN_POINT('Ctrl Pts',(-0.791468851257481,0.000547557155766596,
-0.273133150823697));
#62704=CARTESIAN_POINT('Ctrl Pts',(-0.791065983586929,-0.074815376482576,
-0.270096535085597));
#62705=CARTESIAN_POINT('Ctrl Pts',(-0.779835008433342,-0.150350529500286,
-0.267059919347497));
#62706=CARTESIAN_POINT('Ctrl Pts',(-0.758428280312644,-0.223004338239144,
-0.264023303609398));
#62707=CARTESIAN_POINT('Ctrl Pts',(-0.721097237680188,-0.34970480437989,
-0.258727770777933));
#62708=CARTESIAN_POINT('Ctrl Pts',(-0.652820074852665,-0.467642633822896,
-0.253432237946469));
#62709=CARTESIAN_POINT('Ctrl Pts',(-0.559938392265368,-0.560213600724365,
-0.248136705115005));
#62710=CARTESIAN_POINT('Ctrl Pts',(-0.374175027090764,-0.745355534527313,
-0.237545639452076));
#62711=CARTESIAN_POINT('Ctrl Pts',(-0.089993582877054,-0.829030018164101,
-0.226954573789146));
#62712=CARTESIAN_POINT('Ctrl Pts',(0.166910245748897,-0.774274444394978,
-0.216363508126217));
#62713=CARTESIAN_POINT('Ctrl Pts',(0.29536216006188,-0.746896657510415,
-0.211067975294752));
#62714=CARTESIAN_POINT('Ctrl Pts',(0.416994670477923,-0.68491135627437,
-0.205772442463288));
#62715=CARTESIAN_POINT('Ctrl Pts',(0.516766904098013,-0.598579551649639,
-0.200476909631823));
#62716=CARTESIAN_POINT('Ctrl Pts',(0.616539137718092,-0.512247747024917,
-0.195181376800359));
#62717=CARTESIAN_POINT('Ctrl Pts',(0.694451094542224,-0.401569439011514,
-0.189885843968895));
#62718=CARTESIAN_POINT('Ctrl Pts',(0.740611247050816,-0.278779106530895,
-0.184590311137431));
#62719=CARTESIAN_POINT('Ctrl Pts',(0.786771399559408,-0.155988774050276,
-0.179294778305966));
#62720=CARTESIAN_POINT('Ctrl Pts',(0.801179747752459,-0.0210864171024406,
-0.173999245474501));
#62721=CARTESIAN_POINT('Ctrl Pts',(0.783148445581123,0.109551658983387,
-0.168703712643037));
#62722=CARTESIAN_POINT('Ctrl Pts',(0.765117143409784,0.24018973506923,-0.163408179811572));
#62723=CARTESIAN_POINT('Ctrl Pts',(0.71464619087405,0.366563530293064,-0.158112646980107));
#62724=CARTESIAN_POINT('Ctrl Pts',(0.636094778853461,0.471793541056986,
-0.152817114148643));
#62725=CARTESIAN_POINT('Ctrl Pts',(0.478991954812292,0.682253562584816,
-0.142226048485714));
#62726=CARTESIAN_POINT('Ctrl Pts',(0.209567292831717,0.808138446273004,
-0.131634982822784));
#62727=CARTESIAN_POINT('Ctrl Pts',(-0.0516326420874012,0.790898324967994,
-0.121043917159855));
#62728=CARTESIAN_POINT('Ctrl Pts',(-0.312832577006519,0.773658203662983,
-0.110452851496926));
#62729=CARTESIAN_POINT('Ctrl Pts',(-0.565807784864179,0.613293077364774,
-0.0998617858339976));
#62730=CARTESIAN_POINT('Ctrl Pts',(-0.693025188183458,0.384481595935094,
-0.0892707201710682));
#62731=CARTESIAN_POINT('Ctrl Pts',(-0.757638757569675,0.268268513872607,
-0.083891530388612));
#62732=CARTESIAN_POINT('Ctrl Pts',(-0.789811691001155,0.134398926932358,
-0.0785123406061555));
#62733=CARTESIAN_POINT('Ctrl Pts',(-0.789664670674245,0.000390155355157968,
-0.0731331508236992));
#62734=CARTESIAN_POINT('Origin',(0.,0.,-12.278617978381));
#62735=CARTESIAN_POINT('',(-0.6767,5.98871479897751E-13,-0.17861797838103));
#62736=CARTESIAN_POINT('',(-0.675472231886313,0.000333735468832419,-0.139182021619022));
#62737=CARTESIAN_POINT('',(-0.6767,6.12423655037739E-13,-12.278617978381));
#62738=CARTESIAN_POINT('',(0.564209944071435,0.373617490236885,-0.0599999999999987));
#62739=CARTESIAN_POINT('Ctrl Pts',(-0.6767,5.98871479897751E-13,-0.17861797838103));
#62740=CARTESIAN_POINT('Ctrl Pts',(-0.67670000000009,-0.10198549600935,
-0.173820728251383));
#62741=CARTESIAN_POINT('Ctrl Pts',(-0.653245593890205,-0.203961661393933,
-0.169020603322871));
#62742=CARTESIAN_POINT('Ctrl Pts',(-0.608664118325269,-0.295720951343193,
-0.164221915793792));
#62743=CARTESIAN_POINT('Ctrl Pts',(-0.523085967092649,-0.471861159641993,
-0.155010403570885));
#62744=CARTESIAN_POINT('Ctrl Pts',(-0.357381681450831,-0.607083368831098,
-0.145798891347978));
#62745=CARTESIAN_POINT('Ctrl Pts',(-0.167658291688701,-0.65560169861588,
-0.136587379125071));
#62746=CARTESIAN_POINT('Ctrl Pts',(0.0220650980734294,-0.704120028400661,
-0.127375866902165));
#62747=CARTESIAN_POINT('Ctrl Pts',(0.232341935463792,-0.665048199736589,
-0.118164354679259));
#62748=CARTESIAN_POINT('Ctrl Pts',(0.391973042749502,-0.55161582986504,
-0.108952842456352));
#62749=CARTESIAN_POINT('Ctrl Pts',(0.551604150035213,-0.438183459993492,
-0.0997413302334453));
#62750=CARTESIAN_POINT('Ctrl Pts',(0.657673563169899,-0.252462605657446,
-0.0905298180105381));
#62751=CARTESIAN_POINT('Ctrl Pts',(0.674266461046662,-0.0573378540548125,
-0.0813183057876312));
#62752=CARTESIAN_POINT('Ctrl Pts',(0.687066837440891,0.0931886111168982,
-0.0742122038584208));
#62753=CARTESIAN_POINT('Ctrl Pts',(0.647618097050576,0.247660567562773,
-0.0671061019292091));
#62754=CARTESIAN_POINT('Ctrl Pts',(0.564209944071435,0.373617490236885,
-0.0599999999999987));
#62755=CARTESIAN_POINT('',(0.537060862935828,-0.411689834101626,-0.0599999999999987));
#62756=CARTESIAN_POINT('Origin',(0.,0.,-0.0599999999999987));
#62757=CARTESIAN_POINT('Ctrl Pts',(-0.675472231886313,0.000333735468832488,
-0.139182021619022));
#62758=CARTESIAN_POINT('Ctrl Pts',(-0.67535038361465,-0.110730751752114,
-0.133970145738539));
#62759=CARTESIAN_POINT('Ctrl Pts',(-0.622781870731608,-0.33486777276979,
-0.123462737026592));
#62760=CARTESIAN_POINT('Ctrl Pts',(-0.385645525478233,-0.58933640490133,
-0.107659795483182));
#62761=CARTESIAN_POINT('Ctrl Pts',(-0.0580733210265062,-0.703415543027182,
-0.0917731969887855));
#62762=CARTESIAN_POINT('Ctrl Pts',(0.286592368567594,-0.644628272737791,
-0.0758865984943943));
#62763=CARTESIAN_POINT('Ctrl Pts',(0.468570466391673,-0.501037465313089,
-0.065295532831463));
#62764=CARTESIAN_POINT('Ctrl Pts',(0.537060862935828,-0.411689834101626,
-0.0599999999999987));
#62765=CARTESIAN_POINT('Origin',(0.,0.,-12.278617978381));
#62766=CARTESIAN_POINT('',(-0.67742238718478,-0.000195148311967771,-0.378617978381031));
#62767=CARTESIAN_POINT('',(-0.677015512129869,0.000468375588248721,-0.33918202161902));
#62768=CARTESIAN_POINT('',(-0.6767,6.12423655037739E-13,-12.278617978381));
#62769=CARTESIAN_POINT('Ctrl Pts',(-0.67742238718478,-0.000195148311967774,
-0.378617978381031));
#62770=CARTESIAN_POINT('Ctrl Pts',(-0.677483752750961,-0.0241861451275098,
-0.377488483277405));
#62771=CARTESIAN_POINT('Ctrl Pts',(-0.664431426608646,-0.272956126468997,
-0.365767922510851));
#62772=CARTESIAN_POINT('Ctrl Pts',(-0.361005438736672,-0.714251442192837,
-0.343456296081368));
#62773=CARTESIAN_POINT('Ctrl Pts',(0.407198939161548,-0.689652180392618,
-0.311683099092581));
#62774=CARTESIAN_POINT('Ctrl Pts',(0.732226235701414,-0.141797050653159,
-0.285205434935257));
#62775=CARTESIAN_POINT('Ctrl Pts',(0.631232561002846,0.311089138051407,
-0.264023303609399));
#62776=CARTESIAN_POINT('Ctrl Pts',(0.331887985278457,0.668589766575936,
-0.242841172283542));
#62777=CARTESIAN_POINT('Ctrl Pts',(-0.17162922483904,0.726259811006413,
-0.221659040957683));
#62778=CARTESIAN_POINT('Ctrl Pts',(-0.545275419699615,0.445956922224332,
-0.200476909631823));
#62779=CARTESIAN_POINT('Ctrl Pts',(-0.662707531036891,0.197200756547418,
-0.187895066383429));
#62780=CARTESIAN_POINT('Ctrl Pts',(-0.676692715657785,0.0426351440758945,
-0.180608755966498));
#62781=CARTESIAN_POINT('Ctrl Pts',(-0.676577889632261,0.000358669248252046,
-0.178617978381032));
#62782=CARTESIAN_POINT('Ctrl Pts',(-0.677015512129869,0.000468375588248721,
-0.33918202161902));
#62783=CARTESIAN_POINT('Ctrl Pts',(-0.676670902658741,-0.0639964167176895,
-0.33614540588091));
#62784=CARTESIAN_POINT('Ctrl Pts',(-0.650310658710815,-0.241285123438995,
-0.327813257311336));
#62785=CARTESIAN_POINT('Ctrl Pts',(-0.441609192873322,-0.601783375902012,
-0.308890043078835));
#62786=CARTESIAN_POINT('Ctrl Pts',(0.0445634358699717,-0.744932214423158,
-0.287707911752975));
#62787=CARTESIAN_POINT('Ctrl Pts',(0.460736965378437,-0.532845482801779,
-0.266525780427117));
#62788=CARTESIAN_POINT('Ctrl Pts',(0.660672578510412,-0.248825721585754,
-0.250639181932725));
#62789=CARTESIAN_POINT('Ctrl Pts',(0.697646902447653,0.0973571564825142,
-0.234752583438329));
#62790=CARTESIAN_POINT('Ctrl Pts',(0.524957262296379,0.529753299715826,
-0.213570452112473));
#62791=CARTESIAN_POINT('Ctrl Pts',(-0.0512014684653643,0.798955362640304,
-0.187092787955149));
#62792=CARTESIAN_POINT('Ctrl Pts',(-0.593892650520787,0.454934536693656,
-0.160531466846845));
#62793=CARTESIAN_POINT('Ctrl Pts',(-0.675597991784087,0.114963663071067,
-0.144561211401469));
#62794=CARTESIAN_POINT('Ctrl Pts',(-0.675472231886313,0.000333735468832488,
-0.139182021619022));
#62795=CARTESIAN_POINT('Origin',(0.,0.,-12.278617978381));
#62796=CARTESIAN_POINT('',(-0.67666270498899,-2.04219635818603E-5,-0.578617978381031));
#62797=CARTESIAN_POINT('',(-0.67744637891589,-0.00046734321359837,-0.539182021619019));
#62798=CARTESIAN_POINT('',(-0.6767,6.12423655037739E-13,-12.278617978381));
#62799=CARTESIAN_POINT('Ctrl Pts',(-0.675688670684921,-0.000553782676958534,
-0.578617978381031));
#62800=CARTESIAN_POINT('Ctrl Pts',(-0.676237726692527,-0.0910004131681901,
-0.574368210588314));
#62801=CARTESIAN_POINT('Ctrl Pts',(-0.617491434940766,-0.406206780333588,
-0.559527377132667));
#62802=CARTESIAN_POINT('Ctrl Pts',(-0.136084714826095,-0.789249125190363,
-0.534095478014092));
#62803=CARTESIAN_POINT('Ctrl Pts',(0.466303442539805,-0.582082578534946,
-0.50761781385677));
#62804=CARTESIAN_POINT('Ctrl Pts',(0.682503975557423,-0.171523651470232,
-0.486435682530911));
#62805=CARTESIAN_POINT('Ctrl Pts',(0.685775160935683,0.294752233755149,
-0.465253551205053));
#62806=CARTESIAN_POINT('Ctrl Pts',(0.339331867652397,0.664637404300089,
-0.444071419879196));
#62807=CARTESIAN_POINT('Ctrl Pts',(-0.126912670487204,0.692909095187001,
-0.422889288553336));
#62808=CARTESIAN_POINT('Ctrl Pts',(-0.443257737571659,0.549436516930662,
-0.407002690058943));
#62809=CARTESIAN_POINT('Ctrl Pts',(-0.635922507310959,0.289797886016136,
-0.392245586668175));
#62810=CARTESIAN_POINT('Ctrl Pts',(-0.677196045996511,0.0882934140033878,
-0.38278401610887));
#62811=CARTESIAN_POINT('Ctrl Pts',(-0.67742238718478,-0.000195148311967774,
-0.378617978381031));
#62812=CARTESIAN_POINT('Ctrl Pts',(-0.67744637891589,-0.000467343213598401,
-0.539182021619019));
#62813=CARTESIAN_POINT('Ctrl Pts',(-0.677504662911581,-0.018742695883905,
-0.538320666023284));
#62814=CARTESIAN_POINT('Ctrl Pts',(-0.667984865883078,-0.261522904938053,
-0.526868244764619));
#62815=CARTESIAN_POINT('Ctrl Pts',(-0.448265169876774,-0.596613218990799,
-0.510120290674488));
#62816=CARTESIAN_POINT('Ctrl Pts',(0.00622737937602623,-0.704408304798551,
-0.488938159348631));
#62817=CARTESIAN_POINT('Ctrl Pts',(0.342487484376452,-0.61730076227034,
-0.473051560854236));
#62818=CARTESIAN_POINT('Ctrl Pts',(0.594751965918543,-0.377491481115471,
-0.457164962359842));
#62819=CARTESIAN_POINT('Ctrl Pts',(0.743081667418538,0.0640980403615866,
-0.435982831033984));
#62820=CARTESIAN_POINT('Ctrl Pts',(0.478124579859611,0.641776390658052,
-0.409505166876661));
#62821=CARTESIAN_POINT('Ctrl Pts',(-0.282921364094237,0.749257370810349,
-0.377731969887874));
#62822=CARTESIAN_POINT('Ctrl Pts',(-0.649573297565699,0.320753847754227,
-0.354290921468661));
#62823=CARTESIAN_POINT('Ctrl Pts',(-0.677271864692064,0.0484232812524634,
-0.341440938712375));
#62824=CARTESIAN_POINT('Ctrl Pts',(-0.677015512129869,0.000468375588248721,
-0.33918202161902));
#62825=CARTESIAN_POINT('Origin',(0.,0.,-12.278617978381));
#62826=CARTESIAN_POINT('',(-0.6767,5.55100064568364E-13,-0.778617978381028));
#62827=CARTESIAN_POINT('',(-0.676541475852966,-1.19679499782825E-5,-0.73918202161902));
#62828=CARTESIAN_POINT('',(-0.6767,6.12423655037739E-13,-12.278617978381));
#62829=CARTESIAN_POINT('Ctrl Pts',(-0.6767,5.55100064568364E-13,-0.778617978381028));
#62830=CARTESIAN_POINT('Ctrl Pts',(-0.676700000000037,-0.0455605697071119,
-0.776474875121369));
#62831=CARTESIAN_POINT('Ctrl Pts',(-0.672073181934436,-0.0912183166350835,
-0.774327141130771));
#62832=CARTESIAN_POINT('Ctrl Pts',(-0.662913553532106,-0.135898898242169,
-0.772181722505643));
#62833=CARTESIAN_POINT('Ctrl Pts',(-0.623586017172946,-0.327738252473403,
-0.762970210282736));
#62834=CARTESIAN_POINT('Ctrl Pts',(-0.496498716511246,-0.499760850258025,
-0.75375869805983));
#62835=CARTESIAN_POINT('Ctrl Pts',(-0.324683073455861,-0.593720297624442,
-0.744547185836923));
#62836=CARTESIAN_POINT('Ctrl Pts',(-0.152867430400476,-0.68767974499086,
-0.735335673614017));
#62837=CARTESIAN_POINT('Ctrl Pts',(0.0605380174147123,-0.70185969495009,
-0.726124161391109));
#62838=CARTESIAN_POINT('Ctrl Pts',(0.243274753090137,-0.631458854169401,
-0.716912649168203));
#62839=CARTESIAN_POINT('Ctrl Pts',(0.426011488765561,-0.561058013388712,
-0.707701136945296));
#62840=CARTESIAN_POINT('Ctrl Pts',(0.574741480258209,-0.407362386357087,
-0.698489624722388));
#62841=CARTESIAN_POINT('Ctrl Pts',(0.639105148120741,-0.222412903505094,
-0.689278112499482));
#62842=CARTESIAN_POINT('Ctrl Pts',(0.703468815983272,-0.037463420653101,
-0.680066600276575));
#62843=CARTESIAN_POINT('Ctrl Pts',(0.682290436106702,0.175361465964632,
-0.670855088053667));
#62844=CARTESIAN_POINT('Ctrl Pts',(0.582740951575584,0.343999815925508,
-0.661643575830761));
#62845=CARTESIAN_POINT('Ctrl Pts',(0.483191467044466,0.512638165886383,
-0.652432063607854));
#62846=CARTESIAN_POINT('Ctrl Pts',(0.307089337447684,0.634009480823339,
-0.643220551384948));
#62847=CARTESIAN_POINT('Ctrl Pts',(0.114062275375495,0.667017756387463,
-0.634009039162041));
#62848=CARTESIAN_POINT('Ctrl Pts',(-0.0789647866966941,0.700026031951587,
-0.624797526939135));
#62849=CARTESIAN_POINT('Ctrl Pts',(-0.28539077693003,0.644068309569111,
-0.615586014716227));
#62850=CARTESIAN_POINT('Ctrl Pts',(-0.435320404194442,0.518091725172278,
-0.60637450249332));
#62851=CARTESIAN_POINT('Ctrl Pts',(-0.585250031458855,0.392115140775446,
-0.597162990270414));
#62852=CARTESIAN_POINT('Ctrl Pts',(-0.675944547586627,0.198420894907385,
-0.587951478047506));
#62853=CARTESIAN_POINT('Ctrl Pts',(-0.676695030694978,0.00259334392683,
-0.5787399658246));
#62854=CARTESIAN_POINT('Ctrl Pts',(-0.676698343560937,0.0017289001834459,
-0.57869930334341));
#62855=CARTESIAN_POINT('Ctrl Pts',(-0.676699999999999,0.000864381983809313,
-0.578658637658509));
#62856=CARTESIAN_POINT('Ctrl Pts',(-0.6767,6.08156477887935E-13,-0.578617978381031));
#62857=CARTESIAN_POINT('Ctrl Pts',(-0.675495643773846,-9.09241642347361E-5,
-0.739182021619016));
#62858=CARTESIAN_POINT('Ctrl Pts',(-0.675975014802293,-0.0847821003644994,
-0.735200393334189));
#62859=CARTESIAN_POINT('Ctrl Pts',(-0.641566474247868,-0.281988153762673,
-0.725923232217898));
#62860=CARTESIAN_POINT('Ctrl Pts',(-0.451253979159214,-0.540924894803379,
-0.711350538270144));
#62861=CARTESIAN_POINT('Ctrl Pts',(-0.138570312837484,-0.69221098153884,
-0.695463939775748));
#62862=CARTESIAN_POINT('Ctrl Pts',(0.208944432324475,-0.672734836372497,
-0.679577341281356));
#62863=CARTESIAN_POINT('Ctrl Pts',(0.607864107453516,-0.432180412746452,
-0.658395209955497));
#62864=CARTESIAN_POINT('Ctrl Pts',(0.77987753494969,0.179640205882728,-0.631917545798173));
#62865=CARTESIAN_POINT('Ctrl Pts',(0.269393736650696,0.754228245212569,
-0.600144348809387));
#62866=CARTESIAN_POINT('Ctrl Pts',(-0.359594431187155,0.653414779307557,
-0.573666684652064));
#62867=CARTESIAN_POINT('Ctrl Pts',(-0.631463554648116,0.300945820729597,
-0.553345908921941));
#62868=CARTESIAN_POINT('Ctrl Pts',(-0.677146338412084,0.093612445884841,
-0.543616198854748));
#62869=CARTESIAN_POINT('Ctrl Pts',(-0.67744637891589,-0.000467343213598401,
-0.539182021619019));
#62870=CARTESIAN_POINT('Origin',(0.,0.,-12.278617978381));
#62871=CARTESIAN_POINT('',(-0.678025555836318,-0.000211487647944881,-0.978617978381028));
#62872=CARTESIAN_POINT('',(-0.6767,5.52151526765261E-13,-0.939182021619017));
#62873=CARTESIAN_POINT('',(-0.6767,6.12423655037739E-13,-12.278617978381));
#62874=CARTESIAN_POINT('Ctrl Pts',(-0.678025555836318,-0.00021148764794485,
-0.978617978381028));
#62875=CARTESIAN_POINT('Ctrl Pts',(-0.677787583882777,-0.222089071976444,
-0.968127665210128));
#62876=CARTESIAN_POINT('Ctrl Pts',(-0.496832240698866,-0.555074107827601,
-0.952341819207762));
#62877=CARTESIAN_POINT('Ctrl Pts',(-0.0587849258484244,-0.701267695135047,
-0.931260440373935));
#62878=CARTESIAN_POINT('Ctrl Pts',(0.401871301811429,-0.629019792526908,
-0.910078309048076));
#62879=CARTESIAN_POINT('Ctrl Pts',(0.710799778962247,-0.227272191175134,
-0.888896177722219));
#62880=CARTESIAN_POINT('Ctrl Pts',(0.663227825248934,0.237399973442935,
-0.867714046396359));
#62881=CARTESIAN_POINT('Ctrl Pts',(0.470440577277662,0.526349159381354,
-0.851827447901968));
#62882=CARTESIAN_POINT('Ctrl Pts',(0.16104219249472,0.685780831357495,-0.83594084940757));
#62883=CARTESIAN_POINT('Ctrl Pts',(-0.304766616737118,0.680731951966365,
-0.814758718081714));
#62884=CARTESIAN_POINT('Ctrl Pts',(-0.635643959619811,0.363131720955057,
-0.795651094406201));
#62885=CARTESIAN_POINT('Ctrl Pts',(-0.676734292027046,0.0694989861940519,
-0.781839003562151));
#62886=CARTESIAN_POINT('Ctrl Pts',(-0.676179486370995,0.000828682045256053,
-0.77861797838103));
#62887=CARTESIAN_POINT('Ctrl Pts',(-0.6767,5.52151526765261E-13,-0.939182021619017));
#62888=CARTESIAN_POINT('Ctrl Pts',(-0.676700000000007,-0.00844923571080296,
-0.938784581799655));
#62889=CARTESIAN_POINT('Ctrl Pts',(-0.676541534771158,-0.0169092373903444,
-0.93838663555165));
#62890=CARTESIAN_POINT('Ctrl Pts',(-0.676224715602058,-0.0253579180714143,
-0.937988942517967));
#62891=CARTESIAN_POINT('Ctrl Pts',(-0.668886433556761,-0.221049365417898,
-0.92877743029506));
#62892=CARTESIAN_POINT('Ctrl Pts',(-0.571726805262928,-0.411582729340996,
-0.919565918072152));
#62893=CARTESIAN_POINT('Ctrl Pts',(-0.417643822383386,-0.532443919699525,
-0.910354405849246));
#62894=CARTESIAN_POINT('Ctrl Pts',(-0.263560839503844,-0.653305110058055,
-0.901142893626339));
#62895=CARTESIAN_POINT('Ctrl Pts',(-0.0553691191008583,-0.702286368654506,
-0.891931381403432));
#62896=CARTESIAN_POINT('Ctrl Pts',(0.136438176157497,-0.662802771634832,
-0.882719869180525));
#62897=CARTESIAN_POINT('Ctrl Pts',(0.328245471415853,-0.623319174615159,
-0.873508356957618));
#62898=CARTESIAN_POINT('Ctrl Pts',(0.500164618562822,-0.496091964544725,
-0.864296844734711));
#62899=CARTESIAN_POINT('Ctrl Pts',(0.593984251737507,-0.32419993628598,
-0.855085332511804));
#62900=CARTESIAN_POINT('Ctrl Pts',(0.687803884912193,-0.152307908027235,
-0.845873820288897));
#62901=CARTESIAN_POINT('Ctrl Pts',(0.701810211096223,0.0611090054657547,
-0.836662308065991));
#62902=CARTESIAN_POINT('Ctrl Pts',(0.631260725505247,0.243788405045419,
-0.827450795843085));
#62903=CARTESIAN_POINT('Ctrl Pts',(0.560711239914272,0.426467804625083,
-0.818239283620178));
#62904=CARTESIAN_POINT('Ctrl Pts',(0.406894662315832,0.575072705600625,
-0.80902777139727));
#62905=CARTESIAN_POINT('Ctrl Pts',(0.221892876680649,0.639285883841014,
-0.799816259174364));
#62906=CARTESIAN_POINT('Ctrl Pts',(0.036891091045467,0.703499062081403,
-0.790604746951457));
#62907=CARTESIAN_POINT('Ctrl Pts',(-0.175916495162588,0.682147542455185,
-0.781393234728549));
#62908=CARTESIAN_POINT('Ctrl Pts',(-0.344473799393609,0.582460892705538,
-0.772181722505643));
#62909=CARTESIAN_POINT('Ctrl Pts',(-0.51303110362463,0.48277424295589,-0.762970210282736));
#62910=CARTESIAN_POINT('Ctrl Pts',(-0.634259107965074,0.306573428253798,
-0.753758698059829));
#62911=CARTESIAN_POINT('Ctrl Pts',(-0.667110332652752,0.113519575703642,
-0.744547185836922));
#62912=CARTESIAN_POINT('Ctrl Pts',(-0.673488301544418,0.0760387366272504,
-0.742758797764287));
#62913=CARTESIAN_POINT('Ctrl Pts',(-0.676699999999968,0.0379746730511501,
-0.740968295278925));
#62914=CARTESIAN_POINT('Ctrl Pts',(-0.6767,5.66741998541723E-13,-0.739182021619017));
#62915=CARTESIAN_POINT('Origin',(0.,0.,-12.278617978381));
#62916=CARTESIAN_POINT('',(-0.675858962494509,-0.000507684201011625,-1.17861797838103));
#62917=CARTESIAN_POINT('',(-0.676874835700589,0.000126426303653261,-1.13918202161902));
#62918=CARTESIAN_POINT('',(-0.6767,6.12423655037739E-13,-12.278617978381));
#62919=CARTESIAN_POINT('Ctrl Pts',(-0.675858962494509,-0.000507684201011542,
-1.17861797838103));
#62920=CARTESIAN_POINT('Ctrl Pts',(-0.676345794384335,-0.0647735879750859,
-1.17559845818397));
#62921=CARTESIAN_POINT('Ctrl Pts',(-0.653229074319601,-0.241425877431507,
-1.16728340515544));
#62922=CARTESIAN_POINT('Ctrl Pts',(-0.498772672191106,-0.496445232852937,
-1.15367281929545));
#62923=CARTESIAN_POINT('Ctrl Pts',(-0.100894871170555,-0.739585470098981,
-1.13249068796959));
#62924=CARTESIAN_POINT('Ctrl Pts',(0.394639860164164,-0.633362736055885,
-1.11130855664373));
#62925=CARTESIAN_POINT('Ctrl Pts',(0.659187605562879,-0.248398060071516,
-1.09012642531787));
#62926=CARTESIAN_POINT('Ctrl Pts',(0.699298891271897,0.0966376479255593,
-1.07423982682348));
#62927=CARTESIAN_POINT('Ctrl Pts',(0.566686762943658,0.418444798182639,
-1.05835322832909));
#62928=CARTESIAN_POINT('Ctrl Pts',(0.208383162066687,0.716139049954344,
-1.03717109700323));
#62929=CARTESIAN_POINT('Ctrl Pts',(-0.425983270133073,0.677508544252163,
-1.0106934328459));
#62930=CARTESIAN_POINT('Ctrl Pts',(-0.677095589286557,0.228064891222822,
-0.989410549028017));
#62931=CARTESIAN_POINT('Ctrl Pts',(-0.678027841398909,0.00191949921416389,
-0.978718730873058));
#62932=CARTESIAN_POINT('Ctrl Pts',(-0.678025555836318,-0.00021148764794485,
-0.978617978381028));
#62933=CARTESIAN_POINT('Ctrl Pts',(-0.676874835700589,0.00012642630365326,
-1.13918202161902));
#62934=CARTESIAN_POINT('Ctrl Pts',(-0.676728340351803,-0.104284756028837,
-1.13425538078747));
#62935=CARTESIAN_POINT('Ctrl Pts',(-0.624782516817017,-0.321261817775614,
-1.12403320712446));
#62936=CARTESIAN_POINT('Ctrl Pts',(-0.328086109575231,-0.669804587776323,
-1.10321996779852));
#62937=CARTESIAN_POINT('Ctrl Pts',(0.303509663064016,-0.740514320182075,
-1.0767423036412));
#62938=CARTESIAN_POINT('Ctrl Pts',(0.787888271911223,-0.143754323166431,
-1.04496910665241));
#62939=CARTESIAN_POINT('Ctrl Pts',(0.586590198965058,0.460620189913425,
-1.01849144249509));
#62940=CARTESIAN_POINT('Ctrl Pts',(0.178153413511559,0.680803502488938,
-0.99730931116923));
#62941=CARTESIAN_POINT('Ctrl Pts',(-0.288068623095297,0.688609403797382,
-0.976127179843373));
#62942=CARTESIAN_POINT('Ctrl Pts',(-0.629476800536546,0.375015729132091,
-0.956751416659968));
#62943=CARTESIAN_POINT('Ctrl Pts',(-0.677013369793962,0.074595539042017,
-0.942671186308028));
#62944=CARTESIAN_POINT('Ctrl Pts',(-0.676726131492095,0.000143228251020609,
-0.939182021619018));
#62945=CARTESIAN_POINT('Origin',(0.,0.,-12.278617978381));
#62946=CARTESIAN_POINT('',(-0.676309172935686,0.00035385414077456,-1.37861797838103));
#62947=CARTESIAN_POINT('',(-0.676973562981676,-0.000235536917071982,-1.33918202161902));
#62948=CARTESIAN_POINT('',(-0.6767,6.12423655037739E-13,-12.278617978381));
#62949=CARTESIAN_POINT('Ctrl Pts',(-0.676309172935686,0.000353854140774549,
-1.37861797838103));
#62950=CARTESIAN_POINT('Ctrl Pts',(-0.676266745049917,-0.0176411785517731,
-1.37777371832634));
#62951=CARTESIAN_POINT('Ctrl Pts',(-0.670883252141012,-0.148573698829888,
-1.37163392544018));
#62952=CARTESIAN_POINT('Ctrl Pts',(-0.555673590256809,-0.498390713899415,
-1.3549030668911));
#62953=CARTESIAN_POINT('Ctrl Pts',(-0.109218024599217,-0.738214330501128,
-1.33372093556524));
#62954=CARTESIAN_POINT('Ctrl Pts',(0.341625653170807,-0.616053413812982,
-1.31253880423938));
#62955=CARTESIAN_POINT('Ctrl Pts',(0.595557808340173,-0.37903650385649,
-1.29665220574499));
#62956=CARTESIAN_POINT('Ctrl Pts',(0.702804700428006,-0.0479112667122281,
-1.2807656072506));
#62957=CARTESIAN_POINT('Ctrl Pts',(0.622422081552932,0.410937262240509,
-1.25958347592474));
#62958=CARTESIAN_POINT('Ctrl Pts',(0.113906261266067,0.792152092474895,
-1.23310581176742));
#62959=CARTESIAN_POINT('Ctrl Pts',(-0.53775175223377,0.548962917234563,
-1.20435213497569));
#62960=CARTESIAN_POINT('Ctrl Pts',(-0.674638215638227,0.160641167462172,
-1.1861895238469));
#62961=CARTESIAN_POINT('Ctrl Pts',(-0.675858962494509,-0.000507684201011542,
-1.17861797838103));
#62962=CARTESIAN_POINT('Ctrl Pts',(-0.676973562981676,-0.000235536917072003,
-1.33918202161902));
#62963=CARTESIAN_POINT('Ctrl Pts',(-0.677234775375011,-0.058816887218812,
-1.33643064092984));
#62964=CARTESIAN_POINT('Ctrl Pts',(-0.641806312782087,-0.342596601065592,
-1.32308819457774));
#62965=CARTESIAN_POINT('Ctrl Pts',(-0.248041461525952,-0.760890929984079,
-1.29915468256271));
#62966=CARTESIAN_POINT('Ctrl Pts',(0.507461495749466,-0.619609606749274,
-1.26738148557393));
#62967=CARTESIAN_POINT('Ctrl Pts',(0.74527725860231,-0.0286501079923499,
-1.2409038214166));
#62968=CARTESIAN_POINT('Ctrl Pts',(0.576506692556375,0.403574133443626,
-1.21972169009074));
#62969=CARTESIAN_POINT('Ctrl Pts',(0.226209707001196,0.711333684755956,
-1.19853955876488));
#62970=CARTESIAN_POINT('Ctrl Pts',(-0.280199631649522,0.691648133864366,
-1.17735742743902));
#62971=CARTESIAN_POINT('Ctrl Pts',(-0.606835592617558,0.35774356613014,
-1.15617529611317));
#62972=CARTESIAN_POINT('Ctrl Pts',(-0.674911531355438,0.127977621129902,
-1.14521533845032));
#62973=CARTESIAN_POINT('Ctrl Pts',(-0.676885804830273,0.00794442058850271,
-1.13955091361894));
#62974=CARTESIAN_POINT('Ctrl Pts',(-0.676874835700589,0.00012642630365326,
-1.13918202161902));
#62975=CARTESIAN_POINT('Origin',(0.,0.,-12.278617978381));
#62976=CARTESIAN_POINT('',(-0.6767,5.35204042542703E-13,-1.57861797838103));
#62977=CARTESIAN_POINT('',(-0.675366916321589,-0.000162312625430594,-1.53918202161901));
#62978=CARTESIAN_POINT('',(-0.6767,6.12423655037739E-13,-12.278617978381));
#62979=CARTESIAN_POINT('Ctrl Pts',(-0.677053553463528,0.000169628890303121,
-1.57861797838103));
#62980=CARTESIAN_POINT('Ctrl Pts',(-0.675400439898793,-0.195958740493585,
-1.56935791280578));
#62981=CARTESIAN_POINT('Ctrl Pts',(-0.534568406785807,-0.504445956789688,
-1.55480231439907));
#62982=CARTESIAN_POINT('Ctrl Pts',(-0.138419734612189,-0.690702448703422,
-1.5349511831609));
#62983=CARTESIAN_POINT('Ctrl Pts',(0.208558492969346,-0.674433932524933,
-1.5190645846665));
#62984=CARTESIAN_POINT('Ctrl Pts',(0.504655813759805,-0.491479853157888,
-1.50317798617211));
#62985=CARTESIAN_POINT('Ctrl Pts',(0.740425626835783,-0.0897138352053628,
-1.48199585484625));
#62986=CARTESIAN_POINT('Ctrl Pts',(0.599619882655918,0.530033555816679,
-1.45551819068893));
#62987=CARTESIAN_POINT('Ctrl Pts',(-0.123187980897615,0.79136461622102,
-1.42374499370014));
#62988=CARTESIAN_POINT('Ctrl Pts',(-0.611734609152697,0.415005179511451,
-1.39811158959751));
#62989=CARTESIAN_POINT('Ctrl Pts',(-0.676532869522839,0.0952307806240656,
-1.3830692511578));
#62990=CARTESIAN_POINT('Ctrl Pts',(-0.676309172935686,0.000353854140774549,
-1.37861797838103));
#62991=CARTESIAN_POINT('Ctrl Pts',(-0.675366916321589,-0.000162312625430511,
-1.53918202161901));
#62992=CARTESIAN_POINT('Ctrl Pts',(-0.675221364951782,-0.125283662983,-1.53331036824075));
#62993=CARTESIAN_POINT('Ctrl Pts',(-0.582503076894211,-0.476023863715487,
-1.51684764919956));
#62994=CARTESIAN_POINT('Ctrl Pts',(-0.0143232884913037,-0.800767180802928,
-1.48979386449544));
#62995=CARTESIAN_POINT('Ctrl Pts',(0.549496765312817,-0.504293888311659,
-1.46331620033811));
#62996=CARTESIAN_POINT('Ctrl Pts',(0.700662799746577,-0.0656025060371282,
-1.44213406901226));
#62997=CARTESIAN_POINT('Ctrl Pts',(0.632898545584985,0.395734599961226,
-1.4209519376864));
#62998=CARTESIAN_POINT('Ctrl Pts',(0.234174509286621,0.708555766228003,
-1.39976980636054));
#62999=CARTESIAN_POINT('Ctrl Pts',(-0.230938351402798,0.665505351914144,
-1.37858767503468));
#63000=CARTESIAN_POINT('Ctrl Pts',(-0.521748873394984,0.475537472174135,
-1.36270107654029));
#63001=CARTESIAN_POINT('Ctrl Pts',(-0.65605051904258,0.221017565263106,
-1.34956585873506));
#63002=CARTESIAN_POINT('Ctrl Pts',(-0.676732024588713,0.0539335820474626,
-1.34172617376131));
#63003=CARTESIAN_POINT('Ctrl Pts',(-0.676973562981676,-0.000235536917072003,
-1.33918202161902));
#63004=CARTESIAN_POINT('Origin',(0.,0.,-12.278617978381));
#63005=CARTESIAN_POINT('',(-0.6767,4.82147705686052E-13,-1.77861797838102));
#63006=CARTESIAN_POINT('',(-0.677257035716489,0.00088196528073553,-1.73918202161901));
#63007=CARTESIAN_POINT('',(-0.6767,6.12423655037739E-13,-12.278617978381));
#63008=CARTESIAN_POINT('Ctrl Pts',(-0.6767,4.82147705686052E-13,-1.77861797838102));
#63009=CARTESIAN_POINT('Ctrl Pts',(-0.676700000000059,-0.082119756793935,
-1.77475518387258));
#63010=CARTESIAN_POINT('Ctrl Pts',(-0.661576824416428,-0.164280093512661,
-1.7708893545134));
#63011=CARTESIAN_POINT('Ctrl Pts',(-0.632313905337345,-0.241043595884718,
-1.76702504257958));
#63012=CARTESIAN_POINT('Ctrl Pts',(-0.562558735104792,-0.424027773271085,
-1.75781353035667));
#63013=CARTESIAN_POINT('Ctrl Pts',(-0.40938922223103,-0.573299527009233,
-1.74860201813377));
#63014=CARTESIAN_POINT('Ctrl Pts',(-0.224668156292418,-0.638315838396766,
-1.73939050591086));
#63015=CARTESIAN_POINT('Ctrl Pts',(-0.0399470903538051,-0.703332149784298,
-1.73017899368795));
#63016=CARTESIAN_POINT('Ctrl Pts',(0.172951249061904,-0.68290537294406,
-1.72096748146505));
#63017=CARTESIAN_POINT('Ctrl Pts',(0.341940050610126,-0.58395196017202,
-1.71175596924214));
#63018=CARTESIAN_POINT('Ctrl Pts',(0.510928852158348,-0.484998547399981,
-1.70254445701923));
#63019=CARTESIAN_POINT('Ctrl Pts',(0.632921215811054,-0.309326069907138,
-1.69333294479633));
#63020=CARTESIAN_POINT('Ctrl Pts',(0.666610851776377,-0.116416761224374,
-1.68412143257342));
#63021=CARTESIAN_POINT('Ctrl Pts',(0.700300487741701,0.0764925474583901,
-1.67490992035051));
#63022=CARTESIAN_POINT('Ctrl Pts',(0.645071991109655,0.28311483400515,-1.66569840812761));
#63023=CARTESIAN_POINT('Ctrl Pts',(0.519625583913373,0.433488341876326,
-1.6564868959047));
#63024=CARTESIAN_POINT('Ctrl Pts',(0.394179176717091,0.583861849747502,
-1.64727538368179));
#63025=CARTESIAN_POINT('Ctrl Pts',(0.200806374810538,0.67523972245669,-1.63806387145888));
#63026=CARTESIAN_POINT('Ctrl Pts',(0.0049826944822306,0.6766816554006,-1.62885235923598));
#63027=CARTESIAN_POINT('Ctrl Pts',(-0.190840985846077,0.678123588344511,
-1.61964084701307));
#63028=CARTESIAN_POINT('Ctrl Pts',(-0.385538454760861,0.589603241891143,
-1.61042933479017));
#63029=CARTESIAN_POINT('Ctrl Pts',(-0.51318566724868,0.441093369855553,
-1.60121782256726));
#63030=CARTESIAN_POINT('Ctrl Pts',(-0.61757703619451,0.319640276273546,
-1.59368454117185));
#63031=CARTESIAN_POINT('Ctrl Pts',(-0.676699999999874,0.159958743945511,
-1.5861422061894));
#63032=CARTESIAN_POINT('Ctrl Pts',(-0.6767,5.35204119005623E-13,-1.57861797838103));
#63033=CARTESIAN_POINT('Ctrl Pts',(-0.677257035716489,0.000881965280735513,
-1.73918202161901));
#63034=CARTESIAN_POINT('Ctrl Pts',(-0.675585900234077,-0.189916695348646,
-1.73019009555166));
#63035=CARTESIAN_POINT('Ctrl Pts',(-0.491749932536183,-0.609461463096116,
-1.71060710382138));
#63036=CARTESIAN_POINT('Ctrl Pts',(0.0923655176653327,-0.740086232829771,
-1.68572857925962));
#63037=CARTESIAN_POINT('Ctrl Pts',(0.491570810089264,-0.5035773887053,-1.66454644793377));
#63038=CARTESIAN_POINT('Ctrl Pts',(0.738569211247283,-0.10808312915354,
-1.64336431660791));
#63039=CARTESIAN_POINT('Ctrl Pts',(0.637170952451161,0.388461261913037,
-1.62218218528205));
#63040=CARTESIAN_POINT('Ctrl Pts',(0.254797411454479,0.656740568787333,
-1.60100005395619));
#63041=CARTESIAN_POINT('Ctrl Pts',(-0.0898318649340317,0.700205691474415,
-1.5851134554618));
#63042=CARTESIAN_POINT('Ctrl Pts',(-0.412913548481974,0.570729653953337,
-1.56922685696741));
#63043=CARTESIAN_POINT('Ctrl Pts',(-0.630596046941778,0.313852223971835,
-1.55391637901981));
#63044=CARTESIAN_POINT('Ctrl Pts',(-0.675483904992149,0.100405483174212,
-1.54390143390368));
#63045=CARTESIAN_POINT('Ctrl Pts',(-0.675366916321589,-0.000162312625430511,
-1.53918202161901));
#63046=CARTESIAN_POINT('Origin',(0.,0.,-12.278617978381));
#63047=CARTESIAN_POINT('',(-0.6767,4.6755719955438E-13,-1.97861797838102));
#63048=CARTESIAN_POINT('',(-0.677446490839416,-0.000787741955589949,-1.93918202161901));
#63049=CARTESIAN_POINT('',(-0.6767,6.12423655037739E-13,-12.278617978381));
#63050=CARTESIAN_POINT('Ctrl Pts',(-0.676413475060879,-0.000340497908876618,
-1.97861797838102));
#63051=CARTESIAN_POINT('Ctrl Pts',(-0.676278753013238,-0.104907816759115,
-1.97370843309053));
#63052=CARTESIAN_POINT('Ctrl Pts',(-0.626229281881828,-0.321358158604508,
-1.96350335496856));
#63053=CARTESIAN_POINT('Ctrl Pts',(-0.403309811719612,-0.577556172326435,
-1.94800274401514));
#63054=CARTESIAN_POINT('Ctrl Pts',(0.0313217580437868,-0.745182949734803,
-1.92682061268927));
#63055=CARTESIAN_POINT('Ctrl Pts',(0.620103828443481,-0.505915819003228,
-1.90034294853195));
#63056=CARTESIAN_POINT('Ctrl Pts',(0.760987813965571,0.249661333490343,
-1.86856975154317));
#63057=CARTESIAN_POINT('Ctrl Pts',(0.295673986471208,0.684715937160779,
-1.84209208738584));
#63058=CARTESIAN_POINT('Ctrl Pts',(-0.168329559292972,0.683298768632944,
-1.82090995605999));
#63059=CARTESIAN_POINT('Ctrl Pts',(-0.546841497105642,0.485885352754348,
-1.80151709733553));
#63060=CARTESIAN_POINT('Ctrl Pts',(-0.674917444468637,0.186609400672984,
-1.78741977144254));
#63061=CARTESIAN_POINT('Ctrl Pts',(-0.676717196229297,-0.000122736083201944,
-1.77861797838102));
#63062=CARTESIAN_POINT('Ctrl Pts',(-0.677446490839416,-0.000787741955589942,
-1.93918202161901));
#63063=CARTESIAN_POINT('Ctrl Pts',(-0.677732392339807,-0.0330590201563695,
-1.9376608885255));
#63064=CARTESIAN_POINT('Ctrl Pts',(-0.661044596458893,-0.289636215322383,
-1.92554868976905));
#63065=CARTESIAN_POINT('Ctrl Pts',(-0.408696466689488,-0.62387997162377,
-1.90814095818113));
#63066=CARTESIAN_POINT('Ctrl Pts',(0.0486787143220458,-0.702041615945249,
-1.88695882685528));
#63067=CARTESIAN_POINT('Ctrl Pts',(0.492962794513711,-0.560494536846958,
-1.86577669552942));
#63068=CARTESIAN_POINT('Ctrl Pts',(0.737117187516088,-0.116392553554602,
-1.84459456420356));
#63069=CARTESIAN_POINT('Ctrl Pts',(0.619346845481977,0.335617908590315,
-1.8234124328777));
#63070=CARTESIAN_POINT('Ctrl Pts',(0.384810828458858,0.591843223017294,
-1.80752583438331));
#63071=CARTESIAN_POINT('Ctrl Pts',(0.0547443097277555,0.702305486931504,
-1.79163923588892));
#63072=CARTESIAN_POINT('Ctrl Pts',(-0.404864299349843,0.626389320003439,
-1.77045710456306));
#63073=CARTESIAN_POINT('Ctrl Pts',(-0.659871184498933,0.293031979129122,
-1.75297136647309));
#63074=CARTESIAN_POINT('Ctrl Pts',(-0.677554233324596,0.0348139272107488,
-1.74078116121459));
#63075=CARTESIAN_POINT('Ctrl Pts',(-0.677257035716489,0.000881965280735513,
-1.73918202161901));
#63076=CARTESIAN_POINT('Origin',(0.,0.,-12.278617978381));
#63077=CARTESIAN_POINT('',(-0.6767,4.52966762133127E-13,-2.17861797838102));
#63078=CARTESIAN_POINT('',(-0.675328212337249,-8.63283092417122E-5,-2.13918202161901));
#63079=CARTESIAN_POINT('',(-0.6767,6.12423655037739E-13,-12.278617978381));
#63080=CARTESIAN_POINT('Ctrl Pts',(-0.6767,4.91432703676236E-13,-2.17861797838103));
#63081=CARTESIAN_POINT('Ctrl Pts',(-0.676700000000127,-0.17490534537463,
-2.17039068407346));
#63082=CARTESIAN_POINT('Ctrl Pts',(-0.605526598979385,-0.349171323828889,
-2.16214503008812));
#63083=CARTESIAN_POINT('Ctrl Pts',(-0.482847266157599,-0.47411117637547,
-2.15390855594167));
#63084=CARTESIAN_POINT('Ctrl Pts',(-0.345645090360969,-0.613841473393005,
-2.14469704371876));
#63085=CARTESIAN_POINT('Ctrl Pts',(-0.145512713664304,-0.689273482088197,
-2.13548553149585));
#63086=CARTESIAN_POINT('Ctrl Pts',(0.049785573602703,-0.674866124991505,
-2.12627401927295));
#63087=CARTESIAN_POINT('Ctrl Pts',(0.24508386086971,-0.660458767894813,
-2.11706250705004));
#63088=CARTESIAN_POINT('Ctrl Pts',(0.431980566169593,-0.556475222628767,
-2.10785099482713));
#63089=CARTESIAN_POINT('Ctrl Pts',(0.547192962296249,-0.398124040989057,
-2.09863948260423));
#63090=CARTESIAN_POINT('Ctrl Pts',(0.662405358422905,-0.239772859349346,
-2.08942797038132));
#63091=CARTESIAN_POINT('Ctrl Pts',(0.70382887308767,-0.0299466251200073,
-2.08021645815841));
#63092=CARTESIAN_POINT('Ctrl Pts',(0.657437614425613,0.160308056997643,
-2.07100494593551));
#63093=CARTESIAN_POINT('Ctrl Pts',(0.611046355763555,0.350562739115292,
-2.0617934337126));
#63094=CARTESIAN_POINT('Ctrl Pts',(0.477687747842733,0.517770507569595,
-2.05258192148969));
#63095=CARTESIAN_POINT('Ctrl Pts',(0.302516660526142,0.60531525679113,-2.04337040926679));
#63096=CARTESIAN_POINT('Ctrl Pts',(0.127345573209552,0.692860006012664,
-2.03415889704388));
#63097=CARTESIAN_POINT('Ctrl Pts',(-0.0864381623341533,0.699142565604636,
-2.02494738482097));
#63098=CARTESIAN_POINT('Ctrl Pts',(-0.266447941986903,0.622035677602937,
-2.01573587259807));
#63099=CARTESIAN_POINT('Ctrl Pts',(-0.446457721639652,0.544928789601237,
-2.00652436037516));
#63100=CARTESIAN_POINT('Ctrl Pts',(-0.589405326367021,0.385840957128872,
-1.99731284815225));
#63101=CARTESIAN_POINT('Ctrl Pts',(-0.646889077497289,0.198638897033553,
-1.98810133592935));
#63102=CARTESIAN_POINT('Ctrl Pts',(-0.666615804662001,0.134396673943352,
-1.98494021674657));
#63103=CARTESIAN_POINT('Ctrl Pts',(-0.676699999999954,0.0671595727141406,
-1.98177706748205));
#63104=CARTESIAN_POINT('Ctrl Pts',(-0.6767,4.6755723390959E-13,-1.97861797838102));
#63105=CARTESIAN_POINT('Ctrl Pts',(-0.675328212337249,-8.63283092416567E-5,
-2.13918202161901));
#63106=CARTESIAN_POINT('Ctrl Pts',(-0.675444524571566,-0.0990680295131166,
-2.1345406158364));
#63107=CARTESIAN_POINT('Ctrl Pts',(-0.63166980646997,-0.310842263830983,
-2.12460367722233));
#63108=CARTESIAN_POINT('Ctrl Pts',(-0.417365872073619,-0.566601956028473,
-2.10937120577679));
#63109=CARTESIAN_POINT('Ctrl Pts',(0.0128942183109048,-0.74632444804134,
-2.08818907445093));
#63110=CARTESIAN_POINT('Ctrl Pts',(0.486476949341432,-0.565887932734067,
-2.06700694312507));
#63111=CARTESIAN_POINT('Ctrl Pts',(0.689323544065248,-0.145130793329111,
-2.04582481179921));
#63112=CARTESIAN_POINT('Ctrl Pts',(0.676430423898524,0.201989247127572,
-2.02993821330482));
#63113=CARTESIAN_POINT('Ctrl Pts',(0.496364768725477,0.499851930865303,
-2.01405161481042));
#63114=CARTESIAN_POINT('Ctrl Pts',(0.0969107931718748,0.739518072307371,
-1.99286948348457));
#63115=CARTESIAN_POINT('Ctrl Pts',(-0.488495455026634,0.612489083801584,
-1.96791295242076));
#63116=CARTESIAN_POINT('Ctrl Pts',(-0.675741769969761,0.19163349880046,
-1.94825195418842));
#63117=CARTESIAN_POINT('Ctrl Pts',(-0.677446490839416,-0.000787741955589942,
-1.93918202161901));
#63118=CARTESIAN_POINT('Origin',(0.,0.,-12.278617978381));
#63119=CARTESIAN_POINT('',(-0.677485359766029,-0.000107376913780513,-2.37861797838102));
#63120=CARTESIAN_POINT('',(-0.676795338809115,0.000510576453991912,-2.33918202161901));
#63121=CARTESIAN_POINT('',(-0.6767,6.12423655037739E-13,-12.278617978381));
#63122=CARTESIAN_POINT('Ctrl Pts',(-0.677485359766029,-0.000107376913780525,
-2.37861797838102));
#63123=CARTESIAN_POINT('Ctrl Pts',(-0.677488765774498,-0.0119719264639521,
-2.37805895337527));
#63124=CARTESIAN_POINT('Ctrl Pts',(-0.670999253114086,-0.248539305774364,
-2.36690886270659));
#63125=CARTESIAN_POINT('Ctrl Pts',(-0.398867864803067,-0.693818420334465,
-2.34516770637498));
#63126=CARTESIAN_POINT('Ctrl Pts',(0.369549690352763,-0.710539415377113,
-2.31339450938619));
#63127=CARTESIAN_POINT('Ctrl Pts',(0.723546655452461,-0.180939929980367,
-2.28691684522887));
#63128=CARTESIAN_POINT('Ctrl Pts',(0.647040070382234,0.276715006941831,
-2.26573471390301));
#63129=CARTESIAN_POINT('Ctrl Pts',(0.36733345238644,0.649794257721565,-2.24455258257715));
#63130=CARTESIAN_POINT('Ctrl Pts',(-0.132342674989519,0.734421126487522,
-2.22337045125129));
#63131=CARTESIAN_POINT('Ctrl Pts',(-0.520533786771069,0.474630880163505,
-2.20218831992543));
#63132=CARTESIAN_POINT('Ctrl Pts',(-0.657056894194546,0.221529119030303,
-2.18903600657917));
#63133=CARTESIAN_POINT('Ctrl Pts',(-0.676586384573887,0.0548096435792028,
-2.18117922606436));
#63134=CARTESIAN_POINT('Ctrl Pts',(-0.676477391207069,0.000385350982612692,
-2.17861797838103));
#63135=CARTESIAN_POINT('Ctrl Pts',(-0.676795338809115,0.000510576453991895,
-2.33918202161901));
#63136=CARTESIAN_POINT('Ctrl Pts',(-0.676521639134244,-0.0519039108123045,
-2.33671587597878));
#63137=CARTESIAN_POINT('Ctrl Pts',(-0.656639741323987,-0.217177799902405,
-2.32895419750708));
#63138=CARTESIAN_POINT('Ctrl Pts',(-0.473307084952599,-0.57718874377774,
-2.31060145337244));
#63139=CARTESIAN_POINT('Ctrl Pts',(0.0044593387890197,-0.746236617268379,
-2.28941932204658));
#63140=CARTESIAN_POINT('Ctrl Pts',(0.431445304074627,-0.5568526242795,-2.26823719072073));
#63141=CARTESIAN_POINT('Ctrl Pts',(0.646327285527458,-0.283934524694336,
-2.25235059222633));
#63142=CARTESIAN_POINT('Ctrl Pts',(0.701905026833796,0.0596596155461771,
-2.23646399373194));
#63143=CARTESIAN_POINT('Ctrl Pts',(0.552593332470904,0.500918446467205,
-2.21528186240608));
#63144=CARTESIAN_POINT('Ctrl Pts',(-0.00803857589287147,0.800259305016558,
-2.18880419824876));
#63145=CARTESIAN_POINT('Ctrl Pts',(-0.580828746386521,0.479835670177724,
-2.16167240704258));
#63146=CARTESIAN_POINT('Ctrl Pts',(-0.675179115648332,0.126794940884012,
-2.14513168149933));
#63147=CARTESIAN_POINT('Ctrl Pts',(-0.675328212337249,-8.63283092416567E-5,
-2.13918202161901));
#63148=CARTESIAN_POINT('Origin',(0.,0.,-12.278617978381));
#63149=CARTESIAN_POINT('',(-0.67667083393025,-2.5222838540107E-5,-2.57861797838102));
#63150=CARTESIAN_POINT('',(-0.677533761904701,-0.000330077543184093,-2.53918202161901));
#63151=CARTESIAN_POINT('',(-0.6767,6.12423655037739E-13,-12.278617978381));
#63152=CARTESIAN_POINT('Ctrl Pts',(-0.675978983105548,-0.000623535949907557,
-2.57861797838102));
#63153=CARTESIAN_POINT('Ctrl Pts',(-0.67660824076582,-0.0788507797028598,
-2.57493868068618));
#63154=CARTESIAN_POINT('Ctrl Pts',(-0.628107327354101,-0.381596062206871,
-2.56066831732841));
#63155=CARTESIAN_POINT('Ctrl Pts',(-0.178302031962507,-0.780795504496738,
-2.53580688830771));
#63156=CARTESIAN_POINT('Ctrl Pts',(0.434348713906479,-0.606300433453199,
-2.50932922415038));
#63157=CARTESIAN_POINT('Ctrl Pts',(0.672300129659377,-0.207953320259739,
-2.48814709282452));
#63158=CARTESIAN_POINT('Ctrl Pts',(0.70062407108951,0.257473015323963,-2.46696496149866));
#63159=CARTESIAN_POINT('Ctrl Pts',(0.374558924196536,0.645441389251823,
-2.44578283017281));
#63160=CARTESIAN_POINT('Ctrl Pts',(-0.0894926216029255,0.698728106099681,
-2.42460069884695));
#63161=CARTESIAN_POINT('Ctrl Pts',(-0.413090643562724,0.572463007129391,
-2.40871410035255));
#63162=CARTESIAN_POINT('Ctrl Pts',(-0.627406575776416,0.313931316160718,
-2.39338652686391));
#63163=CARTESIAN_POINT('Ctrl Pts',(-0.677456501332862,0.100418594580537,
-2.38335448620674));
#63164=CARTESIAN_POINT('Ctrl Pts',(-0.677485359766029,-0.000107376913780525,
-2.37861797838102));
#63165=CARTESIAN_POINT('Ctrl Pts',(-0.6775337619047,-0.000330077543184071,
-2.53918202161901));
#63166=CARTESIAN_POINT('Ctrl Pts',(-0.677535144161109,-0.00649456504868987,
-2.53889113612115));
#63167=CARTESIAN_POINT('Ctrl Pts',(-0.674213842716546,-0.23704730980286,
-2.52800918496036));
#63168=CARTESIAN_POINT('Ctrl Pts',(-0.47967921519751,-0.571661460273545,
-2.51183170096809));
#63169=CARTESIAN_POINT('Ctrl Pts',(-0.0316362470218281,-0.703725119240024,
-2.49064956964224));
#63170=CARTESIAN_POINT('Ctrl Pts',(0.308819018868513,-0.634813821459323,
-2.47476297114784));
#63171=CARTESIAN_POINT('Ctrl Pts',(0.573606362075548,-0.408907908713105,
-2.45887637265346));
#63172=CARTESIAN_POINT('Ctrl Pts',(0.745452333195922,0.0240728069648603,
-2.43769424132759));
#63173=CARTESIAN_POINT('Ctrl Pts',(0.511922871354516,0.615154084561029,
-2.41121657717027));
#63174=CARTESIAN_POINT('Ctrl Pts',(-0.242248341456588,0.763379967975192,
-2.37944338018148));
#63175=CARTESIAN_POINT('Ctrl Pts',(-0.640867055936252,0.345262845662194,
-2.3554318616644));
#63176=CARTESIAN_POINT('Ctrl Pts',(-0.677109352037566,0.0606452564527683,
-2.34201140881024));
#63177=CARTESIAN_POINT('Ctrl Pts',(-0.676795338809115,0.000510576453991895,
-2.33918202161901));
#63178=CARTESIAN_POINT('Origin',(0.,0.,-12.278617978381));
#63179=CARTESIAN_POINT('',(-0.676628694961864,5.74670372185009E-5,-2.77861797838102));
#63180=CARTESIAN_POINT('',(-0.6767,4.20837301638721E-13,-2.73918202161901));
#63181=CARTESIAN_POINT('',(-0.6767,6.12423655037739E-13,-12.278617978381));
#63182=CARTESIAN_POINT('Ctrl Pts',(-0.6767,4.0919534680374E-13,-2.77861797838102));
#63183=CARTESIAN_POINT('Ctrl Pts',(-0.676700000000072,-0.118639299394314,
-2.77303735744305));
#63184=CARTESIAN_POINT('Ctrl Pts',(-0.644770474758931,-0.237238798212155,
-2.76745156789602));
#63185=CARTESIAN_POINT('Ctrl Pts',(-0.585155688320175,-0.339876022141225,
-2.76186836265352));
#63186=CARTESIAN_POINT('Ctrl Pts',(-0.4867995810135,-0.509213168401033,
-2.75265685043061));
#63187=CARTESIAN_POINT('Ctrl Pts',(-0.311558945829397,-0.631825059824009,
-2.74344533820771));
#63188=CARTESIAN_POINT('Ctrl Pts',(-0.118769795641856,-0.666195636163426,
-2.7342338259848));
#63189=CARTESIAN_POINT('Ctrl Pts',(0.0740193545456853,-0.700566212502843,
-2.72502231376189));
#63190=CARTESIAN_POINT('Ctrl Pts',(0.280835361332882,-0.646067630185082,
-2.71581080153898));
#63191=CARTESIAN_POINT('Ctrl Pts',(0.431650875022103,-0.52115296419828,
-2.70659928931608));
#63192=CARTESIAN_POINT('Ctrl Pts',(0.582466388711323,-0.396238298211477,
-2.69738777709317));
#63193=CARTESIAN_POINT('Ctrl Pts',(0.67452647874404,-0.203189351150853,
-2.68817626487027));
#63194=CARTESIAN_POINT('Ctrl Pts',(0.676659843546144,-0.0073719829156555,
-2.67896475264736));
#63195=CARTESIAN_POINT('Ctrl Pts',(0.678793208348247,0.188445385319542,
-2.66975324042445));
#63196=CARTESIAN_POINT('Ctrl Pts',(0.590960877977311,0.383454200196352,
-2.66054172820154));
#63197=CARTESIAN_POINT('Ctrl Pts',(0.442902645833232,0.511624995786878,
-2.65133021597864));
#63198=CARTESIAN_POINT('Ctrl Pts',(0.294844413689154,0.639795791377403,
-2.64211870375573));
#63199=CARTESIAN_POINT('Ctrl Pts',(0.0892648433688601,0.698787285721679,
-2.63290719153282));
#63200=CARTESIAN_POINT('Ctrl Pts',(-0.104227369528373,0.668625115772057,
-2.62369567930992));
#63201=CARTESIAN_POINT('Ctrl Pts',(-0.297719582425605,0.638462945822435,
-2.61448416708701));
#63202=CARTESIAN_POINT('Ctrl Pts',(-0.475589936726069,0.51969808065148,
-2.6052726548641));
#63203=CARTESIAN_POINT('Ctrl Pts',(-0.577612003658916,0.352543987651375,
-2.5960611426412));
#63204=CARTESIAN_POINT('Ctrl Pts',(-0.642009235753148,0.247034843933341,
-2.59024675455447));
#63205=CARTESIAN_POINT('Ctrl Pts',(-0.676699999999923,0.123541506275678,
-2.58442919203574));
#63206=CARTESIAN_POINT('Ctrl Pts',(-0.6767,4.23785818580202E-13,-2.57861797838102));
#63207=CARTESIAN_POINT('Ctrl Pts',(-0.675745563573596,-0.000158715524651409,
-2.73918202161901));
#63208=CARTESIAN_POINT('Ctrl Pts',(-0.676298042296179,-0.072673869664635,
-2.73577086343205));
#63209=CARTESIAN_POINT('Ctrl Pts',(-0.648898766616171,-0.257625310384307,
-2.72706417241364));
#63210=CARTESIAN_POINT('Ctrl Pts',(-0.479671017962049,-0.51589302195539,
-2.71306194856376));
#63211=CARTESIAN_POINT('Ctrl Pts',(-0.17556924533772,-0.683764004918535,
-2.69717535006935));
#63212=CARTESIAN_POINT('Ctrl Pts',(0.172489975910581,-0.682991321051767,
-2.68128875157497));
#63213=CARTESIAN_POINT('Ctrl Pts',(0.583760512301853,-0.464222301682604,
-2.6601066202491));
#63214=CARTESIAN_POINT('Ctrl Pts',(0.78840439834167,0.137470282764965,-2.63362895609179));
#63215=CARTESIAN_POINT('Ctrl Pts',(0.309536410753203,0.738661251767208,
-2.601855759103));
#63216=CARTESIAN_POINT('Ctrl Pts',(-0.323960533014889,0.671795053514425,
-2.57537809494567));
#63217=CARTESIAN_POINT('Ctrl Pts',(-0.622531331628934,0.324975084275381,
-2.55448684911768));
#63218=CARTESIAN_POINT('Ctrl Pts',(-0.677509980362131,0.105729131953435,
-2.54418666895261));
#63219=CARTESIAN_POINT('Ctrl Pts',(-0.6775337619047,-0.000330077543184071,
-2.53918202161901));
#63220=CARTESIAN_POINT('Origin',(0.,0.,-12.278617978381));
#63221=CARTESIAN_POINT('',(-0.677908152078298,4.26345795243129E-5,-2.97861797838102));
#63222=CARTESIAN_POINT('',(-0.6767,4.06246809000637E-13,-2.93918202161901));
#63223=CARTESIAN_POINT('',(-0.6767,6.12423655037739E-13,-12.278617978381));
#63224=CARTESIAN_POINT('Ctrl Pts',(-0.677908152078298,4.26345795242825E-5,
-2.97861797838102));
#63225=CARTESIAN_POINT('Ctrl Pts',(-0.676769184190078,-0.209797877091866,
-2.96869813530799));
#63226=CARTESIAN_POINT('Ctrl Pts',(-0.514319791207873,-0.532159781908597,
-2.95348275940349));
#63227=CARTESIAN_POINT('Ctrl Pts',(-0.0963858541361063,-0.697095269579071,
-2.93297185066755));
#63228=CARTESIAN_POINT('Ctrl Pts',(0.367487293040394,-0.649707266439206,
-2.91178971934168));
#63229=CARTESIAN_POINT('Ctrl Pts',(0.697559134358486,-0.265141903002185,
-2.89060758801583));
#63230=CARTESIAN_POINT('Ctrl Pts',(0.675027237917631,0.201415301415524,
-2.86942545668997));
#63231=CARTESIAN_POINT('Ctrl Pts',(0.498046596364184,0.500307267767271,
-2.85353885819557));
#63232=CARTESIAN_POINT('Ctrl Pts',(0.197663098653,0.676135515893496,-2.83765225970118));
#63233=CARTESIAN_POINT('Ctrl Pts',(-0.267743933191193,0.696126330016126,
-2.81647012837532));
#63234=CARTESIAN_POINT('Ctrl Pts',(-0.625584717941753,0.387828683972334,
-2.79679203460194));
#63235=CARTESIAN_POINT('Ctrl Pts',(-0.676382811519772,0.0816008323186632,
-2.78240947366002));
#63236=CARTESIAN_POINT('Ctrl Pts',(-0.675875234839626,0.000664704922657085,
-2.77861797838102));
#63237=CARTESIAN_POINT('Ctrl Pts',(-0.6767,4.44712750543746E-13,-2.93918202161901));
#63238=CARTESIAN_POINT('Ctrl Pts',(-0.676700000000054,-0.0815064203030644,
-2.93534807757142));
#63239=CARTESIAN_POINT('Ctrl Pts',(-0.66180401409219,-0.163055071082539,
-2.9315110623169));
#63240=CARTESIAN_POINT('Ctrl Pts',(-0.63296657669995,-0.239324471754867,
-2.92767558266584));
#63241=CARTESIAN_POINT('Ctrl Pts',(-0.563708900689919,-0.422497524526358,
-2.91846407044293));
#63242=CARTESIAN_POINT('Ctrl Pts',(-0.410945580703484,-0.572184946191539,
-2.90925255822003));
#63243=CARTESIAN_POINT('Ctrl Pts',(-0.226401870485963,-0.637702973993737,
-2.90004104599712));
#63244=CARTESIAN_POINT('Ctrl Pts',(-0.0418581602684427,-0.703221001795936,
-2.89082953377421));
#63245=CARTESIAN_POINT('Ctrl Pts',(0.171094900330045,-0.683372825058906,
-2.88161802155131));
#63246=CARTESIAN_POINT('Ctrl Pts',(0.340351971518003,-0.584878983622944,
-2.8724065093284));
#63247=CARTESIAN_POINT('Ctrl Pts',(0.509609042705961,-0.486385142186983,
-2.86319499710549));
#63248=CARTESIAN_POINT('Ctrl Pts',(0.632078324003079,-0.311044812323557,
-2.85398348488259));
#63249=CARTESIAN_POINT('Ctrl Pts',(0.666292042571853,-0.118227763259854,
-2.84477197265968));
#63250=CARTESIAN_POINT('Ctrl Pts',(0.700505761140627,0.0745892858038498,
-2.83556046043677));
#63251=CARTESIAN_POINT('Ctrl Pts',(0.645838938711248,0.281360886038317,
-2.82634894821387));
#63252=CARTESIAN_POINT('Ctrl Pts',(0.52080161592607,0.432074723686534,-2.81713743599096));
#63253=CARTESIAN_POINT('Ctrl Pts',(0.395764293140892,0.582788561334751,
-2.80792592376805));
#63254=CARTESIAN_POINT('Ctrl Pts',(0.202640513153508,0.674691563143353,
-2.79871441154515));
#63255=CARTESIAN_POINT('Ctrl Pts',(0.0068214740930863,0.67666561719301,
-2.78950289932224));
#63256=CARTESIAN_POINT('Ctrl Pts',(-0.188997564967335,0.678639671242668,
-2.78029138709933));
#63257=CARTESIAN_POINT('Ctrl Pts',(-0.383934858047051,0.590648717703111,
-2.77107987487643));
#63258=CARTESIAN_POINT('Ctrl Pts',(-0.511985156308387,0.442486259357142,
-2.76186836265352));
#63259=CARTESIAN_POINT('Ctrl Pts',(-0.617106974370762,0.320853532206972,
-2.75430624897535));
#63260=CARTESIAN_POINT('Ctrl Pts',(-0.6766999999999,0.160570324119808,-2.74673501727365));
#63261=CARTESIAN_POINT('Ctrl Pts',(-0.6767,4.20837280777099E-13,-2.73918202161901));
#63262=CARTESIAN_POINT('Origin',(0.,0.,-12.278617978381));
#63263=CARTESIAN_POINT('',(-0.676187862115932,-0.000564937425030058,-3.17861797838102));
#63264=CARTESIAN_POINT('',(-0.67679285177372,0.000237387877347908,-3.13918202161901));
#63265=CARTESIAN_POINT('',(-0.6767,6.12423655037739E-13,-12.278617978381));
#63266=CARTESIAN_POINT('Ctrl Pts',(-0.676187862115932,-0.000564937425030061,
-3.17861797838102));
#63267=CARTESIAN_POINT('Ctrl Pts',(-0.676644491535547,-0.0526279803465272,
-3.17616892828183));
#63268=CARTESIAN_POINT('Ctrl Pts',(-0.659369213156443,-0.216993979854592,
-3.16842434535117));
#63269=CARTESIAN_POINT('Ctrl Pts',(-0.524730724624935,-0.468923996380709,
-3.15538422958906));
#63270=CARTESIAN_POINT('Ctrl Pts',(-0.140494133246507,-0.733094701340396,
-3.1342020982632));
#63271=CARTESIAN_POINT('Ctrl Pts',(0.360032912737676,-0.653655319262541,
-3.11301996693734));
#63272=CARTESIAN_POINT('Ctrl Pts',(0.644886244911881,-0.283463625000574,
-3.09183783561148));
#63273=CARTESIAN_POINT('Ctrl Pts',(0.703481663861427,0.0589179339543426,
-3.07595123711709));
#63274=CARTESIAN_POINT('Ctrl Pts',(0.588354962968238,0.38738659498273,-3.06006463862269));
#63275=CARTESIAN_POINT('Ctrl Pts',(0.246567099391958,0.703905779632369,
-3.03888250729684));
#63276=CARTESIAN_POINT('Ctrl Pts',(-0.388958651052195,0.699421719522368,
-3.01240484313951));
#63277=CARTESIAN_POINT('Ctrl Pts',(-0.671229579838026,0.252454363145372,
-2.99055148922376));
#63278=CARTESIAN_POINT('Ctrl Pts',(-0.677985219928073,0.0142414168257241,
-2.97928920097093));
#63279=CARTESIAN_POINT('Ctrl Pts',(-0.677908152078298,4.26345795242825E-5,
-2.97861797838102));
#63280=CARTESIAN_POINT('Ctrl Pts',(-0.67679285177372,0.000237387877347905,
-3.13918202161901));
#63281=CARTESIAN_POINT('Ctrl Pts',(-0.676567324318828,-0.0921345146587963,
-3.13482585088534));
#63282=CARTESIAN_POINT('Ctrl Pts',(-0.633537174009138,-0.297198424375294,
-3.1251741473202));
#63283=CARTESIAN_POINT('Ctrl Pts',(-0.363607076602154,-0.651205478284122,
-3.10493137809214));
#63284=CARTESIAN_POINT('Ctrl Pts',(0.263276112884758,-0.755754763367232,
-3.0784537139348));
#63285=CARTESIAN_POINT('Ctrl Pts',(0.779024453182575,-0.18588742772943,
-3.04668051694603));
#63286=CARTESIAN_POINT('Ctrl Pts',(0.610496128531625,0.428431439002367,
-3.0202028527887));
#63287=CARTESIAN_POINT('Ctrl Pts',(0.214482113777081,0.670245828496365,
-2.99902072146284));
#63288=CARTESIAN_POINT('Ctrl Pts',(-0.250646737033531,0.703095054615309,
-2.97783859013698));
#63289=CARTESIAN_POINT('Ctrl Pts',(-0.618947531810959,0.399622239638097,
-2.9578923568557));
#63290=CARTESIAN_POINT('Ctrl Pts',(-0.676858577889835,0.0866323387819684,
-2.94324165640589));
#63291=CARTESIAN_POINT('Ctrl Pts',(-0.676596105090679,3.86521990314997E-6,
-2.93918202161901));
#63292=CARTESIAN_POINT('Origin',(0.,0.,-12.278617978381));
#63293=CARTESIAN_POINT('',(-0.6767,3.65423945443422E-13,-3.37861797838102));
#63294=CARTESIAN_POINT('',(-0.677150171393189,-0.000258134096645546,-3.33918202161901));
#63295=CARTESIAN_POINT('',(-0.6767,6.12423655037739E-13,-12.278617978381));
#63296=CARTESIAN_POINT('Ctrl Pts',(-0.67623262201224,0.000222076779409647,
-3.37861797838102));
#63297=CARTESIAN_POINT('Ctrl Pts',(-0.676226890528276,-0.00561783417541074,
-3.3783441884242));
#63298=CARTESIAN_POINT('Ctrl Pts',(-0.674616485481495,-0.124427520960238,
-3.37277486563592));
#63299=CARTESIAN_POINT('Ctrl Pts',(-0.581653969262653,-0.467808831309393,
-3.35661447718471));
#63300=CARTESIAN_POINT('Ctrl Pts',(-0.148731575015875,-0.731278259794368,
-3.33543234585885));
#63301=CARTESIAN_POINT('Ctrl Pts',(0.308025509003036,-0.633522044903279,
-3.314250214533));
#63302=CARTESIAN_POINT('Ctrl Pts',(0.5743279309632,-0.410493851410992,-3.2983636160386));
#63303=CARTESIAN_POINT('Ctrl Pts',(0.699214400400128,-0.0856105057499347,
-3.2824770175442));
#63304=CARTESIAN_POINT('Ctrl Pts',(0.643606290730907,0.376894711602609,
-3.26129488621835));
#63305=CARTESIAN_POINT('Ctrl Pts',(0.156311633013567,0.784886136552685,
-3.23481722206102));
#63306=CARTESIAN_POINT('Ctrl Pts',(-0.520643055030093,0.572945154878293,
-3.20549307517143));
#63307=CARTESIAN_POINT('Ctrl Pts',(-0.674669769920679,0.172521805840283,
-3.18675999394476));
#63308=CARTESIAN_POINT('Ctrl Pts',(-0.676187862115932,-0.000564937425030061,
-3.17861797838102));
#63309=CARTESIAN_POINT('Ctrl Pts',(-0.677150171393189,-0.000258134096645515,
-3.33918202161901));
#63310=CARTESIAN_POINT('Ctrl Pts',(-0.677354841532161,-0.0466576125141528,
-3.33700111102771));
#63311=CARTESIAN_POINT('Ctrl Pts',(-0.650453642473587,-0.318071380082664,
-3.32422913477348));
#63312=CARTESIAN_POINT('Ctrl Pts',(-0.28857304180409,-0.746461769625146,
-3.30086609285632));
#63313=CARTESIAN_POINT('Ctrl Pts',(0.473430607192205,-0.645985057580972,
-3.26909289586753));
#63314=CARTESIAN_POINT('Ctrl Pts',(0.742660672680755,-0.0686596397537776,
-3.24261523171021));
#63315=CARTESIAN_POINT('Ctrl Pts',(0.597361558428951,0.372009699145598,
-3.22143310038435));
#63316=CARTESIAN_POINT('Ctrl Pts',(0.264109646042611,0.698149366165507,
-3.2002509690585));
#63317=CARTESIAN_POINT('Ctrl Pts',(-0.242625816165684,0.705706516892486,
-3.17906883773263));
#63318=CARTESIAN_POINT('Ctrl Pts',(-0.586733693445035,0.38983774644249,
-3.15788670640678));
#63319=CARTESIAN_POINT('Ctrl Pts',(-0.671239753740077,0.152310487815706,
-3.14635627864606));
#63320=CARTESIAN_POINT('Ctrl Pts',(-0.676841484381597,0.0201564106724313,
-3.1401213837168));
#63321=CARTESIAN_POINT('Ctrl Pts',(-0.67679285177372,0.000237387877347905,
-3.13918202161901));
#63322=CARTESIAN_POINT('Origin',(0.,0.,-12.278617978381));
#63323=CARTESIAN_POINT('',(-0.6767,3.5083345969789E-13,-3.57861797838102));
#63324=CARTESIAN_POINT('',(-0.6765227315498,-4.29419654870256E-5,-3.53918202161901));
#63325=CARTESIAN_POINT('',(-0.6767,6.12423655037739E-13,-12.278617978381));
#63326=CARTESIAN_POINT('Ctrl Pts',(-0.6767,3.5083345969789E-13,-3.57861797838102));
#63327=CARTESIAN_POINT('Ctrl Pts',(-0.676700000000056,-0.10872516508436,
-3.57350370397235));
#63328=CARTESIAN_POINT('Ctrl Pts',(-0.649982596219497,-0.217427540192554,
-3.56838594349128));
#63329=CARTESIAN_POINT('Ctrl Pts',(-0.599548926342118,-0.313789698559424,
-3.56326992604641));
#63330=CARTESIAN_POINT('Ctrl Pts',(-0.508741893033908,-0.487292077937056,
-3.55405841382351));
#63331=CARTESIAN_POINT('Ctrl Pts',(-0.339068136092228,-0.617498730391311,
-3.5448469016006));
#63332=CARTESIAN_POINT('Ctrl Pts',(-0.147978738227961,-0.660322029794903,
-3.53563538937769));
#63333=CARTESIAN_POINT('Ctrl Pts',(0.0431106596363064,-0.703145329198496,
-3.52642387715479));
#63334=CARTESIAN_POINT('Ctrl Pts',(0.252125089209894,-0.657803027006444,
-3.51721236493188));
#63335=CARTESIAN_POINT('Ctrl Pts',(0.408292820688247,-0.539647906115122,
-3.50800085270897));
#63336=CARTESIAN_POINT('Ctrl Pts',(0.564460552166599,-0.421492785223799,
-3.49878934048607));
#63337=CARTESIAN_POINT('Ctrl Pts',(0.664928886611912,-0.232683172354559,
-3.48957782826316));
#63338=CARTESIAN_POINT('Ctrl Pts',(0.675679513260744,-0.0371495001275096,
-3.48036631604025));
#63339=CARTESIAN_POINT('Ctrl Pts',(0.686430139909577,0.15838417209954,-3.47115480381734));
#63340=CARTESIAN_POINT('Ctrl Pts',(0.607266678236122,0.357070111395513,
-3.46194329159444));
#63341=CARTESIAN_POINT('Ctrl Pts',(0.464993665761435,0.491633787286577,
-3.45273177937153));
#63342=CARTESIAN_POINT('Ctrl Pts',(0.322720653286747,0.626197463177641,
-3.44352026714862));
#63343=CARTESIAN_POINT('Ctrl Pts',(0.119936975630301,0.694180815655831,
-3.43430875492572));
#63344=CARTESIAN_POINT('Ctrl Pts',(-0.0746953534265867,0.672564862430738,
-3.42509724270281));
#63345=CARTESIAN_POINT('Ctrl Pts',(-0.269327682483474,0.650948909205645,
-3.4158857304799));
#63346=CARTESIAN_POINT('Ctrl Pts',(-0.452253335389412,0.540128506539963,
-3.406674218257));
#63347=CARTESIAN_POINT('Ctrl Pts',(-0.561534172714542,0.377627147956546,
-3.39746270603409));
#63348=CARTESIAN_POINT('Ctrl Pts',(-0.6360556905449,0.266813137124048,-3.39118113014973));
#63349=CARTESIAN_POINT('Ctrl Pts',(-0.676699999999928,0.133441673612206,
-3.38489488157883));
#63350=CARTESIAN_POINT('Ctrl Pts',(-0.6767,3.65423931474353E-13,-3.37861797838102));
#63351=CARTESIAN_POINT('Ctrl Pts',(-0.67538587901915,-0.000318336047294726,
-3.53918202161901));
#63352=CARTESIAN_POINT('Ctrl Pts',(-0.675554870863147,-0.113267255406579,
-3.53388083833862));
#63353=CARTESIAN_POINT('Ctrl Pts',(-0.595647073307492,-0.451514156200299,
-3.51798858939529));
#63354=CARTESIAN_POINT('Ctrl Pts',(-0.0573355312236082,-0.798840329041782,
-3.49150527478905));
#63355=CARTESIAN_POINT('Ctrl Pts',(0.521602160227078,-0.533094932750431,
-3.46502761063172));
#63356=CARTESIAN_POINT('Ctrl Pts',(0.696124873969488,-0.103161075934814,
-3.44384547930587));
#63357=CARTESIAN_POINT('Ctrl Pts',(0.653250630478223,0.361151016044349,
-3.42266334798001));
#63358=CARTESIAN_POINT('Ctrl Pts',(0.271913654699282,0.69494743617245,-3.40148121665415));
#63359=CARTESIAN_POINT('Ctrl Pts',(-0.194840623075141,0.676954228271529,
-3.38029908532829));
#63360=CARTESIAN_POINT('Ctrl Pts',(-0.495439723982,0.50288890843937,-3.36441248683389));
#63361=CARTESIAN_POINT('Ctrl Pts',(-0.649643514150033,0.245229588638644,
-3.3507067989308));
#63362=CARTESIAN_POINT('Ctrl Pts',(-0.676857875978016,0.0660063189202375,
-3.34229664385917));
#63363=CARTESIAN_POINT('Ctrl Pts',(-0.677150171393189,-0.000258134096645515,
-3.33918202161901));
#63364=CARTESIAN_POINT('Origin',(0.,0.,-12.278617978381));
#63365=CARTESIAN_POINT('',(-0.6767,3.36242987921428E-13,-3.77861797838102));
#63366=CARTESIAN_POINT('',(-0.6767,3.47884921894787E-13,-3.73918202161901));
#63367=CARTESIAN_POINT('',(-0.6767,6.12423655037739E-13,-12.278617978381));
#63368=CARTESIAN_POINT('Ctrl Pts',(-0.6767,3.36242987921428E-13,-3.77861797838102));
#63369=CARTESIAN_POINT('Ctrl Pts',(-0.676700000000077,-0.155057398273079,
-3.77132430277937));
#63370=CARTESIAN_POINT('Ctrl Pts',(-0.62127275025801,-0.309905500528333,
-3.76401378127864));
#63371=CARTESIAN_POINT('Ctrl Pts',(-0.522673846984314,-0.429808026540475,
-3.75671168272746));
#63372=CARTESIAN_POINT('Ctrl Pts',(-0.398292479586412,-0.581063665748294,
-3.74750017050455));
#63373=CARTESIAN_POINT('Ctrl Pts',(-0.205569794218462,-0.673804825341075,
-3.73828865828164));
#63374=CARTESIAN_POINT('Ctrl Pts',(-0.00976117943853978,-0.676629595403548,
-3.72907714605874));
#63375=CARTESIAN_POINT('Ctrl Pts',(0.186047435341383,-0.67945436546602,
-3.71986563383583));
#63376=CARTESIAN_POINT('Ctrl Pts',(0.38136516489873,-0.592311146231187,
-3.71065412161292));
#63377=CARTESIAN_POINT('Ctrl Pts',(0.510057945616593,-0.444706399901531,
-3.70144260939002));
#63378=CARTESIAN_POINT('Ctrl Pts',(0.638750726334456,-0.297101653571876,
-3.69223109716711));
#63379=CARTESIAN_POINT('Ctrl Pts',(0.698467741207415,-0.0917316599683544,
-3.6830195849442));
#63380=CARTESIAN_POINT('Ctrl Pts',(0.668988967866939,0.101865847428509,
-3.67380807272129));
#63381=CARTESIAN_POINT('Ctrl Pts',(0.639510194526462,0.295463354825373,
-3.66459656049839));
#63382=CARTESIAN_POINT('Ctrl Pts',(0.521374118513707,0.473751951438718,
-3.65538504827548));
#63383=CARTESIAN_POINT('Ctrl Pts',(0.354581300884681,0.576363592763221,
-3.64617353605258));
#63384=CARTESIAN_POINT('Ctrl Pts',(0.187788483255655,0.678975234087723,
-3.63696202382967));
#63385=CARTESIAN_POINT('Ctrl Pts',(-0.024614289760632,0.704035524449951,
-3.62775051160676));
#63386=CARTESIAN_POINT('Ctrl Pts',(-0.210708004284066,0.6430591162021,-3.61853899938385));
#63387=CARTESIAN_POINT('Ctrl Pts',(-0.3968017188075,0.582082707954249,-3.60932748716095));
#63388=CARTESIAN_POINT('Ctrl Pts',(-0.553187021228165,0.436183450502936,
-3.60011597493804));
#63389=CARTESIAN_POINT('Ctrl Pts',(-0.626912264184211,0.254762444279815,
-3.59090446271513));
#63390=CARTESIAN_POINT('Ctrl Pts',(-0.659690958955441,0.174101553251996,
-3.5868089679371));
#63391=CARTESIAN_POINT('Ctrl Pts',(-0.676699999999955,0.0870371046709928,
-3.58271207781673));
#63392=CARTESIAN_POINT('Ctrl Pts',(-0.6767,3.5083345969789E-13,-3.57861797838102));
#63393=CARTESIAN_POINT('Ctrl Pts',(-0.6767,3.47884921894787E-13,-3.73918202161901));
#63394=CARTESIAN_POINT('Ctrl Pts',(-0.676700000000037,-0.0715671495154181,
-3.73581560648426));
#63395=CARTESIAN_POINT('Ctrl Pts',(-0.665239533861194,-0.143202031285933,
-3.73244543791216));
#63396=CARTESIAN_POINT('Ctrl Pts',(-0.642887478847484,-0.211231104577724,
-3.72907714605874));
#63397=CARTESIAN_POINT('Ctrl Pts',(-0.581759691551794,-0.39727514927755,
-3.71986563383583));
#63398=CARTESIAN_POINT('Ctrl Pts',(-0.435733252864803,-0.553541701496641,
-3.71065412161292));
#63399=CARTESIAN_POINT('Ctrl Pts',(-0.254252326446219,-0.627119322375483,
-3.70144260939002));
#63400=CARTESIAN_POINT('Ctrl Pts',(-0.0727714000276362,-0.700696943254326,
-3.69223109716711));
#63401=CARTESIAN_POINT('Ctrl Pts',(0.140848921810412,-0.690241598407965,
-3.6830195849442));
#63402=CARTESIAN_POINT('Ctrl Pts',(0.314277366395853,-0.599293439786626,
-3.67380807272129));
#63403=CARTESIAN_POINT('Ctrl Pts',(0.487705810981295,-0.508345281165287,
-3.66459656049839));
#63404=CARTESIAN_POINT('Ctrl Pts',(0.617774379810403,-0.338565648874499,
-3.65538504827548));
#63405=CARTESIAN_POINT('Ctrl Pts',(0.660442201504015,-0.147441474736689,
-3.64617353605257));
#63406=CARTESIAN_POINT('Ctrl Pts',(0.703110023197628,0.0436826994011212,
-3.63696202382967));
#63407=CARTESIAN_POINT('Ctrl Pts',(0.657597689305156,0.252660170918286,
-3.62775051160676));
#63408=CARTESIAN_POINT('Ctrl Pts',(0.539315555004391,0.408731723909835,
-3.61853899938385));
#63409=CARTESIAN_POINT('Ctrl Pts',(0.421033420703626,0.564803276901384,
-3.60932748716095));
#63410=CARTESIAN_POINT('Ctrl Pts',(0.232142132856037,0.665117969311451,
-3.60011597493804));
#63411=CARTESIAN_POINT('Ctrl Pts',(0.0365997790121158,0.675709513160992,
-3.59090446271513));
#63412=CARTESIAN_POINT('Ctrl Pts',(-0.158942574831805,0.686301057010532,
-3.58169295049223));
#63413=CARTESIAN_POINT('Ctrl Pts',(-0.357564043797021,0.606975977721903,
-3.57248143826932));
#63414=CARTESIAN_POINT('Ctrl Pts',(-0.492011926892181,0.464593536110699,
-3.56326992604641));
#63415=CARTESIAN_POINT('Ctrl Pts',(-0.609204691775011,0.340484538489852,
-3.55524062457061));
#63416=CARTESIAN_POINT('Ctrl Pts',(-0.676699999999909,0.170493761108641,
-3.5472018013875));
#63417=CARTESIAN_POINT('Ctrl Pts',(-0.6767,3.6247539367125E-13,-3.53918202161901));
#63418=CARTESIAN_POINT('Origin',(0.,0.,-12.278617978381));
#63419=CARTESIAN_POINT('',(-0.6767,3.60118402112364E-13,-3.97861797838102));
#63420=CARTESIAN_POINT('',(-0.67777021896946,-0.000635695144750592,-3.93918202161901));
#63421=CARTESIAN_POINT('',(-0.6767,6.12423655037739E-13,-12.278617978381));
#63422=CARTESIAN_POINT('Ctrl Pts',(-0.676398488294932,-0.000408318744697735,
-3.97861797838102));
#63423=CARTESIAN_POINT('Ctrl Pts',(-0.67634238392664,-0.0927455508296921,
-3.97427890318839));
#63424=CARTESIAN_POINT('Ctrl Pts',(-0.634908478920628,-0.297096589374643,
-3.9646442951643));
#63425=CARTESIAN_POINT('Ctrl Pts',(-0.433764682453468,-0.555047868816476,
-3.94971415430875));
#63426=CARTESIAN_POINT('Ctrl Pts',(-0.00876936604903183,-0.745789366591879,
-3.92853202298289));
#63427=CARTESIAN_POINT('Ctrl Pts',(0.592020032873446,-0.538508917887617,
-3.90205435882556));
#63428=CARTESIAN_POINT('Ctrl Pts',(0.773304882718845,0.208405356954825,
-3.87028116183678));
#63429=CARTESIAN_POINT('Ctrl Pts',(0.332043120165925,0.667837096325308,
-3.84380349767945));
#63430=CARTESIAN_POINT('Ctrl Pts',(-0.13136609001657,0.691357359215059,
-3.82262136635359));
#63431=CARTESIAN_POINT('Ctrl Pts',(-0.531370482730002,0.50936984768987,
-3.80265803753127));
#63432=CARTESIAN_POINT('Ctrl Pts',(-0.67533931475917,0.198712628292847,
-3.78799024154041));
#63433=CARTESIAN_POINT('Ctrl Pts',(-0.677056267769222,-2.7870685577195E-5,
-3.77861797838102));
#63434=CARTESIAN_POINT('Ctrl Pts',(-0.67777021896946,-0.000635695144750609,
-3.93918202161901));
#63435=CARTESIAN_POINT('Ctrl Pts',(-0.677903959863105,-0.0207744172333184,
-3.93823135862336));
#63436=CARTESIAN_POINT('Ctrl Pts',(-0.667985189522564,-0.265075498201874,
-3.92668962996479));
#63437=CARTESIAN_POINT('Ctrl Pts',(-0.441632977912428,-0.601015252466975,
-3.90985236847475));
#63438=CARTESIAN_POINT('Ctrl Pts',(0.0108809088601417,-0.703643129412517,
-3.88867023714889));
#63439=CARTESIAN_POINT('Ctrl Pts',(0.462129679432592,-0.586176255061214,
-3.86748810582303));
#63440=CARTESIAN_POINT('Ctrl Pts',(0.729797145596839,-0.15583677657501,
-3.84630597449717));
#63441=CARTESIAN_POINT('Ctrl Pts',(0.636487863470664,0.301849457891777,
-3.82512384317132));
#63442=CARTESIAN_POINT('Ctrl Pts',(0.416060211528914,0.570308403158517,
-3.80923724467692));
#63443=CARTESIAN_POINT('Ctrl Pts',(0.0924068473382293,0.698348703003505,
-3.79335064618252));
#63444=CARTESIAN_POINT('Ctrl Pts',(-0.370617326288914,0.647241437607997,
-3.77216851485667));
#63445=CARTESIAN_POINT('Ctrl Pts',(-0.65206223079829,0.317656845722991,
-3.75411230666883));
#63446=CARTESIAN_POINT('Ctrl Pts',(-0.67730862690677,0.0470558304535615,
-3.74135163131245));
#63447=CARTESIAN_POINT('Ctrl Pts',(-0.676873778127171,0.000939313808043477,
-3.739182021619));
#63448=CARTESIAN_POINT('Origin',(0.,0.,-12.278617978381));
#63449=CARTESIAN_POINT('',(-0.6767,3.07062044368503E-13,-4.17861797838102));
#63450=CARTESIAN_POINT('',(-0.675428755222163,-0.000265590320332854,-4.13918202161901));
#63451=CARTESIAN_POINT('',(-0.6767,6.12423655037739E-13,-12.278617978381));
#63452=CARTESIAN_POINT('Ctrl Pts',(-0.6767,3.26295015140058E-13,-4.17861797838102));
#63453=CARTESIAN_POINT('Ctrl Pts',(-0.676700000000025,-0.0523060661812641,
-4.17615757672992));
#63454=CARTESIAN_POINT('Ctrl Pts',(-0.670596734023588,-0.10470939197741,
-4.17369248129918));
#63455=CARTESIAN_POINT('Ctrl Pts',(-0.658553289072125,-0.15566134861386,
-4.17122973275826));
#63456=CARTESIAN_POINT('Ctrl Pts',(-0.613506732944653,-0.346238893799521,
-4.16201822053536));
#63457=CARTESIAN_POINT('Ctrl Pts',(-0.481332242759297,-0.514384248425477,
-4.15280670831245));
#63458=CARTESIAN_POINT('Ctrl Pts',(-0.306783749263979,-0.603163842738883,
-4.14359519608954));
#63459=CARTESIAN_POINT('Ctrl Pts',(-0.132235255768667,-0.691943437052286,
-4.13438368386664));
#63460=CARTESIAN_POINT('Ctrl Pts',(0.0814987827214579,-0.699735543875582,
-4.12517217164373));
#63461=CARTESIAN_POINT('Ctrl Pts',(0.262048589378461,-0.623901776568042,
-4.11596065942082));
#63462=CARTESIAN_POINT('Ctrl Pts',(0.442598396035471,-0.548068009260499,
-4.10674914719792));
#63463=CARTESIAN_POINT('Ctrl Pts',(0.586665887210476,-0.389993614988096,
-4.09753763497501));
#63464=CARTESIAN_POINT('Ctrl Pts',(0.645470193659864,-0.203202163120125,
-4.0883261227521));
#63465=CARTESIAN_POINT('Ctrl Pts',(0.704274500109252,-0.0164107112521548,
-4.0791146105292));
#63466=CARTESIAN_POINT('Ctrl Pts',(0.676741449973327,0.195685699109407,
-4.06990309830629));
#63467=CARTESIAN_POINT('Ctrl Pts',(0.572193660780889,0.361271787664308,
-4.06069158608338));
#63468=CARTESIAN_POINT('Ctrl Pts',(0.467645871588451,0.526857876219209,
-4.05148007386048));
#63469=CARTESIAN_POINT('Ctrl Pts',(0.287993106415111,0.642908899926974,
-4.04226856163757));
#63470=CARTESIAN_POINT('Ctrl Pts',(0.0940653136114567,0.67013029089512,
-4.03305704941466));
#63471=CARTESIAN_POINT('Ctrl Pts',(-0.0998624791921981,0.697351681863266,
-4.02384553719176));
#63472=CARTESIAN_POINT('Ctrl Pts',(-0.304522841761762,0.63524618990851,
-4.01463402496885));
#63473=CARTESIAN_POINT('Ctrl Pts',(-0.450618319796951,0.504842569385123,
-4.00542251274594));
#63474=CARTESIAN_POINT('Ctrl Pts',(-0.592325825462736,0.378355616861474,
-3.99648766795763));
#63475=CARTESIAN_POINT('Ctrl Pts',(-0.676699999999899,0.189857389572419,
-3.98754859520765));
#63476=CARTESIAN_POINT('Ctrl Pts',(-0.6767,3.60118457688074E-13,-3.97861797838102));
#63477=CARTESIAN_POINT('Ctrl Pts',(-0.675428755222163,-0.00026559032033293,
-4.13918202161901));
#63478=CARTESIAN_POINT('Ctrl Pts',(-0.675756229953581,-0.0870463508529104,
-4.13511108593427));
#63479=CARTESIAN_POINT('Ctrl Pts',(-0.639962042678306,-0.286443286036591,
-4.12574461741807));
#63480=CARTESIAN_POINT('Ctrl Pts',(-0.447211755898116,-0.54335411393822,
-4.1110826160704));
#63481=CARTESIAN_POINT('Ctrl Pts',(-0.027231621354319,-0.745938926057937,
-4.08990048474455));
#63482=CARTESIAN_POINT('Ctrl Pts',(0.455363367272391,-0.591213310405756,
-4.06871835341868));
#63483=CARTESIAN_POINT('Ctrl Pts',(0.680528182180706,-0.181965075860278,
-4.04753622209283));
#63484=CARTESIAN_POINT('Ctrl Pts',(0.686307798878026,0.165346241353982,
-4.03164962359843));
#63485=CARTESIAN_POINT('Ctrl Pts',(0.522509375349723,0.472455171517164,
-4.01576302510404));
#63486=CARTESIAN_POINT('Ctrl Pts',(0.136512190381233,0.733241503857858,
-3.99458089377818));
#63487=CARTESIAN_POINT('Ctrl Pts',(-0.468392871864562,0.635675212224839,
-3.9690538926165));
#63488=CARTESIAN_POINT('Ctrl Pts',(-0.676413990659613,0.20358534956571,
-3.94882242428629));
#63489=CARTESIAN_POINT('Ctrl Pts',(-0.67777021896946,-0.000635695144750609,
-3.93918202161901));
#63490=CARTESIAN_POINT('Origin',(0.,0.,-12.278617978381));
#63491=CARTESIAN_POINT('',(-0.677441199567872,5.70499087820638E-6,-4.37861797838101));
#63492=CARTESIAN_POINT('',(-0.676588893509693,0.000498966854468069,-4.33918202161901));
#63493=CARTESIAN_POINT('',(-0.6767,6.12423655037739E-13,-12.278617978381));
#63494=CARTESIAN_POINT('Ctrl Pts',(-0.677441199567871,5.70499087820063E-6,
-4.37861797838102));
#63495=CARTESIAN_POINT('Ctrl Pts',(-0.676753222916443,-0.224413153492785,
-4.36803835781021));
#63496=CARTESIAN_POINT('Ctrl Pts',(-0.435300975903498,-0.67140171353152,
-4.34686767157647));
#63497=CARTESIAN_POINT('Ctrl Pts',(0.33083155171032,-0.729372140157004,
-4.3151059196798));
#63498=CARTESIAN_POINT('Ctrl Pts',(0.712777470420673,-0.219561605337653,
-4.28862825552248));
#63499=CARTESIAN_POINT('Ctrl Pts',(0.660975650409514,0.241543448084987,
-4.26744612419662));
#63500=CARTESIAN_POINT('Ctrl Pts',(0.401722358340205,0.629114925446567,
-4.24626399287076));
#63501=CARTESIAN_POINT('Ctrl Pts',(-0.0926839103114625,0.74047192210371,
-4.2250818615449));
#63502=CARTESIAN_POINT('Ctrl Pts',(-0.494275113109166,0.50191832815303,
-4.20389973021904));
#63503=CARTESIAN_POINT('Ctrl Pts',(-0.650705510793311,0.245875025282787,
-4.1901769467749));
#63504=CARTESIAN_POINT('Ctrl Pts',(-0.676474114823456,0.0669674968791263,
-4.18174969616223));
#63505=CARTESIAN_POINT('Ctrl Pts',(-0.676399342971297,0.000375592675570233,
-4.17861797838102));
#63506=CARTESIAN_POINT('Ctrl Pts',(-0.676588893509694,0.000498966854468048,
-4.33918202161901));
#63507=CARTESIAN_POINT('Ctrl Pts',(-0.676405822493527,-0.0398360353532038,
-4.33728634607665));
#63508=CARTESIAN_POINT('Ctrl Pts',(-0.662272900657128,-0.193056914041967,
-4.33009513770282));
#63509=CARTESIAN_POINT('Ctrl Pts',(-0.503641062853606,-0.550919342933017,
-4.31231286366604));
#63510=CARTESIAN_POINT('Ctrl Pts',(-0.0356495923251104,-0.745397934811761,
-4.29113073234021));
#63511=CARTESIAN_POINT('Ctrl Pts',(0.400896797976255,-0.579233677324962,
-4.26994860101433));
#63512=CARTESIAN_POINT('Ctrl Pts',(0.630134791455414,-0.318257629803494,
-4.25406200251995));
#63513=CARTESIAN_POINT('Ctrl Pts',(0.704096847355287,0.0218532827285811,
-4.23817540402554));
#63514=CARTESIAN_POINT('Ctrl Pts',(0.578714001944864,0.47049844320186,-4.21699327269969));
#63515=CARTESIAN_POINT('Ctrl Pts',(0.0349786870852126,0.799534905690655,
-4.19051560854237));
#63516=CARTESIAN_POINT('Ctrl Pts',(-0.566591317156505,0.504275578643712,
-4.16281334723832));
#63517=CARTESIAN_POINT('Ctrl Pts',(-0.674904262088699,0.138725020708031,
-4.1457021515972));
#63518=CARTESIAN_POINT('Ctrl Pts',(-0.675428755222163,-0.00026559032033293,
-4.13918202161901));
#63519=CARTESIAN_POINT('Origin',(0.,0.,-12.278617978381));
#63520=CARTESIAN_POINT('',(-0.6767,2.77881016808035E-13,-4.57861797838101));
#63521=CARTESIAN_POINT('',(-0.677483499338122,-0.000155519670934575,-4.539182021619));
#63522=CARTESIAN_POINT('',(-0.6767,6.12423655037739E-13,-12.278617978381));
#63523=CARTESIAN_POINT('Ctrl Pts',(-0.676332918879227,-0.000635712003939359,
-4.57861797838102));
#63524=CARTESIAN_POINT('Ctrl Pts',(-0.676955652671927,-0.0666551245079565,
-4.57550915078405));
#63525=CARTESIAN_POINT('Ctrl Pts',(-0.637892478859078,-0.356991836088987,
-4.56180925752415));
#63526=CARTESIAN_POINT('Ctrl Pts',(-0.220004051678502,-0.770085353509153,
-4.5375182986013));
#63527=CARTESIAN_POINT('Ctrl Pts',(0.401138704855467,-0.628766061699122,
-4.51104063444399));
#63528=CARTESIAN_POINT('Ctrl Pts',(0.660153306932357,-0.243781990912655,
-4.48985850311813));
#63529=CARTESIAN_POINT('Ctrl Pts',(0.713448163538854,0.21944967658462,-4.46867637179228));
#63530=CARTESIAN_POINT('Ctrl Pts',(0.408703467624615,0.624380052697233,
-4.44749424046641));
#63531=CARTESIAN_POINT('Ctrl Pts',(-0.0518139061167167,0.702527732340824,
-4.42631210914056));
#63532=CARTESIAN_POINT('Ctrl Pts',(-0.381729763931295,0.593835130031606,
-4.41042551064616));
#63533=CARTESIAN_POINT('Ctrl Pts',(-0.617941327913625,0.338198834530834,
-4.39453891215177));
#63534=CARTESIAN_POINT('Ctrl Pts',(-0.67772194426544,0.112822645438229,
-4.38393640139672));
#63535=CARTESIAN_POINT('Ctrl Pts',(-0.677441943824823,0.000248482554735446,
-4.37862942347313));
#63536=CARTESIAN_POINT('Ctrl Pts',(-0.677441199567871,5.70499087820063E-6,
-4.37861797838102));
#63537=CARTESIAN_POINT('Ctrl Pts',(-0.677483499338121,-0.000155519670934546,
-4.539182021619));
#63538=CARTESIAN_POINT('Ctrl Pts',(-0.67666748440995,-0.218510581706608,
-4.52887054055609));
#63539=CARTESIAN_POINT('Ctrl Pts',(-0.503895417062598,-0.547116013156695,
-4.5132635266617));
#63540=CARTESIAN_POINT('Ctrl Pts',(-0.0694084667398682,-0.701008102891709,
-4.49236097993585));
#63541=CARTESIAN_POINT('Ctrl Pts',(0.274258103338072,-0.650492326691175,
-4.47647438144146));
#63542=CARTESIAN_POINT('Ctrl Pts',(0.550802926396446,-0.439142428711666,
-4.46058778294706));
#63543=CARTESIAN_POINT('Ctrl Pts',(0.745668804766385,-0.0160223188298255,
-4.4394056516212));
#63544=CARTESIAN_POINT('Ctrl Pts',(0.544241292482002,0.586754624630679,
-4.41292798746388));
#63545=CARTESIAN_POINT('Ctrl Pts',(-0.200874523336002,0.775295208497259,
-4.3811547904751));
#63546=CARTESIAN_POINT('Ctrl Pts',(-0.63137729592835,0.369793488861541,
-4.35657280186013));
#63547=CARTESIAN_POINT('Ctrl Pts',(-0.676917227823677,0.0728390103888557,
-4.34258187890811));
#63548=CARTESIAN_POINT('Ctrl Pts',(-0.676588893509694,0.000498966854468048,
-4.33918202161901));
#63549=CARTESIAN_POINT('Origin',(0.,0.,-12.278617978381));
#63550=CARTESIAN_POINT('',(-0.676672460315546,1.17798547158296E-5,-4.77861797838102));
#63551=CARTESIAN_POINT('',(-0.6767,2.94165516598333E-13,-4.739182021619));
#63552=CARTESIAN_POINT('',(-0.6767,6.12423655037739E-13,-12.278617978381));
#63553=CARTESIAN_POINT('Ctrl Pts',(-0.6767,2.8252359981067E-13,-4.77861797838101));
#63554=CARTESIAN_POINT('Ctrl Pts',(-0.67670000000008,-0.191713242581063,
-4.76960006491478));
#63555=CARTESIAN_POINT('Ctrl Pts',(-0.590610559833386,-0.381943871873007,
-4.76057599466127));
#63556=CARTESIAN_POINT('Ctrl Pts',(-0.446504609572047,-0.508484536275111,
-4.75155500280139));
#63557=CARTESIAN_POINT('Ctrl Pts',(-0.299355189325865,-0.637697697637065,
-4.74234349057849));
#63558=CARTESIAN_POINT('Ctrl Pts',(-0.0941973328990827,-0.698139488514034,
-4.73313197835558));
#63559=CARTESIAN_POINT('Ctrl Pts',(0.0995030553114643,-0.669344479310679,
-4.72392046613267));
#63560=CARTESIAN_POINT('Ctrl Pts',(0.293203443522011,-0.640549470107323,
-4.71470895390977));
#63561=CARTESIAN_POINT('Ctrl Pts',(0.471908059626845,-0.523043656119796,
-4.70549744168686));
#63562=CARTESIAN_POINT('Ctrl Pts',(0.575107996027578,-0.356614193359074,
-4.69628592946395));
#63563=CARTESIAN_POINT('Ctrl Pts',(0.678307932428311,-0.190184730598352,
-4.68707441724105));
#63564=CARTESIAN_POINT('Ctrl Pts',(0.704118047129442,0.0221282320703506,
-4.67786290501814));
#63565=CARTESIAN_POINT('Ctrl Pts',(0.6437991039568,0.208436090311686,-4.66865139279523));
#63566=CARTESIAN_POINT('Ctrl Pts',(0.583480160784159,0.394743948553022,
-4.65943988057233));
#63567=CARTESIAN_POINT('Ctrl Pts',(0.438133999301458,0.551643437017108,
-4.65022836834942));
#63568=CARTESIAN_POINT('Ctrl Pts',(0.256974443116801,0.626008806315702,
-4.64101685612651));
#63569=CARTESIAN_POINT('Ctrl Pts',(0.0758148869321448,0.700374175614296,
-4.63180534390361));
#63570=CARTESIAN_POINT('Ctrl Pts',(-0.137848842077393,0.690847001647876,
-4.6225938316807));
#63571=CARTESIAN_POINT('Ctrl Pts',(-0.311670773686952,0.600653160175968,
-4.61338231945779));
#63572=CARTESIAN_POINT('Ctrl Pts',(-0.485492705296511,0.51045931870406,
-4.60417080723489));
#63573=CARTESIAN_POINT('Ctrl Pts',(-0.616297653217761,0.341246370803001,
-4.59495929501198));
#63574=CARTESIAN_POINT('Ctrl Pts',(-0.659795410069959,0.150309370468427,
-4.58574778278907));
#63575=CARTESIAN_POINT('Ctrl Pts',(-0.671017979214619,0.101046975264696,
-4.58337118131972));
#63576=CARTESIAN_POINT('Ctrl Pts',(-0.676699999999979,0.0504745568557825,
-4.58099222848414));
#63577=CARTESIAN_POINT('Ctrl Pts',(-0.6767,2.77881100815578E-13,-4.57861797838101));
#63578=CARTESIAN_POINT('Ctrl Pts',(-0.676059626651951,-0.000187573017024642,
-4.739182021619));
#63579=CARTESIAN_POINT('Ctrl Pts',(-0.676604188211727,-0.0605326678519595,
-4.73634133352992));
#63580=CARTESIAN_POINT('Ctrl Pts',(-0.655486634525628,-0.233258944214111,
-4.72820511260937));
#63581=CARTESIAN_POINT('Ctrl Pts',(-0.506701789827963,-0.489370199092825,
-4.71477335885737));
#63582=CARTESIAN_POINT('Ctrl Pts',(-0.212060776109364,-0.673340925212919,
-4.69888676036297));
#63583=CARTESIAN_POINT('Ctrl Pts',(0.13553701687756,-0.691273935193279,
-4.68300016186857));
#63584=CARTESIAN_POINT('Ctrl Pts',(0.557969828113902,-0.494922571739213,
-4.66181803054273));
#63585=CARTESIAN_POINT('Ctrl Pts',(0.794652742927993,0.0949030669946144,
-4.63534036638539));
#63586=CARTESIAN_POINT('Ctrl Pts',(0.348784514783706,0.720959497261372,
-4.6035671693966));
#63587=CARTESIAN_POINT('Ctrl Pts',(-0.287390379613016,0.68823381970347,
-4.57708950523929));
#63588=CARTESIAN_POINT('Ctrl Pts',(-0.608578462087337,0.353361434271592,
-4.55590737391342));
#63589=CARTESIAN_POINT('Ctrl Pts',(-0.676285382095685,0.123841442227276,
-4.54503672365049));
#63590=CARTESIAN_POINT('Ctrl Pts',(-0.677505624695856,0.00576494047506343,
-4.53946160621901));
#63591=CARTESIAN_POINT('Ctrl Pts',(-0.677483499338121,-0.000155519670934546,
-4.539182021619));
#63592=CARTESIAN_POINT('Origin',(0.,0.,-12.278617978381));
#63593=CARTESIAN_POINT('',(-0.677644860324165,0.000269891732193889,-4.97861797838101));
#63594=CARTESIAN_POINT('',(-0.6767,2.60342091236013E-13,-4.939182021619));
#63595=CARTESIAN_POINT('',(-0.6767,6.12423655037739E-13,-12.278617978381));
#63596=CARTESIAN_POINT('Ctrl Pts',(-0.677644860324165,0.000269891732193914,
-4.97861797838101));
#63597=CARTESIAN_POINT('Ctrl Pts',(-0.675978634032105,-0.197648105273453,
-4.96926860540586));
#63598=CARTESIAN_POINT('Ctrl Pts',(-0.530813983809632,-0.508956833739578,
-4.95462369959923));
#63599=CARTESIAN_POINT('Ctrl Pts',(-0.133708223738798,-0.690908212899286,
-4.93468326096116));
#63600=CARTESIAN_POINT('Ctrl Pts',(0.332041232394348,-0.668517062310377,
-4.91350112963529));
#63601=CARTESIAN_POINT('Ctrl Pts',(0.682302518044435,-0.302245344918345,
-4.89231899830944));
#63602=CARTESIAN_POINT('Ctrl Pts',(0.684875796890799,0.164848531713828,
-4.87113686698358));
#63603=CARTESIAN_POINT('Ctrl Pts',(0.524213242357612,0.472819469636789,
-4.85525026848919));
#63604=CARTESIAN_POINT('Ctrl Pts',(0.23371275114266,0.664536143768718,-4.83936366999479));
#63605=CARTESIAN_POINT('Ctrl Pts',(-0.229947459772284,0.709508877214857,
-4.81818153866894));
#63606=CARTESIAN_POINT('Ctrl Pts',(-0.614678118223211,0.412519780986417,
-4.79793297479767));
#63607=CARTESIAN_POINT('Ctrl Pts',(-0.676025351084611,0.0936457920984287,
-4.78297994375788));
#63608=CARTESIAN_POINT('Ctrl Pts',(-0.675657090930862,0.000446095054207521,
-4.77861797838102));
#63609=CARTESIAN_POINT('Ctrl Pts',(-0.6767,2.60342091236013E-13,-4.939182021619));
#63610=CARTESIAN_POINT('Ctrl Pts',(-0.676700000000059,-0.154446373905746,
-4.93191708771927));
#63611=CARTESIAN_POINT('Ctrl Pts',(-0.6217245569102,-0.30869061553757,-4.92463548908214));
#63612=CARTESIAN_POINT('Ctrl Pts',(-0.523839866944655,-0.428386138663947,
-4.91736222281372));
#63613=CARTESIAN_POINT('Ctrl Pts',(-0.399869977107543,-0.579979210279085,
-4.90815071059081));
#63614=CARTESIAN_POINT('Ctrl Pts',(-0.207400015820569,-0.673243727327307,
-4.8989391983679));
#63615=CARTESIAN_POINT('Ctrl Pts',(-0.0115997999403209,-0.676600572451239,
-4.889727686145));
#63616=CARTESIAN_POINT('Ctrl Pts',(0.184200415939927,-0.679957417575171,
-4.88051617392209));
#63617=CARTESIAN_POINT('Ctrl Pts',(0.379754225200688,-0.593345271650633,
-4.87130466169918));
#63618=CARTESIAN_POINT('Ctrl Pts',(0.508847628265527,-0.446090776870076,
-4.86209314947628));
#63619=CARTESIAN_POINT('Ctrl Pts',(0.637941031330366,-0.29883628208952,
-4.85288163725337));
#63620=CARTESIAN_POINT('Ctrl Pts',(0.698215893069096,-0.0936293202670115,
-4.84367012503046));
#63621=CARTESIAN_POINT('Ctrl Pts',(0.669263305648498,0.100047577244257,
-4.83445861280756));
#63622=CARTESIAN_POINT('Ctrl Pts',(0.640310718227899,0.293724474755526,
-4.82524710058465));
#63623=CARTESIAN_POINT('Ctrl Pts',(0.522659555408253,0.472333433168122,
-4.81603558836174));
#63624=CARTESIAN_POINT('Ctrl Pts',(0.356146187928414,0.575397934323768,
-4.80682407613883));
#63625=CARTESIAN_POINT('Ctrl Pts',(0.189632820448575,0.678462435479413,
-4.79761256391593));
#63626=CARTESIAN_POINT('Ctrl Pts',(-0.0227010701478788,0.704099811363474,
-4.78840105169302));
#63627=CARTESIAN_POINT('Ctrl Pts',(-0.208959793384939,0.643629314705696,
-4.77918953947011));
#63628=CARTESIAN_POINT('Ctrl Pts',(-0.395218516621998,0.583158818047918,
-4.76997802724721));
#63629=CARTESIAN_POINT('Ctrl Pts',(-0.551999704693553,0.437685056823018,
-4.7607665150243));
#63630=CARTESIAN_POINT('Ctrl Pts',(-0.62621766440955,0.256465059572349,
-4.75155500280139));
#63631=CARTESIAN_POINT('Ctrl Pts',(-0.659447728295543,0.175326314865503,
-4.7474306757406));
#63632=CARTESIAN_POINT('Ctrl Pts',(-0.676699999999962,0.087650303709258,
-4.74330496505));
#63633=CARTESIAN_POINT('Ctrl Pts',(-0.6767,2.9416553378403E-13,-4.739182021619));
#63634=CARTESIAN_POINT('Origin',(0.,0.,-12.278617978381));
#63635=CARTESIAN_POINT('',(-0.676546632405414,-0.000558781037866288,-5.17861797838101));
#63636=CARTESIAN_POINT('',(-0.676681193656348,0.000319961310848924,-5.139182021619));
#63637=CARTESIAN_POINT('',(-0.6767,6.12423655037739E-13,-12.278617978381));
#63638=CARTESIAN_POINT('Ctrl Pts',(-0.676546632405414,-0.000558781037866309,
-5.17861797838101));
#63639=CARTESIAN_POINT('Ctrl Pts',(-0.676910944207348,-0.0404440489505496,
-5.1767393983797));
#63640=CARTESIAN_POINT('Ctrl Pts',(-0.664788307948526,-0.192568022435409,
-5.16956528554692));
#63641=CARTESIAN_POINT('Ctrl Pts',(-0.549172285849032,-0.440047552208631,
-5.15709563988267));
#63642=CARTESIAN_POINT('Ctrl Pts',(-0.179687362077751,-0.724485261766983,
-5.1359135085568));
#63643=CARTESIAN_POINT('Ctrl Pts',(0.324385456870523,-0.67205881440986,
-5.11473137723096));
#63644=CARTESIAN_POINT('Ctrl Pts',(0.628721139150488,-0.317709969564103,
-5.09354924590509));
#63645=CARTESIAN_POINT('Ctrl Pts',(0.705631348411274,0.0210279449736901,
-5.0776626474107));
#63646=CARTESIAN_POINT('Ctrl Pts',(0.608322795378933,0.355208830188862,
-5.0617760489163));
#63647=CARTESIAN_POINT('Ctrl Pts',(0.284038448676206,0.689638195560499,
-5.04059391759044));
#63648=CARTESIAN_POINT('Ctrl Pts',(-0.350809927077043,0.719313540142401,
-5.01411625343312));
#63649=CARTESIAN_POINT('Ctrl Pts',(-0.664677743479125,0.276906197068003,
-4.99169242941949));
#63650=CARTESIAN_POINT('Ctrl Pts',(-0.677866152276955,0.0265554330528713,
-4.97985967106879));
#63651=CARTESIAN_POINT('Ctrl Pts',(-0.677644860324165,0.000269891732193914,
-4.97861797838101));
#63652=CARTESIAN_POINT('Ctrl Pts',(-0.676681193656349,0.000319961310848927,
-5.139182021619));
#63653=CARTESIAN_POINT('Ctrl Pts',(-0.676458674215642,-0.0800116306119912,
-5.1353963209832));
#63654=CARTESIAN_POINT('Ctrl Pts',(-0.641533144143856,-0.273093713028534,
-5.12631508751594));
#63655=CARTESIAN_POINT('Ctrl Pts',(-0.398077205723047,-0.630724360863014,
-5.10664278838574));
#63656=CARTESIAN_POINT('Ctrl Pts',(0.222281684997194,-0.768811047320993,
-5.08016512422842));
#63657=CARTESIAN_POINT('Ctrl Pts',(0.767909224957921,-0.227483310747878,
-5.04839192723964));
#63658=CARTESIAN_POINT('Ctrl Pts',(0.632637701696453,0.39500450537932,-5.0219142630823));
#63659=CARTESIAN_POINT('Ctrl Pts',(0.250190952797296,0.657751119258226,
-5.00073213175645));
#63660=CARTESIAN_POINT('Ctrl Pts',(-0.212500472627088,0.715548734708769,
-4.97955000043058));
#63661=CARTESIAN_POINT('Ctrl Pts',(-0.607562341949752,0.424205965160257,
-4.95903329705144));
#63662=CARTESIAN_POINT('Ctrl Pts',(-0.676723613838758,0.098630709613695,
-4.94381212650376));
#63663=CARTESIAN_POINT('Ctrl Pts',(-0.676504186696694,-0.000135632411926398,
-4.939182021619));
#63664=CARTESIAN_POINT('Origin',(0.,0.,-12.278617978381));
#63665=CARTESIAN_POINT('',(-0.6767,2.19519227014769E-13,-5.37861797838101));
#63666=CARTESIAN_POINT('',(-0.677314241554135,-0.00024113045791524,-5.339182021619));
#63667=CARTESIAN_POINT('',(-0.6767,6.12423655037739E-13,-12.278617978381));
#63668=CARTESIAN_POINT('Ctrl Pts',(-0.676213525726746,6.46560819233264E-5,
-5.37861797838101));
#63669=CARTESIAN_POINT('Ctrl Pts',(-0.67625358434725,-0.106616645045719,
-5.3736191256906));
#63670=CARTESIAN_POINT('Ctrl Pts',(-0.600096841340238,-0.439885678167944,
-5.35802920733728));
#63671=CARTESIAN_POINT('Ctrl Pts',(-0.187815285885199,-0.722228768117197,
-5.33714375615245));
#63672=CARTESIAN_POINT('Ctrl Pts',(0.273535159807509,-0.649159773727578,
-5.31596162482661));
#63673=CARTESIAN_POINT('Ctrl Pts',(0.551438224564908,-0.44076485660649,
-5.3000750263322));
#63674=CARTESIAN_POINT('Ctrl Pts',(0.693603344904396,-0.123062327230168,
-5.28418842783782));
#63675=CARTESIAN_POINT('Ctrl Pts',(0.662930453897055,0.341762921281637,
-5.26300629651195));
#63676=CARTESIAN_POINT('Ctrl Pts',(0.198265258367223,0.775351830664549,
-5.23652863235464));
#63677=CARTESIAN_POINT('Ctrl Pts',(-0.502472826500339,0.596687001070201,
-5.20663401536716));
#63678=CARTESIAN_POINT('Ctrl Pts',(-0.67485702570861,0.184421270147124,
-5.18733046404262));
#63679=CARTESIAN_POINT('Ctrl Pts',(-0.676546632405414,-0.000558781037866309,
-5.17861797838101));
#63680=CARTESIAN_POINT('Ctrl Pts',(-0.677314241554135,-0.000241130457915198,
-5.339182021619));
#63681=CARTESIAN_POINT('Ctrl Pts',(-0.677442214828523,-0.0344734714592605,
-5.33757158112557));
#63682=CARTESIAN_POINT('Ctrl Pts',(-0.658345400178551,-0.293576636578878,
-5.32537007496922));
#63683=CARTESIAN_POINT('Ctrl Pts',(-0.328270635324783,-0.729875307140714,
-5.30257750314993));
#63684=CARTESIAN_POINT('Ctrl Pts',(0.438031486668258,-0.670493587687057,
-5.27080430616114));
#63685=CARTESIAN_POINT('Ctrl Pts',(0.737897769931333,-0.108470742618401,
-5.24432664200382));
#63686=CARTESIAN_POINT('Ctrl Pts',(0.616490027294739,0.339370143052669,
-5.22314451067796));
#63687=CARTESIAN_POINT('Ctrl Pts',(0.301246298432971,0.682947370072152,
-5.2019623793521));
#63688=CARTESIAN_POINT('Ctrl Pts',(-0.204350803094626,0.717725381973961,
-5.18078024802625));
#63689=CARTESIAN_POINT('Ctrl Pts',(-0.564936112187733,0.420805281242191,
-5.15959811670039));
#63690=CARTESIAN_POINT('Ctrl Pts',(-0.666891133314686,0.176652537412118,
-5.14749721884179));
#63691=CARTESIAN_POINT('Ctrl Pts',(-0.676769939980493,0.0323582114215476,
-5.14069185381466));
#63692=CARTESIAN_POINT('Ctrl Pts',(-0.676681193656349,0.000319961310848927,
-5.139182021619));
#63693=CARTESIAN_POINT('Origin',(0.,0.,-12.278617978381));
#63694=CARTESIAN_POINT('',(-0.6767,2.04928741933266E-13,-5.57861797838101));
#63695=CARTESIAN_POINT('',(-0.676473652988121,-8.72929341335908E-5,-5.539182021619));
#63696=CARTESIAN_POINT('',(-0.6767,6.12423655037739E-13,-12.278617978381));
#63697=CARTESIAN_POINT('Ctrl Pts',(-0.6767,2.04928741933266E-13,-5.57861797838101));
#63698=CARTESIAN_POINT('Ctrl Pts',(-0.676700000000055,-0.181681376406979,
-5.57007194938059));
#63699=CARTESIAN_POINT('Ctrl Pts',(-0.599682817833766,-0.362452229318455,
-5.56151037025653));
#63700=CARTESIAN_POINT('Ctrl Pts',(-0.468453904192104,-0.488337823281358,
-5.55295656619429));
#63701=CARTESIAN_POINT('Ctrl Pts',(-0.327134704779409,-0.623902851313269,
-5.54374505397138));
#63702=CARTESIAN_POINT('Ctrl Pts',(-0.124836170252917,-0.693316532000011,
-5.53453354174847));
#63703=CARTESIAN_POINT('Ctrl Pts',(0.0699439537792119,-0.673075577724918,
-5.52532202952557));
#63704=CARTESIAN_POINT('Ctrl Pts',(0.264724077811341,-0.652834623449824,
-5.51611051730266));
#63705=CARTESIAN_POINT('Ctrl Pts',(0.448427764043003,-0.543308773519562,
-5.50689900507975));
#63706=CARTESIAN_POINT('Ctrl Pts',(0.558853433030084,-0.381583189344721,
-5.49768749285685));
#63707=CARTESIAN_POINT('Ctrl Pts',(0.669279102017165,-0.21985760516988,
-5.48847598063394));
#63708=CARTESIAN_POINT('Ctrl Pts',(0.704409620094189,-0.00888651037799307,
-5.47926446841103));
#63709=CARTESIAN_POINT('Ctrl Pts',(0.652349887299333,0.17989584358886,-5.47005295618813));
#63710=CARTESIAN_POINT('Ctrl Pts',(0.600290154504477,0.368678197555713,
-5.46084144396522));
#63711=CARTESIAN_POINT('Ctrl Pts',(0.461991140305252,0.531823344003806,
-5.45162993174231));
#63712=CARTESIAN_POINT('Ctrl Pts',(0.284280522987371,0.614090770367074,
-5.44241841951941));
#63713=CARTESIAN_POINT('Ctrl Pts',(0.106569905669491,0.696358196730342,
-5.4332069072965));
#63714=CARTESIAN_POINT('Ctrl Pts',(-0.107306094280518,0.696245132893723,
-5.42399539507359));
#63715=CARTESIAN_POINT('Ctrl Pts',(-0.284929632262066,0.613789861971509,
-5.41478388285069));
#63716=CARTESIAN_POINT('Ctrl Pts',(-0.462553170243613,0.531334591049295,
-5.40557237062778));
#63717=CARTESIAN_POINT('Ctrl Pts',(-0.600679616438922,0.36804331449264,
-5.39636085840487));
#63718=CARTESIAN_POINT('Ctrl Pts',(-0.652539723629315,0.179206024133614,
-5.38714934618197));
#63719=CARTESIAN_POINT('Ctrl Pts',(-0.668550039052439,0.120907945975067,
-5.38430555691498));
#63720=CARTESIAN_POINT('Ctrl Pts',(-0.67669999999998,0.0604092412225694,
-5.38145954165838));
#63721=CARTESIAN_POINT('Ctrl Pts',(-0.6767,2.19519213709729E-13,-5.37861797838101));
#63722=CARTESIAN_POINT('Ctrl Pts',(-0.675509068550524,-0.000459294334369663,
-5.539182021619));
#63723=CARTESIAN_POINT('Ctrl Pts',(-0.675920327415641,-0.101206008316284,
-5.53445130843648));
#63724=CARTESIAN_POINT('Ctrl Pts',(-0.607873754724515,-0.426945848796192,
-5.51912952959103));
#63725=CARTESIAN_POINT('Ctrl Pts',(-0.100182069364385,-0.794604796709607,
-5.49321668508265));
#63726=CARTESIAN_POINT('Ctrl Pts',(0.492200104289347,-0.56035531426314,
-5.46673902092533));
#63727=CARTESIAN_POINT('Ctrl Pts',(0.689575122107159,-0.140421506011553,
-5.44555688959948));
#63728=CARTESIAN_POINT('Ctrl Pts',(0.671714796398658,0.325523691904682,
-5.42437475827361));
#63729=CARTESIAN_POINT('Ctrl Pts',(0.308866959837698,0.679330682531593,
-5.40319262694776));
#63730=CARTESIAN_POINT('Ctrl Pts',(-0.158179798246442,0.686446681763176,
-5.3820104956219));
#63731=CARTESIAN_POINT('Ctrl Pts',(-0.467698735375229,0.528786977202589,
-5.36612389712751));
#63732=CARTESIAN_POINT('Ctrl Pts',(-0.642511679277089,0.269422734927641,
-5.35184773912654));
#63733=CARTESIAN_POINT('Ctrl Pts',(-0.677021406559707,0.078091063778343,
-5.34286711395704));
#63734=CARTESIAN_POINT('Ctrl Pts',(-0.677314241554135,-0.000241130457915198,
-5.339182021619));
#63735=CARTESIAN_POINT('Origin',(0.,0.,-12.278617978381));
#63736=CARTESIAN_POINT('',(-0.6767,1.90338270156804E-13,-5.77861797838101));
#63737=CARTESIAN_POINT('',(-0.676682641762153,7.35447311691314E-5,-5.739182021619));
#63738=CARTESIAN_POINT('',(-0.6767,6.12423655037739E-13,-12.278617978381));
#63739=CARTESIAN_POINT('Ctrl Pts',(-0.6767,1.90338270156804E-13,-5.77861797838101));
#63740=CARTESIAN_POINT('Ctrl Pts',(-0.676700000000009,-0.0324523956795152,
-5.77709146465629));
#63741=CARTESIAN_POINT('Ctrl Pts',(-0.674355800339294,-0.0649836093856385,
-5.77556123248971));
#63742=CARTESIAN_POINT('Ctrl Pts',(-0.669691645670928,-0.0971390226354201,
-5.77403285954405));
#63743=CARTESIAN_POINT('Ctrl Pts',(-0.641580759607818,-0.290939876691033,
-5.76482134732115));
#63744=CARTESIAN_POINT('Ctrl Pts',(-0.524706672654737,-0.470058284279229,
-5.75560983509824));
#63745=CARTESIAN_POINT('Ctrl Pts',(-0.358642639729406,-0.573845229106179,
-5.74639832287533));
#63746=CARTESIAN_POINT('Ctrl Pts',(-0.192578606804075,-0.67763217393313,
-5.73718681065243));
#63747=CARTESIAN_POINT('Ctrl Pts',(0.0196418984952844,-0.704191791184361,
-5.72797529842952));
#63748=CARTESIAN_POINT('Ctrl Pts',(0.206161577652617,-0.64453106511617,
-5.71876378620661));
#63749=CARTESIAN_POINT('Ctrl Pts',(0.392681256809949,-0.584870339047978,
-5.70955227398371));
#63750=CARTESIAN_POINT('Ctrl Pts',(0.550092975165776,-0.440079085643937,
-5.7003407617608));
#63751=CARTESIAN_POINT('Ctrl Pts',(0.625097543653214,-0.259183238112958,
-5.69112924953789));
#63752=CARTESIAN_POINT('Ctrl Pts',(0.700102112140652,-0.0782873905819796,
-5.68191773731498));
#63753=CARTESIAN_POINT('Ctrl Pts',(0.691329430478235,0.13540864633611,-5.67270622509208));
#63754=CARTESIAN_POINT('Ctrl Pts',(0.601749905338556,0.309547963044565,
-5.66349471286917));
#63755=CARTESIAN_POINT('Ctrl Pts',(0.512170380198877,0.483687279753019,
-5.65428320064626));
#63756=CARTESIAN_POINT('Ctrl Pts',(0.343420351008757,0.615088892324483,
-5.64507168842336));
#63757=CARTESIAN_POINT('Ctrl Pts',(0.15263812871983,0.659260564314982,-5.63586017620045));
#63758=CARTESIAN_POINT('Ctrl Pts',(-0.0381440935690977,0.703432236305481,
-5.62664866397754));
#63759=CARTESIAN_POINT('Ctrl Pts',(-0.247473510886337,0.659567088594882,
-5.61743715175464));
#63760=CARTESIAN_POINT('Ctrl Pts',(-0.404471739415305,0.542517743501867,
-5.60822563953173));
#63761=CARTESIAN_POINT('Ctrl Pts',(-0.561469967944274,0.425468398408852,
-5.59901412730882));
#63762=CARTESIAN_POINT('Ctrl Pts',(-0.663269138148019,0.237372983568734,
-5.58980261508592));
#63763=CARTESIAN_POINT('Ctrl Pts',(-0.675400321815768,0.0419201060489659,
-5.58059110286301));
#63764=CARTESIAN_POINT('Ctrl Pts',(-0.676266496478922,0.0279646392961009,
-5.57993339470234));
#63765=CARTESIAN_POINT('Ctrl Pts',(-0.676699999999996,0.0139696120037695,
-5.57927508871157));
#63766=CARTESIAN_POINT('Ctrl Pts',(-0.6767,2.04928741933266E-13,-5.57861797838101));
#63767=CARTESIAN_POINT('Ctrl Pts',(-0.6767,2.01980204130163E-13,-5.739182021619));
#63768=CARTESIAN_POINT('Ctrl Pts',(-0.676700000000043,-0.144550082451763,
-5.73238259494645));
#63769=CARTESIAN_POINT('Ctrl Pts',(-0.628766694107548,-0.288982634149047,
-5.72556986467741));
#63770=CARTESIAN_POINT('Ctrl Pts',(-0.542188500137206,-0.404912978699086,
-5.71876378620661));
#63771=CARTESIAN_POINT('Ctrl Pts',(-0.425011465605937,-0.561815928086265,
-5.7095522739837));
#63772=CARTESIAN_POINT('Ctrl Pts',(-0.236833292830468,-0.663462036860449,
-5.7003407617608));
#63773=CARTESIAN_POINT('Ctrl Pts',(-0.0413706104950007,-0.67543420300372,
-5.69112924953789));
#63774=CARTESIAN_POINT('Ctrl Pts',(0.154092071840467,-0.687406369146992,
-5.68191773731498));
#63775=CARTESIAN_POINT('Ctrl Pts',(0.353268768211662,-0.609485898404675,
-5.67270622509208));
#63776=CARTESIAN_POINT('Ctrl Pts',(0.488718779104662,-0.468056454875316,
-5.66349471286917));
#63777=CARTESIAN_POINT('Ctrl Pts',(0.624168789997662,-0.326627011345958,
-5.65428320064626));
#63778=CARTESIAN_POINT('Ctrl Pts',(0.693417864819581,-0.124272071267007,
-5.64507168842336));
#63779=CARTESIAN_POINT('Ctrl Pts',(0.673018451061671,0.0704915209833714,
-5.63586017620045));
#63780=CARTESIAN_POINT('Ctrl Pts',(0.652619037303762,0.265255113233749,
-5.62664866397754));
#63781=CARTESIAN_POINT('Ctrl Pts',(0.542943768834802,0.448869632333708,
-5.61743715175464));
#63782=CARTESIAN_POINT('Ctrl Pts',(0.381128399785082,0.559163690592713,
-5.60822563953173));
#63783=CARTESIAN_POINT('Ctrl Pts',(0.219313030735361,0.669457748851717,
-5.59901412730882));
#63784=CARTESIAN_POINT('Ctrl Pts',(0.0083134248229402,0.704416616723123,
-5.58980261508592));
#63785=CARTESIAN_POINT('Ctrl Pts',(-0.180426512720538,0.652203314548083,
-5.58059110286301));
#63786=CARTESIAN_POINT('Ctrl Pts',(-0.369166450264015,0.599990012373043,
-5.5713795906401));
#63787=CARTESIAN_POINT('Ctrl Pts',(-0.53219902756101,0.461558314854205,
-5.56216807841719));
#63788=CARTESIAN_POINT('Ctrl Pts',(-0.614321847660544,0.283780826496322,
-5.55295656619429));
#63789=CARTESIAN_POINT('Ctrl Pts',(-0.655256293555913,0.195166931238217,
-5.54836505133586));
#63790=CARTESIAN_POINT('Ctrl Pts',(-0.676699999999966,0.0975831743075417,
-5.5437721929072));
#63791=CARTESIAN_POINT('Ctrl Pts',(-0.6767,2.3580364667818E-13,-5.539182021619));
#63792=CARTESIAN_POINT('Origin',(0.,0.,-12.278617978381));
#63793=CARTESIAN_POINT('',(-0.675992408981733,-0.00051856590770552,-5.97861797838101));
#63794=CARTESIAN_POINT('',(-0.677862131410808,-0.000317623256960498,-5.939182021619));
#63795=CARTESIAN_POINT('',(-0.6767,6.12423655037739E-13,-12.278617978381));
#63796=CARTESIAN_POINT('Ctrl Pts',(-0.675992408981733,-0.000518565907705555,
-5.97861797838101));
#63797=CARTESIAN_POINT('Ctrl Pts',(-0.676480548855683,-0.0808249889540484,
-5.97484937328625));
#63798=CARTESIAN_POINT('Ctrl Pts',(-0.625946858428093,-0.386173097447615,
-5.96048970252857));
#63799=CARTESIAN_POINT('Ctrl Pts',(-0.172598743972036,-0.781008560151051,
-5.93553896610797));
#63800=CARTESIAN_POINT('Ctrl Pts',(0.562958377491915,-0.568642748947718,
-5.90376576911917));
#63801=CARTESIAN_POINT('Ctrl Pts',(0.78296431633078,0.166020846752831,-5.87199257213039));
#63802=CARTESIAN_POINT('Ctrl Pts',(0.367652295433943,0.649277541756489,
-5.84551490797305));
#63803=CARTESIAN_POINT('Ctrl Pts',(-0.094108426135513,0.697311105773554,
-5.82433277664721));
#63804=CARTESIAN_POINT('Ctrl Pts',(-0.51485447745632,0.532696085594891,
-5.803798977727));
#63805=CARTESIAN_POINT('Ctrl Pts',(-0.675957546053224,0.210905853308733,
-5.78856071163828));
#63806=CARTESIAN_POINT('Ctrl Pts',(-0.677343470085779,8.23098365132415E-5,
-5.77861797838101));
#63807=CARTESIAN_POINT('Ctrl Pts',(-0.677862131410808,-0.000317623256960531,
-5.939182021619));
#63808=CARTESIAN_POINT('Ctrl Pts',(-0.677882831941353,-0.00835939249928384,
-5.93880182872123));
#63809=CARTESIAN_POINT('Ctrl Pts',(-0.673999656496432,-0.240380536296751,
-5.92783057016052));
#63810=CARTESIAN_POINT('Ctrl Pts',(-0.473532610433715,-0.576625011097358,
-5.91156377876836));
#63811=CARTESIAN_POINT('Ctrl Pts',(-0.0268458389766041,-0.703120526676957,
-5.8903816474425));
#63812=CARTESIAN_POINT('Ctrl Pts',(0.429873304441071,-0.610241380137162,
-5.86919951611663));
#63813=CARTESIAN_POINT('Ctrl Pts',(0.72041369487452,-0.194790217664389,
-5.84801738479079));
#63814=CARTESIAN_POINT('Ctrl Pts',(0.651769364779252,0.267190941228426,
-5.82683525346492));
#63815=CARTESIAN_POINT('Ctrl Pts',(0.446117917906169,0.547134871850125,
-5.81094865497054));
#63816=CARTESIAN_POINT('Ctrl Pts',(0.129797396400296,0.692369309990026,
-5.79506205647613));
#63817=CARTESIAN_POINT('Ctrl Pts',(-0.335295695534132,0.666226148989499,
-5.77387992515028));
#63818=CARTESIAN_POINT('Ctrl Pts',(-0.643488391291915,0.342319004679031,
-5.75525324686457));
#63819=CARTESIAN_POINT('Ctrl Pts',(-0.67701347904639,0.0592534314261598,
-5.74192210141032));
#63820=CARTESIAN_POINT('Ctrl Pts',(-0.676484660513756,0.000912367068930366,
-5.739182021619));
#63821=CARTESIAN_POINT('Origin',(0.,0.,-12.278617978381));
#63822=CARTESIAN_POINT('',(-0.676704782873988,0.000128481712317595,-6.17861797838101));
#63823=CARTESIAN_POINT('',(-0.676556184750891,-0.000492135516488926,-6.139182021619));
#63824=CARTESIAN_POINT('',(-0.6767,6.12423655037739E-13,-12.278617978381));
#63825=CARTESIAN_POINT('Ctrl Pts',(-0.676704782873988,0.000128481712317646,
-6.17861797838101));
#63826=CARTESIAN_POINT('Ctrl Pts',(-0.676580798701789,-0.0338241820643936,
-6.17702463342863));
#63827=CARTESIAN_POINT('Ctrl Pts',(-0.665162410638196,-0.180638294760152,
-6.17013575564478));
#63828=CARTESIAN_POINT('Ctrl Pts',(-0.562221864267348,-0.426947701728367,
-6.15795134502947));
#63829=CARTESIAN_POINT('Ctrl Pts',(-0.289550464019102,-0.642148606418798,
-6.14206474653509));
#63830=CARTESIAN_POINT('Ctrl Pts',(0.169783162631269,-0.726713697646756,
-6.1208826152092));
#63831=CARTESIAN_POINT('Ctrl Pts',(0.595024636138863,-0.450700878954778,
-6.09970048388339));
#63832=CARTESIAN_POINT('Ctrl Pts',(0.70362826836473,0.00253654546368757,
-6.07851835255749));
#63833=CARTESIAN_POINT('Ctrl Pts',(0.592641591588357,0.453327123043412,
-6.05733622123166));
#63834=CARTESIAN_POINT('Ctrl Pts',(0.0569329064749938,0.798344967018745,
-6.03085855707431));
#63835=CARTESIAN_POINT('Ctrl Pts',(-0.557831024569953,0.517353749803968,
-6.0028539651803));
#63836=CARTESIAN_POINT('Ctrl Pts',(-0.675108709321502,0.144863449673475,
-5.98544043894919));
#63837=CARTESIAN_POINT('Ctrl Pts',(-0.675992408981733,-0.000518565907705555,
-5.97861797838101));
#63838=CARTESIAN_POINT('Ctrl Pts',(-0.676556184750892,-0.000492135516488929,
-6.139182021619));
#63839=CARTESIAN_POINT('Ctrl Pts',(-0.676915433003454,-0.0750118267480244,
-6.13568155603213));
#63840=CARTESIAN_POINT('Ctrl Pts',(-0.629822248076123,-0.374271290200019,
-6.12159002478234));
#63841=CARTESIAN_POINT('Ctrl Pts',(-0.192973643036106,-0.776760719460778,
-6.09690742786962));
#63842=CARTESIAN_POINT('Ctrl Pts',(0.548852666849259,-0.58226923395591,
-6.06513423088083));
#63843=CARTESIAN_POINT('Ctrl Pts',(0.786505655010167,0.145511346935457,
-6.03336103389204));
#63844=CARTESIAN_POINT('Ctrl Pts',(0.303954112232331,0.739849035349103,
-6.00158783690326));
#63845=CARTESIAN_POINT('Ctrl Pts',(-0.448015488347003,0.657740779645327,
-5.97019483281224));
#63846=CARTESIAN_POINT('Ctrl Pts',(-0.67730617551369,0.215660852461966,
-5.94939289438415));
#63847=CARTESIAN_POINT('Ctrl Pts',(-0.677862131410808,-0.000317623256960531,
-5.939182021619));
#63848=CARTESIAN_POINT('Origin',(0.,0.,-12.278617978381));
#63849=CARTESIAN_POINT('',(-0.6767,1.4656678648528E-13,-6.37861797838101));
#63850=CARTESIAN_POINT('',(-0.675457068551241,0.00029468390945811,-6.339182021619));
#63851=CARTESIAN_POINT('',(-0.6767,6.12423655037739E-13,-12.278617978381));
#63852=CARTESIAN_POINT('Ctrl Pts',(-0.676875242892834,9.14395672268094E-5,
-6.37861797838101));
#63853=CARTESIAN_POINT('Ctrl Pts',(-0.67674179299303,-0.0997811966725849,
-6.37390436073954));
#63854=CARTESIAN_POINT('Ctrl Pts',(-0.628299285756436,-0.311940683515031,
-6.3638952102666));
#63855=CARTESIAN_POINT('Ctrl Pts',(-0.340972135963656,-0.663797545482861,
-6.34329499413074));
#63856=CARTESIAN_POINT('Ctrl Pts',(0.161643869936548,-0.728723180265365,
-6.32211286280486));
#63857=CARTESIAN_POINT('Ctrl Pts',(0.538076797651925,-0.453547551601197,
-6.30093073147902));
#63858=CARTESIAN_POINT('Ctrl Pts',(0.744851349578635,-0.038160346185337,
-6.27974860015315));
#63859=CARTESIAN_POINT('Ctrl Pts',(0.560874095982173,0.57170878506611,-6.25327093599583));
#63860=CARTESIAN_POINT('Ctrl Pts',(-0.178950953192254,0.780037574273926,
-6.22149773900705));
#63861=CARTESIAN_POINT('Ctrl Pts',(-0.625642030755787,0.383504116506336,
-6.1966134198021));
#63862=CARTESIAN_POINT('Ctrl Pts',(-0.676992864057429,0.079018580249279,
-6.18232016626009));
#63863=CARTESIAN_POINT('Ctrl Pts',(-0.676704782873988,0.000128481712317646,
-6.17861797838101));
#63864=CARTESIAN_POINT('Ctrl Pts',(-0.675457068551241,0.000294683909458103,
-6.339182021619));
#63865=CARTESIAN_POINT('Ctrl Pts',(-0.674863684696936,-0.140825266627321,
-6.33256128334304));
#63866=CARTESIAN_POINT('Ctrl Pts',(-0.563978321160066,-0.508573136181875,
-6.31534947940416));
#63867=CARTESIAN_POINT('Ctrl Pts',(0.042556028366106,-0.799168971730803,
-6.28754660980234));
#63868=CARTESIAN_POINT('Ctrl Pts',(0.58315304606446,-0.46498710724797,-6.26106894564502));
#63869=CARTESIAN_POINT('Ctrl Pts',(0.704267131783399,-0.0151800071787377,
-6.23988681431916));
#63870=CARTESIAN_POINT('Ctrl Pts',(0.627100262560229,0.324226811612303,
-6.22400021582477));
#63871=CARTESIAN_POINT('Ctrl Pts',(0.395365052280528,0.582992949678207,
-6.20811361733038));
#63872=CARTESIAN_POINT('Ctrl Pts',(-0.0426668885056882,0.745062854587275,
-6.18693148600451));
#63873=CARTESIAN_POINT('Ctrl Pts',(-0.508936057342763,0.546049163939659,
-6.16574935467866));
#63874=CARTESIAN_POINT('Ctrl Pts',(-0.663119369583067,0.188858374715681,
-6.14806768893966));
#63875=CARTESIAN_POINT('Ctrl Pts',(-0.676371959322915,0.0377221686919021,
-6.1409770888636));
#63876=CARTESIAN_POINT('Ctrl Pts',(-0.676556184750892,-0.000492135516488929,
-6.139182021619));
#63877=CARTESIAN_POINT('Origin',(0.,0.,-12.278617978381));
#63878=CARTESIAN_POINT('',(-0.6767,1.31976383050954E-13,-6.57861797838101));
#63879=CARTESIAN_POINT('',(-0.677816872487775,0.000601865446929958,-6.539182021619));
#63880=CARTESIAN_POINT('',(-0.6767,6.12423655037739E-13,-12.278617978381));
#63881=CARTESIAN_POINT('Ctrl Pts',(-0.6767,1.31976383050954E-13,-6.57861797838101));
#63882=CARTESIAN_POINT('Ctrl Pts',(-0.676700000000005,-0.0225339661634695,
-6.57755801322587));
#63883=CARTESIAN_POINT('Ctrl Pts',(-0.675570903631601,-0.0451197667652925,
-6.57649560808497));
#63884=CARTESIAN_POINT('Ctrl Pts',(-0.673318349535998,-0.0675669310988747,
-6.57543442293695));
#63885=CARTESIAN_POINT('Ctrl Pts',(-0.653765277554997,-0.262417310426306,
-6.56622291071404));
#63886=CARTESIAN_POINT('Ctrl Pts',(-0.544888756309662,-0.446506580237345,
-6.55701139849113));
#63887=CARTESIAN_POINT('Ctrl Pts',(-0.383554086245299,-0.557502603513682,
-6.54779988626823));
#63888=CARTESIAN_POINT('Ctrl Pts',(-0.222219416180937,-0.668498626790019,
-6.53858837404532));
#63889=CARTESIAN_POINT('Ctrl Pts',(-0.0113736801396104,-0.704373851266513,
-6.52937686182241));
#63890=CARTESIAN_POINT('Ctrl Pts',(0.177591316576043,-0.652981021375651,
-6.52016534959951));
#63891=CARTESIAN_POINT('Ctrl Pts',(0.366556313291696,-0.601588191484788,
-6.5109538373766));
#63892=CARTESIAN_POINT('Ctrl Pts',(0.530188767672756,-0.463866094451386,
-6.50174232515369));
#63893=CARTESIAN_POINT('Ctrl Pts',(0.613083165983457,-0.286447065943606,
-6.49253081293079));
#63894=CARTESIAN_POINT('Ctrl Pts',(0.695977564294159,-0.109028037435825,
-6.48331930070788));
#63895=CARTESIAN_POINT('Ctrl Pts',(0.696619683591181,0.104847028480835,
-6.47410778848497));
#63896=CARTESIAN_POINT('Ctrl Pts',(0.614792103988806,0.282760603466992,
-6.46489627626207));
#63897=CARTESIAN_POINT('Ctrl Pts',(0.53296452438643,0.460674178453149,-6.45568476403916));
#63898=CARTESIAN_POINT('Ctrl Pts',(0.370161981366855,0.59937633461666,-6.44647325181625));
#63899=CARTESIAN_POINT('Ctrl Pts',(0.181508982886692,0.651902890875197,
-6.43726173959334));
#63900=CARTESIAN_POINT('Ctrl Pts',(-0.00714401559347194,0.704429447133734,
-6.42805022737044));
#63901=CARTESIAN_POINT('Ctrl Pts',(-0.218201365763082,0.669820906606433,
-6.41883871514753));
#63902=CARTESIAN_POINT('Ctrl Pts',(-0.380199610338631,0.559795629045416,
-6.40962720292462));
#63903=CARTESIAN_POINT('Ctrl Pts',(-0.542197854914179,0.4497703514844,-6.40041569070172));
#63904=CARTESIAN_POINT('Ctrl Pts',(-0.652177789610297,0.266338156648583,
-6.39120417847881));
#63905=CARTESIAN_POINT('Ctrl Pts',(-0.672900501122695,0.0716086977177066,
-6.3819926662559));
#63906=CARTESIAN_POINT('Ctrl Pts',(-0.675431127350092,0.047828630339819,
-6.3808677702976));
#63907=CARTESIAN_POINT('Ctrl Pts',(-0.676699999999995,0.0238863472897277,
-6.37974155758702));
#63908=CARTESIAN_POINT('Ctrl Pts',(-0.6767,1.46566854827417E-13,-6.37861797838101));
#63909=CARTESIAN_POINT('Ctrl Pts',(-0.677816872487775,0.000601865446929938,
-6.539182021619));
#63910=CARTESIAN_POINT('Ctrl Pts',(-0.67655614108913,-0.205703460295888,
-6.52944101065395));
#63911=CARTESIAN_POINT('Ctrl Pts',(-0.464731990145984,-0.639726014582718,
-6.50910893402597));
#63912=CARTESIAN_POINT('Ctrl Pts',(0.143458633831261,-0.731914130435804,
-6.48348132456653));
#63913=CARTESIAN_POINT('Ctrl Pts',(0.526965677843967,-0.467479525104637,
-6.46229919324067));
#63914=CARTESIAN_POINT('Ctrl Pts',(0.687844780422188,-0.158831240600472,
-6.44641259474628));
#63915=CARTESIAN_POINT('Ctrl Pts',(0.678772152266887,0.188409603808886,
-6.43052599625188));
#63916=CARTESIAN_POINT('Ctrl Pts',(0.449737145934374,0.595504557883058,
-6.40934386492603));
#63917=CARTESIAN_POINT('Ctrl Pts',(-0.0343035843211689,0.745647019873919,
-6.38816173360018));
#63918=CARTESIAN_POINT('Ctrl Pts',(-0.452343460848582,0.539089431506795,
-6.36697960227431));
#63919=CARTESIAN_POINT('Ctrl Pts',(-0.641343804359365,0.282137405713559,
-6.35241820922441));
#63920=CARTESIAN_POINT('Ctrl Pts',(-0.675812909255033,0.0849215610206185,
-6.34315234900597));
#63921=CARTESIAN_POINT('Ctrl Pts',(-0.675457068551241,0.000294683909458103,
-6.339182021619));
#63922=CARTESIAN_POINT('Origin',(0.,0.,-12.278617978381));
#63923=CARTESIAN_POINT('',(-0.676558247700131,-7.87320039269999E-6,-6.77861797838101));
#63924=CARTESIAN_POINT('',(-0.676709423551057,-8.49736032138343E-5,-6.739182021619));
#63925=CARTESIAN_POINT('',(-0.6767,6.12423655037739E-13,-12.278617978381));
#63926=CARTESIAN_POINT('Ctrl Pts',(-0.6767,1.17385911274492E-13,-6.77861797838101));
#63927=CARTESIAN_POINT('Ctrl Pts',(-0.676700000000012,-0.0689923121809674,
-6.77537267986794));
#63928=CARTESIAN_POINT('Ctrl Pts',(-0.666054446306332,-0.138058240211869,
-6.77212344587233));
#63929=CARTESIAN_POINT('Ctrl Pts',(-0.645254990554443,-0.203884494664468,
-6.76887617961799));
#63930=CARTESIAN_POINT('Ctrl Pts',(-0.586253225413585,-0.390613669295004,
-6.75966466739508));
#63931=CARTESIAN_POINT('Ctrl Pts',(-0.442018685279904,-0.548535655004635,
-6.75045315517218));
#63932=CARTESIAN_POINT('Ctrl Pts',(-0.261388801730013,-0.624178487557964,
-6.74124164294927));
#63933=CARTESIAN_POINT('Ctrl Pts',(-0.0807589181801233,-0.699821320111294,
-6.73203013072636));
#63934=CARTESIAN_POINT('Ctrl Pts',(0.132966762381217,-0.691803240126696,
-6.72281861850346));
#63935=CARTESIAN_POINT('Ctrl Pts',(0.30742129309852,-0.602839148156151,
-6.71360710628055));
#63936=CARTESIAN_POINT('Ctrl Pts',(0.481875823815823,-0.513875056185606,
-6.70439559405764));
#63937=CARTESIAN_POINT('Ctrl Pts',(0.613872462781772,-0.345590049605281,
-6.69518408183474));
#63938=CARTESIAN_POINT('Ctrl Pts',(0.658717499198191,-0.154964983948248,
-6.68597256961183));
#63939=CARTESIAN_POINT('Ctrl Pts',(0.703562535614611,0.0356600817087843,
-6.67676105738892));
#63940=CARTESIAN_POINT('Ctrl Pts',(0.660436790086757,0.245143079135101,
-6.66754954516601));
#63941=CARTESIAN_POINT('Ctrl Pts',(0.543942525321295,0.402553622697762,
-6.65833803294311));
#63942=CARTESIAN_POINT('Ctrl Pts',(0.427448260555833,0.559964166260423,
-6.6491265207202));
#63943=CARTESIAN_POINT('Ctrl Pts',(0.239713464596202,0.662426854708672,
-6.63991500849729));
#63944=CARTESIAN_POINT('Ctrl Pts',(0.0443046399162912,0.675248094319331,
-6.63070349627439));
#63945=CARTESIAN_POINT('Ctrl Pts',(-0.151104184763619,0.68806933392999,
-6.62149198405148));
#63946=CARTESIAN_POINT('Ctrl Pts',(-0.350617526451464,0.611014920515853,
-6.61228047182857));
#63947=CARTESIAN_POINT('Ctrl Pts',(-0.486680698424695,0.470175273468152,
-6.60306895960567));
#63948=CARTESIAN_POINT('Ctrl Pts',(-0.607069113224888,0.345560643343055,
-6.59491863253078));
#63949=CARTESIAN_POINT('Ctrl Pts',(-0.676699999999966,0.173069887823577,
-6.58675893542178));
#63950=CARTESIAN_POINT('Ctrl Pts',(-0.6767,1.31976383050954E-13,-6.57861797838101));
#63951=CARTESIAN_POINT('Ctrl Pts',(-0.676804323507533,-0.000940701036842954,
-6.73918202161899));
#63952=CARTESIAN_POINT('Ctrl Pts',(-0.6772597637176,-0.0492104853983123,
-6.73691180362778));
#63953=CARTESIAN_POINT('Ctrl Pts',(-0.650606445369866,-0.322003920915775,
-6.72405051997364));
#63954=CARTESIAN_POINT('Ctrl Pts',(-0.36446354353643,-0.650726522050533,
-6.70589370348805));
#63955=CARTESIAN_POINT('Ctrl Pts',(0.0990244122389695,-0.697441110221215,
-6.68471157216218));
#63956=CARTESIAN_POINT('Ctrl Pts',(0.421449152886381,-0.566337695957096,
-6.6688249736678));
#63957=CARTESIAN_POINT('Ctrl Pts',(0.639321376606824,-0.295800731727484,
-6.6529383751734));
#63958=CARTESIAN_POINT('Ctrl Pts',(0.72828669883045,0.162749683301894,-6.63175624384754));
#63959=CARTESIAN_POINT('Ctrl Pts',(0.456550800284682,0.590531801388853,
-6.61057411252168));
#63960=CARTESIAN_POINT('Ctrl Pts',(0.00420849966872835,0.703714670097329,
-6.58939198119583));
#63961=CARTESIAN_POINT('Ctrl Pts',(-0.447311932305929,0.59680068373128,
-6.56820984986996));
#63962=CARTESIAN_POINT('Ctrl Pts',(-0.66913515988933,0.260749856922413,
-6.55147319667769));
#63963=CARTESIAN_POINT('Ctrl Pts',(-0.67792689090907,0.0186052135567966,
-6.54003207631688));
#63964=CARTESIAN_POINT('Ctrl Pts',(-0.677816872487775,0.000601865446929938,
-6.539182021619));
#63965=CARTESIAN_POINT('Origin',(0.,0.,-12.278617978381));
#63966=CARTESIAN_POINT('',(-0.677117923044813,0.000572801869896454,-6.97861797838101));
#63967=CARTESIAN_POINT('',(-0.676424852156372,7.29842916120558E-5,-6.939182021619));
#63968=CARTESIAN_POINT('',(-0.6767,6.12423655037739E-13,-12.278617978381));
#63969=CARTESIAN_POINT('Ctrl Pts',(-0.677117923044813,0.000572801869896465,
-6.978617978381));
#63970=CARTESIAN_POINT('Ctrl Pts',(-0.676704078716193,-0.0735018107475405,
-6.97513460833519));
#63971=CARTESIAN_POINT('Ctrl Pts',(-0.64466818210056,-0.260791847049063,
-6.9663557054579));
#63972=CARTESIAN_POINT('Ctrl Pts',(-0.416626705641162,-0.618612325309093,
-6.9469857369177));
#63973=CARTESIAN_POINT('Ctrl Pts',(0.200815735222948,-0.77531043778035,
-6.92050807276037));
#63974=CARTESIAN_POINT('Ctrl Pts',(0.760672052637908,-0.248711886132582,
-6.88873487577159));
#63975=CARTESIAN_POINT('Ctrl Pts',(0.644101608620266,0.376047601873901,
-6.86225721161426));
#63976=CARTESIAN_POINT('Ctrl Pts',(0.268310163838186,0.651336773415186,
-6.8410750802884));
#63977=CARTESIAN_POINT('Ctrl Pts',(-0.07606725508181,0.701834415681397,
-6.825188481794));
#63978=CARTESIAN_POINT('Ctrl Pts',(-0.401035133744832,0.579137908513486,
-6.80930188329962));
#63979=CARTESIAN_POINT('Ctrl Pts',(-0.627635862151523,0.322555973188607,
-6.79377838216195));
#63980=CARTESIAN_POINT('Ctrl Pts',(-0.675440530384168,0.104886329948958,
-6.78355041385574));
#63981=CARTESIAN_POINT('Ctrl Pts',(-0.675270388616731,-7.94034175511452E-5,
-6.778617978381));
#63982=CARTESIAN_POINT('Ctrl Pts',(-0.6767,1.14437373471389E-13,-6.939182021619));
#63983=CARTESIAN_POINT('Ctrl Pts',(-0.676700000000005,-0.0318401568288711,
-6.93768430672372));
#63984=CARTESIAN_POINT('Ctrl Pts',(-0.674443556279103,-0.063757730454072,
-6.93618294029321));
#63985=CARTESIAN_POINT('Ctrl Pts',(-0.669953136301276,-0.095318860463623,
-6.93468339963031));
#63986=CARTESIAN_POINT('Ctrl Pts',(-0.642368983676898,-0.289195386819788,
-6.92547188740741));
#63987=CARTESIAN_POINT('Ctrl Pts',(-0.525982060165414,-0.468630723845636,
-6.9162603751845));
#63988=CARTESIAN_POINT('Ctrl Pts',(-0.36020066843924,-0.572868543782886,
-6.90704886296159));
#63989=CARTESIAN_POINT('Ctrl Pts',(-0.194419276713066,-0.677106363720137,
-6.89783735073869));
#63990=CARTESIAN_POINT('Ctrl Pts',(0.0177282726055708,-0.704242565667796,
-6.88862583851578));
#63991=CARTESIAN_POINT('Ctrl Pts',(0.204409383701599,-0.645088903837861,
-6.87941432629287));
#63992=CARTESIAN_POINT('Ctrl Pts',(0.391090494797627,-0.585935242007925,
-6.87020281406997));
#63993=CARTESIAN_POINT('Ctrl Pts',(0.548895084151931,-0.441572269896767,
-6.86099130184706));
#63994=CARTESIAN_POINT('Ctrl Pts',(0.624390937622713,-0.260880905806902,
-6.85177978962415));
#63995=CARTESIAN_POINT('Ctrl Pts',(0.699886791093495,-0.0801895417170372,
-6.84256827740125));
#63996=CARTESIAN_POINT('Ctrl Pts',(0.691694834150018,0.13352954488845,-6.83335676517834));
#63997=CARTESIAN_POINT('Ctrl Pts',(0.602588841619969,0.307911639849981,
-6.82414525295543));
#63998=CARTESIAN_POINT('Ctrl Pts',(0.513482849089919,0.482293734811513,
-6.81493374073253));
#63999=CARTESIAN_POINT('Ctrl Pts',(0.345090510431523,0.614153419397832,
-6.80572222850962));
#64000=CARTESIAN_POINT('Ctrl Pts',(0.15442902353395,0.658843355199361,-6.79651071628671));
#64001=CARTESIAN_POINT('Ctrl Pts',(-0.0362324633636222,0.703533291000889,
-6.7872992040638));
#64002=CARTESIAN_POINT('Ctrl Pts',(-0.245680305890116,0.660237131828919,
-6.7780876918409));
#64003=CARTESIAN_POINT('Ctrl Pts',(-0.402996021768146,0.543614841996655,
-6.76887617961799));
#64004=CARTESIAN_POINT('Ctrl Pts',(-0.560311737646177,0.42699255216439,
-6.75966466739508));
#64005=CARTESIAN_POINT('Ctrl Pts',(-0.662621657831973,0.239174458335219,
-6.75045315517218));
#64006=CARTESIAN_POINT('Ctrl Pts',(-0.675283915529609,0.0437552674200567,
-6.74124164294927));
#64007=CARTESIAN_POINT('Ctrl Pts',(-0.676227642444813,0.0291905385527463,
-6.74055510250584));
#64008=CARTESIAN_POINT('Ctrl Pts',(-0.676699999999997,0.0145816535338437,
-6.73986792149733));
#64009=CARTESIAN_POINT('Ctrl Pts',(-0.6767,1.29027845247851E-13,-6.739182021619));
#64010=CARTESIAN_POINT('Origin',(0.,0.,-12.278617978381));
#64011=CARTESIAN_POINT('',(-0.677341240022379,-0.00028442510368357,-7.17861797838101));
#64012=CARTESIAN_POINT('',(-0.677180734722105,0.000258105871726116,-7.13918202161899));
#64013=CARTESIAN_POINT('',(-0.6767,6.12423655037739E-13,-12.278617978381));
#64014=CARTESIAN_POINT('Ctrl Pts',(-0.677341240022379,-0.000284425103683573,
-7.17861797838101));
#64015=CARTESIAN_POINT('Ctrl Pts',(-0.677448645608267,-0.0280058869623878,
-7.17730986847756));
#64016=CARTESIAN_POINT('Ctrl Pts',(-0.662413805830168,-0.279976094954333,
-7.16541069291119));
#64017=CARTESIAN_POINT('Ctrl Pts',(-0.348839181256874,-0.720933048253655,
-7.14292045168188));
#64018=CARTESIAN_POINT('Ctrl Pts',(0.418773010672415,-0.681988811858619,
-7.1111472546931));
#64019=CARTESIAN_POINT('Ctrl Pts',(0.7343636570957,-0.130340708297302,-7.08466959053577));
#64020=CARTESIAN_POINT('Ctrl Pts',(0.626147981225155,0.322751672388126,
-7.06348745920991));
#64021=CARTESIAN_POINT('Ctrl Pts',(0.396356446240715,0.58417406811166,-7.04760086071553));
#64022=CARTESIAN_POINT('Ctrl Pts',(0.069241032314998,0.70102466077804,-7.03171426222112));
#64023=CARTESIAN_POINT('Ctrl Pts',(-0.393074702260597,0.634335284449263,
-7.01053213089527));
#64024=CARTESIAN_POINT('Ctrl Pts',(-0.656026752865113,0.302421633265633,
-6.99283336961523));
#64025=CARTESIAN_POINT('Ctrl Pts',(-0.677333218371325,0.0391088329492429,
-6.98043014116665));
#64026=CARTESIAN_POINT('Ctrl Pts',(-0.677117923044813,0.000572801869896465,
-6.978617978381));
#64027=CARTESIAN_POINT('Ctrl Pts',(-0.677180734722105,0.000258105871726134,
-7.13918202161899));
#64028=CARTESIAN_POINT('Ctrl Pts',(-0.676883705358868,-0.0681365544791201,
-7.13596679108107));
#64029=CARTESIAN_POINT('Ctrl Pts',(-0.648438885871331,-0.249497900513073,
-7.12745602771168));
#64030=CARTESIAN_POINT('Ctrl Pts',(-0.49064907573534,-0.507564044048387,
-7.11364973151081));
#64031=CARTESIAN_POINT('Ctrl Pts',(-0.188413006671554,-0.678771268169181,
-7.09776313301643));
#64032=CARTESIAN_POINT('Ctrl Pts',(0.278490899227765,-0.692337918723144,
-7.07658100169056));
#64033=CARTESIAN_POINT('Ctrl Pts',(0.656645685556425,-0.354940679903258,
-7.05539887036471));
#64034=CARTESIAN_POINT('Ctrl Pts',(0.695115409901483,0.109757071136956,
-7.03421673903885));
#64035=CARTESIAN_POINT('Ctrl Pts',(0.516523923338716,0.538016781798218,
-7.01303460771299));
#64036=CARTESIAN_POINT('Ctrl Pts',(-0.0649075310191635,0.798260763698985,
-6.98655694355567));
#64037=CARTESIAN_POINT('Ctrl Pts',(-0.597869132640885,0.447184752523441,
-6.96017423724718));
#64038=CARTESIAN_POINT('Ctrl Pts',(-0.675617621543642,0.111143512104154,
-6.94438259660162));
#64039=CARTESIAN_POINT('Ctrl Pts',(-0.675400146481493,0.000344792410071813,
-6.939182021619));
#64040=CARTESIAN_POINT('Origin',(0.,0.,-12.278617978381));
#64041=CARTESIAN_POINT('',(-0.675588369597491,-0.000390811426926173,-7.37861797838101));
#64042=CARTESIAN_POINT('',(-0.676774544010776,-0.000254207991752908,-7.339182021619));
#64043=CARTESIAN_POINT('',(-0.6767,6.12423655037739E-13,-12.278617978381));
#64044=CARTESIAN_POINT('Ctrl Pts',(-0.675588369597491,-0.000390811426926201,
-7.37861797838101));
#64045=CARTESIAN_POINT('Ctrl Pts',(-0.676146181321002,-0.0947607935846297,
-7.37418959578847));
#64046=CARTESIAN_POINT('Ctrl Pts',(-0.614211218569264,-0.414290428991899,
-7.35917014753301));
#64047=CARTESIAN_POINT('Ctrl Pts',(-0.122302166900868,-0.790899332367473,
-7.3335596336146));
#64048=CARTESIAN_POINT('Ctrl Pts',(0.475348861974375,-0.574736583594672,
-7.30708196945728));
#64049=CARTESIAN_POINT('Ctrl Pts',(0.686178318089926,-0.159340052105395,
-7.28589983813143));
#64050=CARTESIAN_POINT('Ctrl Pts',(0.680265741730897,0.18866980404402,-7.27001323963702));
#64051=CARTESIAN_POINT('Ctrl Pts',(0.50658489163482,0.489491208442347,-7.25412664114265));
#64052=CARTESIAN_POINT('Ctrl Pts',(0.111040555138311,0.737942389193872,
-7.23294450981677));
#64053=CARTESIAN_POINT('Ctrl Pts',(-0.385978182755204,0.638895363144113,
-7.21176237849093));
#64054=CARTESIAN_POINT('Ctrl Pts',(-0.638174968181164,0.281410096762473,
-7.1918883570685));
#64055=CARTESIAN_POINT('Ctrl Pts',(-0.677013842840659,0.0842170317865397,
-7.18260540130902));
#64056=CARTESIAN_POINT('Ctrl Pts',(-0.677341240022379,-0.000284425103683573,
-7.17861797838101));
#64057=CARTESIAN_POINT('Ctrl Pts',(-0.676774544010776,-0.00025420799175294,
-7.339182021619));
#64058=CARTESIAN_POINT('Ctrl Pts',(-0.676830719503838,-0.0223091699601035,
-7.33814205122344));
#64059=CARTESIAN_POINT('Ctrl Pts',(-0.670522348189875,-0.156602863542262,
-7.33180654799642));
#64060=CARTESIAN_POINT('Ctrl Pts',(-0.583010888431519,-0.39538361061797,
-7.32017551193793));
#64061=CARTESIAN_POINT('Ctrl Pts',(-0.235923423345702,-0.707975361839259,
-7.29899338061208));
#64062=CARTESIAN_POINT('Ctrl Pts',(0.270717601992387,-0.695613702123204,
-7.27781124928622));
#64063=CARTESIAN_POINT('Ctrl Pts',(0.600862087662645,-0.366328813167557,
-7.25662911796036));
#64064=CARTESIAN_POINT('Ctrl Pts',(0.741976258067605,0.0756984368513641,
-7.23544698663451));
#64065=CARTESIAN_POINT('Ctrl Pts',(0.467284115457725,0.650445070613317,
-7.20896932247717));
#64066=CARTESIAN_POINT('Ctrl Pts',(-0.295637994600642,0.743691972604572,
-7.1771961254884));
#64067=CARTESIAN_POINT('Ctrl Pts',(-0.651899538900863,0.313748973069414,
-7.15393369186899));
#64068=CARTESIAN_POINT('Ctrl Pts',(-0.677372917166972,0.0445104750611548,
-7.14126232391253));
#64069=CARTESIAN_POINT('Ctrl Pts',(-0.677180734722105,0.000258105871726134,
-7.13918202161899));
#64070=CARTESIAN_POINT('Origin',(0.,0.,-12.278617978381));
#64071=CARTESIAN_POINT('',(-0.676392201347069,0.0008047333580961,-7.578617978381));
#64072=CARTESIAN_POINT('',(-0.6767,7.06659665679343E-14,-7.53918202161899));
#64073=CARTESIAN_POINT('',(-0.6767,6.12423655037739E-13,-12.278617978381));
#64074=CARTESIAN_POINT('Ctrl Pts',(-0.676392201347069,0.000804733358096152,
-7.578617978381));
#64075=CARTESIAN_POINT('Ctrl Pts',(-0.674918865337116,-0.160046296534286,
-7.57106932309937));
#64076=CARTESIAN_POINT('Ctrl Pts',(-0.536787257819588,-0.549167815545202,
-7.55292960215482));
#64077=CARTESIAN_POINT('Ctrl Pts',(-0.00975058277995205,-0.745777183371727,
-7.5294943483788));
#64078=CARTESIAN_POINT('Ctrl Pts',(0.419849643624006,-0.565646721170082,
-7.50831221705293));
#64079=CARTESIAN_POINT('Ctrl Pts',(0.640628155804832,-0.296569284182963,
-7.49242561855854));
#64080=CARTESIAN_POINT('Ctrl Pts',(0.702987671893402,0.0451467467366845,
-7.47653902006416));
#64081=CARTESIAN_POINT('Ctrl Pts',(0.562342884997569,0.490570539624217,
-7.45535688873828));
#64082=CARTESIAN_POINT('Ctrl Pts',(0.119401435125199,0.736824090200709,
-7.43417475741245));
#64083=CARTESIAN_POINT('Ctrl Pts',(-0.332123683053873,0.620423973506661,
-7.41299262608657));
#64084=CARTESIAN_POINT('Ctrl Pts',(-0.605606017960123,0.375687041846724,
-7.39623887735325));
#64085=CARTESIAN_POINT('Ctrl Pts',(-0.674812100430787,0.130937563943502,
-7.3847806614514));
#64086=CARTESIAN_POINT('Ctrl Pts',(-0.675588369597491,-0.000390811426926201,
-7.37861797838101));
#64087=CARTESIAN_POINT('Ctrl Pts',(-0.676577157036262,2.11996792289677E-5,
-7.53918202161899));
#64088=CARTESIAN_POINT('Ctrl Pts',(-0.676832809338945,-0.0887511003222832,
-7.53502177853434));
#64089=CARTESIAN_POINT('Ctrl Pts',(-0.617002632935423,-0.403960088726185,
-7.52027046978677));
#64090=CARTESIAN_POINT('Ctrl Pts',(-0.243968745432271,-0.705440071063631,
-7.50022362820774));
#64091=CARTESIAN_POINT('Ctrl Pts',(0.22082772031363,-0.66818198545617,-7.47904149688187));
#64092=CARTESIAN_POINT('Ctrl Pts',(0.614531056354557,-0.422623475038358,
-7.45785936555602));
#64093=CARTESIAN_POINT('Ctrl Pts',(0.777226853872599,0.193265755020321,
-7.43138170139868));
#64094=CARTESIAN_POINT('Ctrl Pts',(0.256098235933003,0.758217163825756,
-7.39960850440991));
#64095=CARTESIAN_POINT('Ctrl Pts',(-0.369765439283066,0.64772849328574,
-7.37313084025257));
#64096=CARTESIAN_POINT('Ctrl Pts',(-0.635001886562817,0.292949972624209,
-7.35298867932228));
#64097=CARTESIAN_POINT('Ctrl Pts',(-0.67654467369993,0.0899947722476126,
-7.34343758405491));
#64098=CARTESIAN_POINT('Ctrl Pts',(-0.676774544010776,-0.00025420799175294,
-7.339182021619));
#64099=CARTESIAN_POINT('Origin',(0.,0.,-12.278617978381));
#64100=CARTESIAN_POINT('',(-0.677890574183207,-0.000373347607181736,-7.778617978381));
#64101=CARTESIAN_POINT('',(-0.67644239189479,4.75998292377457E-5,-7.73918202161899));
#64102=CARTESIAN_POINT('',(-0.6767,6.12423655037739E-13,-12.278617978381));
#64103=CARTESIAN_POINT('Ctrl Pts',(-0.677890574183207,-0.00037334760718182,
-7.778617978381));
#64104=CARTESIAN_POINT('Ctrl Pts',(-0.677891800033195,-0.00201980826256494,
-7.77854011607321));
#64105=CARTESIAN_POINT('Ctrl Pts',(-0.677156403482296,-0.227613571077705,
-7.76787118810249));
#64106=CARTESIAN_POINT('Ctrl Pts',(-0.490212471272208,-0.562112456819458,
-7.75190672730032));
#64107=CARTESIAN_POINT('Ctrl Pts',(-0.0461672328563757,-0.702921420239883,
-7.73072459597445));
#64108=CARTESIAN_POINT('Ctrl Pts',(0.296296052364626,-0.640754573673755,
-7.71483799748007));
#64109=CARTESIAN_POINT('Ctrl Pts',(0.565036603409811,-0.420670336941072,
-7.69895139898565));
#64110=CARTESIAN_POINT('Ctrl Pts',(0.746184610028158,0.00987433095006524,
-7.67776926765981));
#64111=CARTESIAN_POINT('Ctrl Pts',(0.56799153737738,0.484305746484325,-7.65658713633396));
#64112=CARTESIAN_POINT('Ctrl Pts',(0.148491341379806,0.687882525786409,
-7.63540500500808));
#64113=CARTESIAN_POINT('Ctrl Pts',(-0.315358990972195,0.675875526773047,
-7.61422287368224));
#64114=CARTESIAN_POINT('Ctrl Pts',(-0.638876986888255,0.355359411367687,
-7.59529386480653));
#64115=CARTESIAN_POINT('Ctrl Pts',(-0.67698601476212,0.0656341400444222,
-7.5816603887623));
#64116=CARTESIAN_POINT('Ctrl Pts',(-0.676392201347069,0.000804733358096152,
-7.578617978381));
#64117=CARTESIAN_POINT('Ctrl Pts',(-0.6767,5.60754863655395E-14,-7.73918202161899));
#64118=CARTESIAN_POINT('Ctrl Pts',(-0.676700000000002,-0.021921959043459,
-7.73815084439303));
#64119=CARTESIAN_POINT('Ctrl Pts',(-0.675631472587797,-0.0438938715230559,
-7.73711731588847));
#64120=CARTESIAN_POINT('Ctrl Pts',(-0.673499468305582,-0.0657370229938853,
-7.73608496302321));
#64121=CARTESIAN_POINT('Ctrl Pts',(-0.654475950121291,-0.260639815954453,
-7.7268734508003));
#64122=CARTESIAN_POINT('Ctrl Pts',(-0.54610007048813,-0.445024264462959,
-7.71766193857739));
#64123=CARTESIAN_POINT('Ctrl Pts',(-0.385067613933398,-0.556458284779407,
-7.70845042635449));
#64124=CARTESIAN_POINT('Ctrl Pts',(-0.224035157378667,-0.667892305095855,
-7.69923891413158));
#64125=CARTESIAN_POINT('Ctrl Pts',(-0.0132876862431723,-0.704340344110886,
-7.69002740190867));
#64126=CARTESIAN_POINT('Ctrl Pts',(0.175816266406146,-0.65346119277812,
-7.68081588968577));
#64127=CARTESIAN_POINT('Ctrl Pts',(0.364920219055463,-0.602582041445354,
-7.67160437746286));
#64128=CARTESIAN_POINT('Ctrl Pts',(0.528926311916782,-0.465305103679348,
-7.66239286523995));
#64129=CARTESIAN_POINT('Ctrl Pts',(0.612302518258926,-0.288111985404596,
-7.65318135301705));
#64130=CARTESIAN_POINT('Ctrl Pts',(0.695678724601069,-0.110918867129844,
-7.64396984079414));
#64131=CARTESIAN_POINT('Ctrl Pts',(0.696902020345894,0.10295366426577,-7.63475832857123));
#64132=CARTESIAN_POINT('Ctrl Pts',(0.615558200808584,0.281088938624948,
-7.62554681634833));
#64133=CARTESIAN_POINT('Ctrl Pts',(0.534214381271273,0.459224212984125,
-7.61633530412542));
#64134=CARTESIAN_POINT('Ctrl Pts',(0.371789345141617,0.598368252656427,
-7.60712379190251));
#64135=CARTESIAN_POINT('Ctrl Pts',(0.183279777547595,0.651407255979011,
-7.5979122796796));
#64136=CARTESIAN_POINT('Ctrl Pts',(-0.00522979004642629,0.704446259301594,
-7.5887007674567));
#64137=CARTESIAN_POINT('Ctrl Pts',(-0.216380405370042,0.6704113685789,-7.57948925523379));
#64138=CARTESIAN_POINT('Ctrl Pts',(-0.378677031806715,0.560826707265316,
-7.57027774301088));
#64139=CARTESIAN_POINT('Ctrl Pts',(-0.540973658243388,0.451242045951731,
-7.56106623078798));
#64140=CARTESIAN_POINT('Ctrl Pts',(-0.651451640998797,0.26810938511718,
-7.55185471856507));
#64141=CARTESIAN_POINT('Ctrl Pts',(-0.672703429020755,0.0734369565254355,
-7.54264320634216));
#64142=CARTESIAN_POINT('Ctrl Pts',(-0.675365183944437,0.0490545236320713,
-7.54148947810111));
#64143=CARTESIAN_POINT('Ctrl Pts',(-0.676699999999998,0.0244983809836534,
-7.54033439000418));
#64144=CARTESIAN_POINT('Ctrl Pts',(-0.6767,7.06659581420018E-14,-7.53918202161899));
#64145=CARTESIAN_POINT('Origin',(0.,0.,-12.278617978381));
#64146=CARTESIAN_POINT('',(-0.675799427295481,-0.000196415820169861,-7.978617978381));
#64147=CARTESIAN_POINT('',(-0.677536114604909,0.000301369397225656,-7.93918202161899));
#64148=CARTESIAN_POINT('',(-0.6767,6.12423655037739E-13,-12.278617978381));
#64149=CARTESIAN_POINT('Ctrl Pts',(-0.67579942729548,-0.000196415820169965,
-7.978617978381));
#64150=CARTESIAN_POINT('Ctrl Pts',(-0.676291431262014,-0.0682707116028679,
-7.97541984338411));
#64151=CARTESIAN_POINT('Ctrl Pts',(-0.651210353376953,-0.248880751939011,
-7.96692617555577));
#64152=CARTESIAN_POINT('Ctrl Pts',(-0.490226125422572,-0.505873781070776,
-7.95313697489597));
#64153=CARTESIAN_POINT('Ctrl Pts',(-0.188959895740458,-0.680185218989984,
-7.93725037640156));
#64154=CARTESIAN_POINT('Ctrl Pts',(0.158343748144318,-0.68640888178885,
-7.92136377790718));
#64155=CARTESIAN_POINT('Ctrl Pts',(0.57512722912829,-0.475518290888796,
-7.9001816465813));
#64156=CARTESIAN_POINT('Ctrl Pts',(0.746434431978506,0.00144269434815235,
-7.87899951525548));
#64157=CARTESIAN_POINT('Ctrl Pts',(0.558481156467344,0.428171514253297,
-7.85781738392959));
#64158=CARTESIAN_POINT('Ctrl Pts',(0.197165933085699,0.719294526399437,
-7.83663525260375));
#64159=CARTESIAN_POINT('Ctrl Pts',(-0.436112882427935,0.670670210164639,
-7.81023545075422));
#64160=CARTESIAN_POINT('Ctrl Pts',(-0.67772505622498,0.221936729982677,
-7.78913118173614));
#64161=CARTESIAN_POINT('Ctrl Pts',(-0.677890574183207,-0.00037334760718182,
-7.778617978381));
#64162=CARTESIAN_POINT('Ctrl Pts',(-0.677536114604909,0.000301369397225706,
-7.93918202161899));
#64163=CARTESIAN_POINT('Ctrl Pts',(-0.677582832650084,-0.107871171142427,
-7.93407676598763));
#64164=CARTESIAN_POINT('Ctrl Pts',(-0.620875575886241,-0.329206785654903,
-7.92367597752479));
#64165=CARTESIAN_POINT('Ctrl Pts',(-0.317576031167041,-0.674836636013439,
-7.90268412339904));
#64166=CARTESIAN_POINT('Ctrl Pts',(0.316526456894863,-0.73569303145392,
-7.87620645924171));
#64167=CARTESIAN_POINT('Ctrl Pts',(0.789672444363271,-0.129988478648325,
-7.84443326225293));
#64168=CARTESIAN_POINT('Ctrl Pts',(0.579332529080104,0.469736630306881,
-7.81795559809561));
#64169=CARTESIAN_POINT('Ctrl Pts',(0.166006120765101,0.684596161463233,
-7.79677346676974));
#64170=CARTESIAN_POINT('Ctrl Pts',(-0.182044780093774,0.68206852468891,
-7.78088686827537));
#64171=CARTESIAN_POINT('Ctrl Pts',(-0.484541134815908,0.511321605495331,
-7.76500026978095));
#64172=CARTESIAN_POINT('Ctrl Pts',(-0.650114110956395,0.253328034721966,
-7.75109865422884));
#64173=CARTESIAN_POINT('Ctrl Pts',(-0.676353652975621,0.0705349586336249,
-7.74249257150818));
#64174=CARTESIAN_POINT('Ctrl Pts',(-0.675796937800043,0.000166864340071023,
-7.73918202161899));
#64175=CARTESIAN_POINT('Origin',(0.,0.,-12.278617978381));
#64176=CARTESIAN_POINT('',(-0.676581765607971,3.46312420244521E-5,-8.178617978381));
#64177=CARTESIAN_POINT('',(-0.676757248046547,-0.000512325571017325,-8.139182021619));
#64178=CARTESIAN_POINT('',(-0.6767,6.12423655037739E-13,-12.278617978381));
#64179=CARTESIAN_POINT('Ctrl Pts',(-0.676581765607971,3.46312420244597E-5,
-8.178617978381));
#64180=CARTESIAN_POINT('Ctrl Pts',(-0.676517670152724,-0.0217651188480246,
-8.17759510352649));
#64181=CARTESIAN_POINT('Ctrl Pts',(-0.66971641899371,-0.156406801086305,
-8.17127669584052));
#64182=CARTESIAN_POINT('Ctrl Pts',(-0.584343046747153,-0.396107280984521,
-8.15966275532308));
#64183=CARTESIAN_POINT('Ctrl Pts',(-0.323660302086688,-0.625678754975878,
-8.14377615682868));
#64184=CARTESIAN_POINT('Ctrl Pts',(0.130528774517201,-0.734745679590988,
-8.12259402550284));
#64185=CARTESIAN_POINT('Ctrl Pts',(0.569859400741034,-0.482106529718409,
-8.10141189417698));
#64186=CARTESIAN_POINT('Ctrl Pts',(0.702847075744717,-0.0351857338159052,
-8.08022976285111));
#64187=CARTESIAN_POINT('Ctrl Pts',(0.615915117961009,0.420603837767584,
-8.05904763152526));
#64188=CARTESIAN_POINT('Ctrl Pts',(0.100242323565696,0.794597200479857,
-8.03256996736792));
#64189=CARTESIAN_POINT('Ctrl Pts',(-0.542739842833042,0.540862840079443,
-8.00399490537604));
#64190=CARTESIAN_POINT('Ctrl Pts',(-0.674662092187505,0.157166719054403,
-7.98601090904705));
#64191=CARTESIAN_POINT('Ctrl Pts',(-0.67579942729548,-0.000196415820169965,
-7.978617978381));
#64192=CARTESIAN_POINT('Ctrl Pts',(-0.676757248046547,-0.000512325571017335,
-8.139182021619));
#64193=CARTESIAN_POINT('Ctrl Pts',(-0.677077249127755,-0.0627978904691677,
-8.13625202613001));
#64194=CARTESIAN_POINT('Ctrl Pts',(-0.639251224563342,-0.349588008735834,
-8.12273096497808));
#64195=CARTESIAN_POINT('Ctrl Pts',(-0.234999107869971,-0.765642641017721,
-8.09861883816322));
#64196=CARTESIAN_POINT('Ctrl Pts',(0.517732728409698,-0.610272394838091,
-8.06684564117445));
#64197=CARTESIAN_POINT('Ctrl Pts',(0.745647079045141,-0.0170033706618007,
-8.04036797701711));
#64198=CARTESIAN_POINT('Ctrl Pts',(0.569703324557914,0.414328442674807,
-8.01918584569126));
#64199=CARTESIAN_POINT('Ctrl Pts',(0.302785852511827,0.637713495113113,
-8.00329924719686));
#64200=CARTESIAN_POINT('Ctrl Pts',(-0.0383075228840123,0.70339350954178,
-7.98741264870248));
#64201=CARTESIAN_POINT('Ctrl Pts',(-0.485078126151442,0.567087459025494,
-7.96623051737661));
#64202=CARTESIAN_POINT('Ctrl Pts',(-0.675241177176038,0.232736134400955,
-7.95015364168212));
#64203=CARTESIAN_POINT('Ctrl Pts',(-0.677534373383808,0.00433305157491817,
-7.93937229881909));
#64204=CARTESIAN_POINT('Ctrl Pts',(-0.677536114604909,0.000301369397225706,
-7.93918202161899));
#64205=CARTESIAN_POINT('Origin',(0.,0.,-12.278617978381));
#64206=CARTESIAN_POINT('',(-0.6767,3.91279890432639E-14,-8.378617978381));
#64207=CARTESIAN_POINT('',(-0.675338277625542,0.000119265976971927,-8.33918202161899));
#64208=CARTESIAN_POINT('',(-0.6767,6.12423655037739E-13,-12.278617978381));
#64209=CARTESIAN_POINT('Ctrl Pts',(-0.676800963596304,0.00021576680758149,
-8.378617978381));
#64210=CARTESIAN_POINT('Ctrl Pts',(-0.676608873861011,-0.0875972287274319,
-8.3744748308374));
#64211=CARTESIAN_POINT('Ctrl Pts',(-0.636733335774834,-0.287882668666046,
-8.36503615046233));
#64212=CARTESIAN_POINT('Ctrl Pts',(-0.376151562716211,-0.644514527780979,
-8.34500640442435));
#64213=CARTESIAN_POINT('Ctrl Pts',(0.122248771729135,-0.736357033252738,
-8.32382427309847));
#64214=CARTESIAN_POINT('Ctrl Pts',(0.512926016390591,-0.481808000615124,
-8.30264214177264));
#64215=CARTESIAN_POINT('Ctrl Pts',(0.741723760032622,-0.0781337614659248,
-8.28146001044675));
#64216=CARTESIAN_POINT('Ctrl Pts',(0.590788201416899,0.540742577860168,
-8.25498234628945));
#64217=CARTESIAN_POINT('Ctrl Pts',(-0.136775462740103,0.788525235335051,
-8.22320914930065));
#64218=CARTESIAN_POINT('Ctrl Pts',(-0.614839420141264,0.408047756448488,
-8.19775435999784));
#64219=CARTESIAN_POINT('Ctrl Pts',(-0.676849499199172,0.0910945255265748,
-8.18289063635796));
#64220=CARTESIAN_POINT('Ctrl Pts',(-0.676581765607971,3.46312420244597E-5,
-8.178617978381));
#64221=CARTESIAN_POINT('Ctrl Pts',(-0.675338277625542,0.000119265976971872,
-8.33918202161899));
#64222=CARTESIAN_POINT('Ctrl Pts',(-0.675125560369215,-0.12890170738665,
-8.33313175344091));
#64223=CARTESIAN_POINT('Ctrl Pts',(-0.578388002552477,-0.48415351739988,
-8.31649041959989));
#64224=CARTESIAN_POINT('Ctrl Pts',(-0.000450182530976969,-0.800299550983042,
-8.28925802009595));
#64225=CARTESIAN_POINT('Ctrl Pts',(0.55731818268824,-0.495656256237618,
-8.26278035593863));
#64226=CARTESIAN_POINT('Ctrl Pts',(0.70243916327569,-0.0530014935470479,
-8.24159822461277));
#64227=CARTESIAN_POINT('Ctrl Pts',(0.643605972302399,0.290050214182614,
-8.22571162611838));
#64228=CARTESIAN_POINT('Ctrl Pts',(0.426145850537514,0.56091854100633,-8.20982502762398));
#64229=CARTESIAN_POINT('Ctrl Pts',(-0.00261665234877711,0.746245353610373,
-8.18864289629813));
#64230=CARTESIAN_POINT('Ctrl Pts',(-0.478758691882225,0.5726749143775,-8.16746076497226));
#64231=CARTESIAN_POINT('Ctrl Pts',(-0.657683237969969,0.212924793057815,
-8.1492086291354));
#64232=CARTESIAN_POINT('Ctrl Pts',(-0.676498894574648,0.0497740418370898,
-8.14154755896147));
#64233=CARTESIAN_POINT('Ctrl Pts',(-0.676757248046547,-0.000512325571017335,
-8.139182021619));
#64234=CARTESIAN_POINT('Origin',(0.,0.,-12.278617978381));
#64235=CARTESIAN_POINT('',(-0.6767,2.45376068294393E-14,-8.578617978381));
#64236=CARTESIAN_POINT('',(-0.677509650187365,0.000766222167987149,-8.539182021619));
#64237=CARTESIAN_POINT('',(-0.6767,6.12423655037739E-13,-12.278617978381));
#64238=CARTESIAN_POINT('Ctrl Pts',(-0.6767,1.49211214436621E-14,-8.578617978381));
#64239=CARTESIAN_POINT('Ctrl Pts',(-0.676700000000002,-0.0956161613166699,
-8.57412033253705));
#64240=CARTESIAN_POINT('Ctrl Pts',(-0.65612415604488,-0.191237609808786,
-8.56962003485022));
#64241=CARTESIAN_POINT('Ctrl Pts',(-0.616773580775826,-0.278411996970255,
-8.56512106308482));
#64242=CARTESIAN_POINT('Ctrl Pts',(-0.536204436542128,-0.45689898793987,
-8.55590955086192));
#64243=CARTESIAN_POINT('Ctrl Pts',(-0.374385443722978,-0.596747369056862,
-8.54669803863901));
#64244=CARTESIAN_POINT('Ctrl Pts',(-0.186108082793701,-0.650604850519002,
-8.5374865264161));
#64245=CARTESIAN_POINT('Ctrl Pts',(0.00216927813557544,-0.704462331981142,
-8.5282750141932));
#64246=CARTESIAN_POINT('Ctrl Pts',(0.213465765134057,-0.671345105041863,
-8.51906350197029));
#64247=CARTESIAN_POINT('Ctrl Pts',(0.376236949824165,-0.562466574639782,
-8.50985198974738));
#64248=CARTESIAN_POINT('Ctrl Pts',(0.539008134514272,-0.453588044237701,
-8.50064047752448));
#64249=CARTESIAN_POINT('Ctrl Pts',(0.650280693397769,-0.270937082626308,
-8.49142896530157));
#64250=CARTESIAN_POINT('Ctrl Pts',(0.672378034059336,-0.0763588194939005,
-8.48221745307866));
#64251=CARTESIAN_POINT('Ctrl Pts',(0.694475374720904,0.118219443638507,
-8.47300594085575));
#64252=CARTESIAN_POINT('Ctrl Pts',(0.62699384744599,0.321170668356893,-8.46379442863285));
#64253=CARTESIAN_POINT('Ctrl Pts',(0.492782517846198,0.463776109890496,
-8.45458291640994));
#64254=CARTESIAN_POINT('Ctrl Pts',(0.358571188246407,0.6063815514241,-8.44537140418703));
#64255=CARTESIAN_POINT('Ctrl Pts',(0.160081680058386,0.686036251708044,
-8.43615989196413));
#64256=CARTESIAN_POINT('Ctrl Pts',(-0.0354779872946126,0.675769341134624,
-8.42694837974122));
#64257=CARTESIAN_POINT('Ctrl Pts',(-0.231037654647611,0.665502430561203,
-8.41773686751831));
#64258=CARTESIAN_POINT('Ctrl Pts',(-0.420095214026566,0.565501453667373,
-8.40852535529541));
#64259=CARTESIAN_POINT('Ctrl Pts',(-0.538636278782801,0.409626475192969,
-8.3993138430725));
#64260=CARTESIAN_POINT('Ctrl Pts',(-0.627413227207555,0.292889672185607,
-8.39241522150867));
#64261=CARTESIAN_POINT('Ctrl Pts',(-0.676699999999992,0.146509960619025,
-8.38550959488601));
#64262=CARTESIAN_POINT('Ctrl Pts',(-0.6767,3.91280786059017E-14,-8.378617978381));
#64263=CARTESIAN_POINT('Ctrl Pts',(-0.677509650187365,0.000766222167987083,
-8.539182021619));
#64264=CARTESIAN_POINT('Ctrl Pts',(-0.675844325969005,-0.193734978521912,
-8.53001148075182));
#64265=CARTESIAN_POINT('Ctrl Pts',(-0.485030615819685,-0.6166037500008,
-8.5102498742217));
#64266=CARTESIAN_POINT('Ctrl Pts',(0.10391852221122,-0.738565922476695,
-8.48519273486015));
#64267=CARTESIAN_POINT('Ctrl Pts',(0.501082034024498,-0.495122945943268,
-8.46401060353428));
#64268=CARTESIAN_POINT('Ctrl Pts',(0.678315270358112,-0.195566276054168,
-8.44812400503989));
#64269=CARTESIAN_POINT('Ctrl Pts',(0.687916430292161,0.151660411805788,
-8.43223740654549));
#64270=CARTESIAN_POINT('Ctrl Pts',(0.481089349371821,0.570475251501399,
-8.41105527521963));
#64271=CARTESIAN_POINT('Ctrl Pts',(0.00581701517587562,0.746413159680681,
-8.38987314389378));
#64272=CARTESIAN_POINT('Ctrl Pts',(-0.422719610264708,0.562619035266954,
-8.36869101256792));
#64273=CARTESIAN_POINT('Ctrl Pts',(-0.63318944003504,0.306541419473106,
-8.35355914942015));
#64274=CARTESIAN_POINT('Ctrl Pts',(-0.675497924430293,0.096951025181312,
-8.34372281910384));
#64275=CARTESIAN_POINT('Ctrl Pts',(-0.675338277625542,0.000119265976971872,
-8.33918202161899));
#64276=CARTESIAN_POINT('Origin',(0.,0.,-12.278617978381));
#64277=CARTESIAN_POINT('',(-0.6767,2.91801058245312E-14,-8.778617978381));
#64278=CARTESIAN_POINT('',(-0.67719182899154,-0.000898131385783873,-8.73918202161899));
#64279=CARTESIAN_POINT('',(-0.6767,6.12423655037739E-13,-12.278617978381));
#64280=CARTESIAN_POINT('Ctrl Pts',(-0.6767,3.87965912103085E-14,-8.778617978381));
#64281=CARTESIAN_POINT('Ctrl Pts',(-0.676700000000008,-0.141987090474437,
-8.77193911114168));
#64282=CARTESIAN_POINT('Ctrl Pts',(-0.630506051029792,-0.28387092797994,
-8.76524787263758));
#64283=CARTESIAN_POINT('Ctrl Pts',(-0.546771726394805,-0.398702356671295,
-8.75856281976587));
#64284=CARTESIAN_POINT('Ctrl Pts',(-0.431391972538878,-0.556931637615385,
-8.74935130754296));
#64285=CARTESIAN_POINT('Ctrl Pts',(-0.244385431591964,-0.660717521921091,
-8.74013979532005));
#64286=CARTESIAN_POINT('Ctrl Pts',(-0.0490720208180517,-0.674918385268051,
-8.73092828309715));
#64287=CARTESIAN_POINT('Ctrl Pts',(0.14624138995586,-0.68911924861501,-8.72171677087424));
#64288=CARTESIAN_POINT('Ctrl Pts',(0.346293901759852,-0.613475685379523,
-8.71250525865133));
#64289=CARTESIAN_POINT('Ctrl Pts',(0.483348266304422,-0.473600404835669,
-8.70329374642843));
#64290=CARTESIAN_POINT('Ctrl Pts',(0.620402630848992,-0.333725124291814,
-8.69408223420552));
#64291=CARTESIAN_POINT('Ctrl Pts',(0.69195529098788,-0.132173212951097,
-8.68487072198261));
#64292=CARTESIAN_POINT('Ctrl Pts',(0.67377870635233,0.0628103882027554,
-8.6756592097597));
#64293=CARTESIAN_POINT('Ctrl Pts',(0.65560212171678,0.257793989356608,-8.6664476975368));
#64294=CARTESIAN_POINT('Ctrl Pts',(0.548028321998149,0.442647536123078,
-8.65723618531389));
#64295=CARTESIAN_POINT('Ctrl Pts',(0.387481509598483,0.554780109339981,
-8.64802467309099));
#64296=CARTESIAN_POINT('Ctrl Pts',(0.226934697198816,0.666912682556885,
-8.63881316086808));
#64297=CARTESIAN_POINT('Ctrl Pts',(0.0163475632500464,0.704275968725133,
-8.62960164864517));
#64298=CARTESIAN_POINT('Ctrl Pts',(-0.17297564892576,0.654218858547132,
-8.62039013642226));
#64299=CARTESIAN_POINT('Ctrl Pts',(-0.362298861101567,0.604161748369132,
-8.61117862419936));
#64300=CARTESIAN_POINT('Ctrl Pts',(-0.526899805012704,0.467598629623219,
-8.60196711197645));
#64301=CARTESIAN_POINT('Ctrl Pts',(-0.611045038945032,0.290769411012686,
-8.59275559975354));
#64302=CARTESIAN_POINT('Ctrl Pts',(-0.654093108536358,0.200304911090468,
-8.58804305929603));
#64303=CARTESIAN_POINT('Ctrl Pts',(-0.676699999999998,0.100155113678007,
-8.58332912997485));
#64304=CARTESIAN_POINT('Ctrl Pts',(-0.6767,1.49211214436621E-14,-8.578617978381));
#64305=CARTESIAN_POINT('Ctrl Pts',(-0.67719182899154,-0.000898131385784005,
-8.73918202161899));
#64306=CARTESIAN_POINT('Ctrl Pts',(-0.677515066866202,-0.0369757515937125,
-8.73748227372565));
#64307=CARTESIAN_POINT('Ctrl Pts',(-0.6585483635347,-0.297371631309851,
-8.72519146016938));
#64308=CARTESIAN_POINT('Ctrl Pts',(-0.398906696132759,-0.630200070519562,
-8.70760511378165));
#64309=CARTESIAN_POINT('Ctrl Pts',(0.061401085864204,-0.701754831174225,
-8.68642298245581));
#64310=CARTESIAN_POINT('Ctrl Pts',(0.390405367007379,-0.588167853373958,
-8.67053638396139));
#64311=CARTESIAN_POINT('Ctrl Pts',(0.622501320628285,-0.329730194842773,
-8.65464978546701));
#64312=CARTESIAN_POINT('Ctrl Pts',(0.735980420215885,0.123376641684858,
-8.63346765414115));
#64313=CARTESIAN_POINT('Ctrl Pts',(0.487626042973425,0.565143596640834,
-8.61228552281528));
#64314=CARTESIAN_POINT('Ctrl Pts',(0.0420197908343311,0.702471625708329,
-8.59110339148945));
#64315=CARTESIAN_POINT('Ctrl Pts',(-0.414593702842348,0.619976678949471,
-8.56992126016356));
#64316=CARTESIAN_POINT('Ctrl Pts',(-0.662321132177836,0.285300701931316,
-8.55261413687343));
#64317=CARTESIAN_POINT('Ctrl Pts',(-0.677767610364351,0.0308946281568698,
-8.54060254641475));
#64318=CARTESIAN_POINT('Ctrl Pts',(-0.677509650187365,0.000766222167987083,
-8.539182021619));
#64319=CARTESIAN_POINT('Origin',(0.,0.,-12.278617978381));
#64320=CARTESIAN_POINT('',(-0.6767,3.38226048196233E-14,-8.978617978381));
#64321=CARTESIAN_POINT('',(-0.675362603300994,0.000190139876870055,-8.93918202161899));
#64322=CARTESIAN_POINT('',(-0.6767,6.12423655037739E-13,-12.278617978381));
#64323=CARTESIAN_POINT('Ctrl Pts',(-0.6767,2.42061194338461E-14,-8.978617978381));
#64324=CARTESIAN_POINT('Ctrl Pts',(-0.676700000000007,-0.188486775366012,
-8.96975183326294));
#64325=CARTESIAN_POINT('Ctrl Pts',(-0.593581982928983,-0.375700115386127,
-8.96087571042494));
#64326=CARTESIAN_POINT('Ctrl Pts',(-0.453641556933961,-0.502127700712211,
-8.95200457644691));
#64327=CARTESIAN_POINT('Ctrl Pts',(-0.308331729833587,-0.633406210362486,
-8.942793064224));
#64328=CARTESIAN_POINT('Ctrl Pts',(-0.104047973338697,-0.696739479426886,
-8.9335815520011));
#64329=CARTESIAN_POINT('Ctrl Pts',(0.0900397760654122,-0.670683031488117,
-8.92437003977819));
#64330=CARTESIAN_POINT('Ctrl Pts',(0.284127525469521,-0.644626583549348,
-8.91515852755528));
#64331=CARTESIAN_POINT('Ctrl Pts',(0.464473888008647,-0.529656388903286,
-8.90594701533237));
#64332=CARTESIAN_POINT('Ctrl Pts',(0.570014065109352,-0.364701049597491,
-8.89673550310947));
#64333=CARTESIAN_POINT('Ctrl Pts',(0.675554242210057,-0.199745710291696,
-8.88752399088656));
#64334=CARTESIAN_POINT('Ctrl Pts',(0.704360342954921,0.012181552461174,
-8.87831247866365));
#64335=CARTESIAN_POINT('Ctrl Pts',(0.646678698265703,0.199322731291181,
-8.86910096644075));
#64336=CARTESIAN_POINT('Ctrl Pts',(0.588997053576484,0.386463910121188,
-8.85988945421784));
#64337=CARTESIAN_POINT('Ctrl Pts',(0.445881327772811,0.54540051750204,-8.85067794199493));
#64338=CARTESIAN_POINT('Ctrl Pts',(0.26579012487558,0.622317040999701,-8.84146642977203));
#64339=CARTESIAN_POINT('Ctrl Pts',(0.0856989219783484,0.699233564497362,
-8.83225491754912));
#64340=CARTESIAN_POINT('Ctrl Pts',(-0.128078051628479,0.692724978356484,
-8.82304340532621));
#64341=CARTESIAN_POINT('Ctrl Pts',(-0.30315648140067,0.604995072529327,
-8.81383189310331));
#64342=CARTESIAN_POINT('Ctrl Pts',(-0.478234911172861,0.51726516670217,
-8.8046203808804));
#64343=CARTESIAN_POINT('Ctrl Pts',(-0.611416658507033,0.349916493821073,
-8.79540886865749));
#64344=CARTESIAN_POINT('Ctrl Pts',(-0.657606738064317,0.159612869319515,
-8.78619735643459));
#64345=CARTESIAN_POINT('Ctrl Pts',(-0.670275380911006,0.107417924553277,
-8.78367089708339));
#64346=CARTESIAN_POINT('Ctrl Pts',(-0.676699999999997,0.0536606993785083,
-8.78114210001714));
#64347=CARTESIAN_POINT('Ctrl Pts',(-0.6767,3.87965912103085E-14,-8.778617978381));
#64348=CARTESIAN_POINT('Ctrl Pts',(-0.675362603300994,0.000190139876870103,
-8.93918202161899));
#64349=CARTESIAN_POINT('Ctrl Pts',(-0.675434194437074,-0.102521459598344,
-8.93436200103656));
#64350=CARTESIAN_POINT('Ctrl Pts',(-0.62903813993231,-0.318143050274465,
-8.92424644762267));
#64351=CARTESIAN_POINT('Ctrl Pts',(-0.407483346505639,-0.574619229353,-8.90883536137732));
#64352=CARTESIAN_POINT('Ctrl Pts',(-0.0831884995869038,-0.701025996570153,
-8.89294876288291));
#64353=CARTESIAN_POINT('Ctrl Pts',(0.261013149201355,-0.654295064568733,
-8.87706216438852));
#64354=CARTESIAN_POINT('Ctrl Pts',(0.640825685227696,-0.382402165013538,
-8.85588003306267));
#64355=CARTESIAN_POINT('Ctrl Pts',(0.737511168356077,0.11508135887323,-8.8346979017368));
#64356=CARTESIAN_POINT('Ctrl Pts',(0.486773807622215,0.508215808451524,
-8.81351577041096));
#64357=CARTESIAN_POINT('Ctrl Pts',(0.0853438924577135,0.740928769112059,
-8.79233363908507));
#64358=CARTESIAN_POINT('Ctrl Pts',(-0.495149682015662,0.605321926693759,
-8.76755572282111));
#64359=CARTESIAN_POINT('Ctrl Pts',(-0.67550098373734,0.187822552956029,
-8.74807333938859));
#64360=CARTESIAN_POINT('Ctrl Pts',(-0.67719182899154,-0.000898131385784005,
-8.73918202161899));
#64361=CARTESIAN_POINT('Origin',(0.,0.,-12.278617978381));
#64362=CARTESIAN_POINT('',(-0.677457454399445,-0.000117200421055334,-9.17861797838101));
#64363=CARTESIAN_POINT('',(-0.677004582552561,0.000242201296634908,-9.13918202161899));
#64364=CARTESIAN_POINT('',(-0.6767,6.12423655037739E-13,-12.278617978381));
#64365=CARTESIAN_POINT('Ctrl Pts',(-0.677457454399445,-0.000117200421055338,
-9.17861797838101));
#64366=CARTESIAN_POINT('Ctrl Pts',(-0.677485000120747,-0.0157378251760865,
-9.17788033857543));
#64367=CARTESIAN_POINT('Ctrl Pts',(-0.66916109833789,-0.255569895231283,
-9.16655163310692));
#64368=CARTESIAN_POINT('Ctrl Pts',(-0.387077784779294,-0.701144794585703,
-9.14463186197549));
#64369=CARTESIAN_POINT('Ctrl Pts',(0.381518042580854,-0.703508036310348,
-9.11285866498672));
#64370=CARTESIAN_POINT('Ctrl Pts',(0.726298025262084,-0.169616802242028,
-9.08638100082937));
#64371=CARTESIAN_POINT('Ctrl Pts',(0.642587744543107,0.288636323051471,
-9.06519886950353));
#64372=CARTESIAN_POINT('Ctrl Pts',(0.427177008054458,0.562029872978596,
-9.04931227100912));
#64373=CARTESIAN_POINT('Ctrl Pts',(0.106813790756512,0.696290679012175,
-9.03342567251474));
#64374=CARTESIAN_POINT('Ctrl Pts',(-0.358417752115536,0.654542351282965,
-9.01224354118889));
#64375=CARTESIAN_POINT('Ctrl Pts',(-0.647864952636916,0.327011892154612,
-8.99397430981096));
#64376=CARTESIAN_POINT('Ctrl Pts',(-0.67717075072116,0.0512874461424838,
-8.98100061126452));
#64377=CARTESIAN_POINT('Ctrl Pts',(-0.676878116969163,0.000554397463382497,
-8.978617978381));
#64378=CARTESIAN_POINT('Ctrl Pts',(-0.677004582552561,0.000242201296634919,
-9.13918202161899));
#64379=CARTESIAN_POINT('Ctrl Pts',(-0.676751893901764,-0.056062095357369,
-9.13653726117894));
#64380=CARTESIAN_POINT('Ctrl Pts',(-0.654972458078587,-0.225288642313194,
-9.12859696790741));
#64381=CARTESIAN_POINT('Ctrl Pts',(-0.517216387829029,-0.48046329983859,
-9.11536114180443));
#64382=CARTESIAN_POINT('Ctrl Pts',(-0.224617670094119,-0.667665183948138,
-9.09947454331003));
#64383=CARTESIAN_POINT('Ctrl Pts',(0.240882484103758,-0.706303478333916,
-9.07829241198417));
#64384=CARTESIAN_POINT('Ctrl Pts',(0.636622435975274,-0.389715686909015,
-9.05711028065832));
#64385=CARTESIAN_POINT('Ctrl Pts',(0.700009260781494,0.0722432181399054,
-9.03592814933246));
#64386=CARTESIAN_POINT('Ctrl Pts',(0.544690364967499,0.509481527819525,
-9.0147460180066));
#64387=CARTESIAN_POINT('Ctrl Pts',(-0.0219154922400167,0.800595369487078,
-8.98826835384928));
#64388=CARTESIAN_POINT('Ctrl Pts',(-0.58488911759003,0.47170683380819,-8.96131517744292));
#64389=CARTESIAN_POINT('Ctrl Pts',(-0.675276886722274,0.123167471762641,
-8.94495306669949));
#64390=CARTESIAN_POINT('Ctrl Pts',(-0.675362603300994,0.000190139876870103,
-8.93918202161899));
#64391=CARTESIAN_POINT('Origin',(0.,0.,-12.278617978381));
#64392=CARTESIAN_POINT('',(-0.675869510275858,-0.000515265065460229,-9.378617978381));
#64393=CARTESIAN_POINT('',(-0.676863776772284,-0.000147692535406863,-9.33918202161899));
#64394=CARTESIAN_POINT('',(-0.6767,6.12423655037739E-13,-12.278617978381));
#64395=CARTESIAN_POINT('Ctrl Pts',(-0.675869510275858,-0.000515265065460194,
-9.378617978381));
#64396=CARTESIAN_POINT('Ctrl Pts',(-0.676533915652542,-0.0826540124146915,
-9.37476006588634));
#64397=CARTESIAN_POINT('Ctrl Pts',(-0.62509694516892,-0.389649898441223,
-9.36031108772875));
#64398=CARTESIAN_POINT('Ctrl Pts',(-0.164628083532023,-0.783183993759156,
-9.33527104390821));
#64399=CARTESIAN_POINT('Ctrl Pts',(0.443775836884319,-0.599451155391359,
-9.30879337975089));
#64400=CARTESIAN_POINT('Ctrl Pts',(0.676623900661522,-0.195984778682572,
-9.28761124842504));
#64401=CARTESIAN_POINT('Ctrl Pts',(0.689421792526712,0.151839936511941,
-9.27172464993064));
#64402=CARTESIAN_POINT('Ctrl Pts',(0.532157948497518,0.461560194802287,
-9.25583805143624));
#64403=CARTESIAN_POINT('Ctrl Pts',(0.150536857936622,0.730908769311981,
-9.2346559201104));
#64404=CARTESIAN_POINT('Ctrl Pts',(-0.351086430223958,0.658714476175113,
-9.21347378878452));
#64405=CARTESIAN_POINT('Ctrl Pts',(-0.629910032807131,0.305441235120693,
-9.19302929726426));
#64406=CARTESIAN_POINT('Ctrl Pts',(-0.677287248765119,0.0964029928941302,
-9.1831758714069));
#64407=CARTESIAN_POINT('Ctrl Pts',(-0.677457454399445,-0.000117200421055338,
-9.17861797838101));
#64408=CARTESIAN_POINT('Ctrl Pts',(-0.676863776772284,-0.000147692535406885,
-9.33918202161899));
#64409=CARTESIAN_POINT('Ctrl Pts',(-0.67688013367565,-0.0100987013725557,
-9.33871252132131));
#64410=CARTESIAN_POINT('Ctrl Pts',(-0.67431259378526,-0.132268211572331,
-9.33294748819216));
#64411=CARTESIAN_POINT('Ctrl Pts',(-0.603416199871352,-0.363481478631069,
-9.32188692223156));
#64412=CARTESIAN_POINT('Ctrl Pts',(-0.273628850822219,-0.694273884466568,
-9.30070479090568));
#64413=CARTESIAN_POINT('Ctrl Pts',(0.23294438000554,-0.709156793970058,
-9.27952265957983));
#64414=CARTESIAN_POINT('Ctrl Pts',(0.580307452228801,-0.398089573632346,
-9.25834052825398));
#64415=CARTESIAN_POINT('Ctrl Pts',(0.744972095404132,0.0357155140929017,
-9.2371583969281));
#64416=CARTESIAN_POINT('Ctrl Pts',(0.501563565304761,0.624393485234313,
-9.2106807327708));
#64417=CARTESIAN_POINT('Ctrl Pts',(-0.255245053230173,0.758504803392499,
-9.17890753578199));
#64418=CARTESIAN_POINT('Ctrl Pts',(-0.643387444434367,0.338269595953793,
-9.15507463206474));
#64419=CARTESIAN_POINT('Ctrl Pts',(-0.677257845603916,0.0566744863639501,
-9.1418327940104));
#64420=CARTESIAN_POINT('Ctrl Pts',(-0.677004582552561,0.000242201296634919,
-9.13918202161899));
#64421=CARTESIAN_POINT('Origin',(0.,0.,-12.278617978381));
#64422=CARTESIAN_POINT('',(-0.676043544325099,0.00066804154600488,-9.57861797838101));
#64423=CARTESIAN_POINT('',(-0.6767,6.90086009169644E-14,-9.53918202161899));
#64424=CARTESIAN_POINT('',(-0.6767,6.12423655037739E-13,-12.278617978381));
#64425=CARTESIAN_POINT('Ctrl Pts',(-0.676043544325099,0.000668041546004881,
-9.57861797838101));
#64426=CARTESIAN_POINT('Ctrl Pts',(-0.674905073035165,-0.148231709807252,
-9.57163979319725));
#64427=CARTESIAN_POINT('Ctrl Pts',(-0.552970071990971,-0.524995973750943,
-9.55407054235057));
#64428=CARTESIAN_POINT('Ctrl Pts',(-0.0498142904822183,-0.744175528733757,
-9.5312057586724));
#64429=CARTESIAN_POINT('Ctrl Pts',(0.388845301867087,-0.587391919962783,
-9.51002362734656));
#64430=CARTESIAN_POINT('Ctrl Pts',(0.623764909652236,-0.33056786265037,
-9.49413702885215));
#64431=CARTESIAN_POINT('Ctrl Pts',(0.704398011625223,0.00730320432709524,
-9.47825043035776));
#64432=CARTESIAN_POINT('Ctrl Pts',(0.587893373397589,0.459641551831196,
-9.45706829903191));
#64433=CARTESIAN_POINT('Ctrl Pts',(0.158825559311775,0.729342775599619,
-9.43588616770604));
#64434=CARTESIAN_POINT('Ctrl Pts',(-0.298302397103462,0.637375656602442,
-9.4147040363802));
#64435=CARTESIAN_POINT('Ctrl Pts',(-0.594288149775049,0.399868325412857,
-9.39737981754899));
#64436=CARTESIAN_POINT('Ctrl Pts',(-0.674709934164887,0.14284018110295,
-9.38535113154927));
#64437=CARTESIAN_POINT('Ctrl Pts',(-0.675869510275858,-0.000515265065460194,
-9.378617978381));
#64438=CARTESIAN_POINT('Ctrl Pts',(-0.676700480522553,-0.000119391525579517,
-9.53918202161899));
#64439=CARTESIAN_POINT('Ctrl Pts',(-0.676985427297024,-0.0767212178377484,
-9.53559224863222));
#64440=CARTESIAN_POINT('Ctrl Pts',(-0.627680731706276,-0.37935610130508,
-9.5214114099825));
#64441=CARTESIAN_POINT('Ctrl Pts',(-0.281526301655526,-0.691309904519107,
-9.50193503850135));
#64442=CARTESIAN_POINT('Ctrl Pts',(0.184600760711549,-0.679083652352037,
-9.48075290717548));
#64443=CARTESIAN_POINT('Ctrl Pts',(0.590931414136129,-0.455037454134073,
-9.45957077584963));
#64444=CARTESIAN_POINT('Ctrl Pts',(0.786489778819108,0.151218590977907,
-9.43309311169231));
#64445=CARTESIAN_POINT('Ctrl Pts',(0.296474486791864,0.743358898950881,
-9.40131991470351));
#64446=CARTESIAN_POINT('Ctrl Pts',(-0.334422425230761,0.666663575280057,
-9.3748422505462));
#64447=CARTESIAN_POINT('Ctrl Pts',(-0.626382474312723,0.317021538909944,
-9.35412961951802));
#64448=CARTESIAN_POINT('Ctrl Pts',(-0.676695642804777,0.102139553349016,
-9.34400805415277));
#64449=CARTESIAN_POINT('Ctrl Pts',(-0.676863776772284,-0.000147692535406885,
-9.33918202161899));
#64450=CARTESIAN_POINT('Origin',(0.,0.,-12.278617978381));
#64451=CARTESIAN_POINT('',(-0.677843803276718,-0.000108888079095037,-9.778617978381));
#64452=CARTESIAN_POINT('',(-0.6767,6.40345347733506E-14,-9.73918202161899));
#64453=CARTESIAN_POINT('',(-0.6767,6.12423655037739E-13,-12.278617978381));
#64454=CARTESIAN_POINT('Ctrl Pts',(-0.677843803276718,-0.000108888079095024,
-9.778617978381));
#64455=CARTESIAN_POINT('Ctrl Pts',(-0.67702325059819,-0.213595101097744,
-9.76851952050815));
#64456=CARTESIAN_POINT('Ctrl Pts',(-0.509576090600237,-0.538781197494748,
-9.75312552980383));
#64457=CARTESIAN_POINT('Ctrl Pts',(-0.0838752645359608,-0.69942467530156,
-9.73243600626807));
#64458=CARTESIAN_POINT('Ctrl Pts',(0.261433978866206,-0.655751514695071,
-9.71654940777366));
#64459=CARTESIAN_POINT('Ctrl Pts',(0.541613442530161,-0.450427324266235,
-9.70066280927928));
#64460=CARTESIAN_POINT('Ctrl Pts',(0.745637002453177,-0.0302396300775194,
-9.6794806779534));
#64461=CARTESIAN_POINT('Ctrl Pts',(0.593197195641168,0.453082254887026,
-9.65829854662756));
#64462=CARTESIAN_POINT('Ctrl Pts',(0.185243328053068,0.678908651556959,
-9.6371164153017));
#64463=CARTESIAN_POINT('Ctrl Pts',(-0.278581983793115,0.691846152828526,
-9.61593428397583));
#64464=CARTESIAN_POINT('Ctrl Pts',(-0.629111894284224,0.380057342876616,
-9.59643480500227));
#64465=CARTESIAN_POINT('Ctrl Pts',(-0.676632975615784,0.0777592896071504,
-9.58223085886018));
#64466=CARTESIAN_POINT('Ctrl Pts',(-0.676043544325099,0.000668041546004881,
-9.57861797838101));
#64467=CARTESIAN_POINT('Ctrl Pts',(-0.6767,8.3267505544905E-14,-9.73918202161899));
#64468=CARTESIAN_POINT('Ctrl Pts',(-0.676700000000012,-0.0950032677258063,
-9.73471320540252));
#64469=CARTESIAN_POINT('Ctrl Pts',(-0.656390733383678,-0.190013320510327,
-9.73024174265372));
#64470=CARTESIAN_POINT('Ctrl Pts',(-0.617527853484026,-0.276734963767522,
-9.72577160317108));
#64471=CARTESIAN_POINT('Ctrl Pts',(-0.537444022855581,-0.455440232351895,
-9.71656009094818));
#64472=CARTESIAN_POINT('Ctrl Pts',(-0.376005648018375,-0.595727820070727,
-9.70734857872527));
#64473=CARTESIAN_POINT('Ctrl Pts',(-0.187875333211616,-0.650096722934845,
-9.69813706650236));
#64474=CARTESIAN_POINT('Ctrl Pts',(0.000254981595142312,-0.704465625798963,
-9.68892555427946));
#64475=CARTESIAN_POINT('Ctrl Pts',(0.211640680406031,-0.671922692982764,
-9.67971404205655));
#64476=CARTESIAN_POINT('Ctrl Pts',(0.374707127961123,-0.563486874962609,
-9.67050252983364));
#64477=CARTESIAN_POINT('Ctrl Pts',(0.537773575516215,-0.455051056942453,
-9.66129101761074));
#64478=CARTESIAN_POINT('Ctrl Pts',(0.649542054782686,-0.272703138992979,
-9.65207950538783));
#64479=CARTESIAN_POINT('Ctrl Pts',(0.672168056022858,-0.0781856410247563,
-9.64286799316492));
#64480=CARTESIAN_POINT('Ctrl Pts',(0.69479405726303,0.116331856943467,-9.63365648094202));
#64481=CARTESIAN_POINT('Ctrl Pts',(0.627864273777154,0.319465704986035,
-9.62444496871911));
#64482=CARTESIAN_POINT('Ctrl Pts',(0.494040952197692,0.462435322560461,
-9.6152334564962));
#64483=CARTESIAN_POINT('Ctrl Pts',(0.360217630618229,0.605404940134888,
-9.6060219442733));
#64484=CARTESIAN_POINT('Ctrl Pts',(0.161945306981591,0.68559871681223,-9.59681043205039));
#64485=CARTESIAN_POINT('Ctrl Pts',(-0.0336415374002855,0.675863253152104,
-9.58759891982748));
#64486=CARTESIAN_POINT('Ctrl Pts',(-0.229228381782162,0.666127789491978,
-9.57838740760458));
#64487=CARTESIAN_POINT('Ctrl Pts',(-0.418556983330429,0.56664092214847,
-9.56917589538167));
#64488=CARTESIAN_POINT('Ctrl Pts',(-0.537521181238947,0.411088639735383,
-9.55996438315876));
#64489=CARTESIAN_POINT('Ctrl Pts',(-0.626987380758105,0.294106625157086,
-9.55303692931217));
#64490=CARTESIAN_POINT('Ctrl Pts',(-0.676699999999985,0.147120594995907,
-9.54610236148133));
#64491=CARTESIAN_POINT('Ctrl Pts',(-0.6767,6.90085211640358E-14,-9.53918202161899));
#64492=CARTESIAN_POINT('Origin',(0.,0.,-12.278617978381));
#64493=CARTESIAN_POINT('',(-0.67610244318158,-0.000267596609132326,-9.978617978381));
#64494=CARTESIAN_POINT('',(-0.677469765816856,0.000446699746677298,-9.93918202161899));
#64495=CARTESIAN_POINT('',(-0.6767,6.12423655037739E-13,-12.278617978381));
#64496=CARTESIAN_POINT('Ctrl Pts',(-0.67610244318158,-0.00026759660913226,
-9.978617978381));
#64497=CARTESIAN_POINT('Ctrl Pts',(-0.676583469304382,-0.0561528993705457,
-9.97599031348199));
#64498=CARTESIAN_POINT('Ctrl Pts',(-0.657565044010056,-0.224499853671964,
-9.96806711575151));
#64499=CARTESIAN_POINT('Ctrl Pts',(-0.516703214563073,-0.478798208519891,
-9.95484838518958));
#64500=CARTESIAN_POINT('Ctrl Pts',(-0.225239754106489,-0.669047701962083,
-9.93896178669518));
#64501=CARTESIAN_POINT('Ctrl Pts',(0.12122757218792,-0.693926344302069,
-9.92307518820078));
#64502=CARTESIAN_POINT('Ctrl Pts',(0.54874197779906,-0.505738288500843,
-9.90189305687493));
#64503=CARTESIAN_POINT('Ctrl Pts',(0.745433350289229,-0.0386725081502612,
-9.88071092554906));
#64504=CARTESIAN_POINT('Ctrl Pts',(0.580683923966688,0.397540222108045,
-9.85952879422322));
#64505=CARTESIAN_POINT('Ctrl Pts',(0.235535653683076,0.707659506204665,
-9.83834666289734));
#64506=CARTESIAN_POINT('Ctrl Pts',(-0.401313885472845,0.693094798545597,
-9.81186899874004));
#64507=CARTESIAN_POINT('Ctrl Pts',(-0.672947296769713,0.244628003099024,
-9.79019425962409));
#64508=CARTESIAN_POINT('Ctrl Pts',(-0.677883830243875,0.0103050754123359,
-9.77911058617108));
#64509=CARTESIAN_POINT('Ctrl Pts',(-0.677843803276718,-0.000108888079095024,
-9.778617978381));
#64510=CARTESIAN_POINT('Ctrl Pts',(-0.677469765816856,0.000446699746677286,
-9.93918202161899));
#64511=CARTESIAN_POINT('Ctrl Pts',(-0.67720463427496,-0.0957460685350012,
-9.9346472360855));
#64512=CARTESIAN_POINT('Ctrl Pts',(-0.629944124500754,-0.305187579010285,
-9.92481691772054));
#64513=CARTESIAN_POINT('Ctrl Pts',(-0.353382605913268,-0.65679506295015,
-9.90439553369265));
#64514=CARTESIAN_POINT('Ctrl Pts',(0.276533191529025,-0.751639959307012,
-9.87791786953533));
#64515=CARTESIAN_POINT('Ctrl Pts',(0.781545819003339,-0.172237355896938,
-9.84614467254655));
#64516=CARTESIAN_POINT('Ctrl Pts',(0.603738860340227,0.437924730538819,
-9.8196670083892));
#64517=CARTESIAN_POINT('Ctrl Pts',(0.202556190221955,0.674685798149359,
-9.79848487706338));
#64518=CARTESIAN_POINT('Ctrl Pts',(-0.145127604936405,0.690865944026855,
-9.78259827856895));
#64519=CARTESIAN_POINT('Ctrl Pts',(-0.456362724825398,0.536621802543421,
-9.76671168007457));
#64520=CARTESIAN_POINT('Ctrl Pts',(-0.642914547871936,0.277692214258572,
-9.75223959442458));
#64521=CARTESIAN_POINT('Ctrl Pts',(-0.676032577839247,0.0826491836746199,
-9.74306304160606));
#64522=CARTESIAN_POINT('Ctrl Pts',(-0.675534132712119,0.000105302539254004,
-9.73918202161899));
#64523=CARTESIAN_POINT('Origin',(0.,0.,-12.278617978381));
#64524=CARTESIAN_POINT('',(-0.6767,8.09105386856412E-14,-10.178617978381));
#64525=CARTESIAN_POINT('',(-0.676977044559859,-0.000480244224215359,-10.139182021619));
#64526=CARTESIAN_POINT('',(-0.6767,6.12423655037739E-13,-12.278617978381));
#64527=CARTESIAN_POINT('Ctrl Pts',(-0.676487528708653,-6.3808423934459E-5,
-10.178617978381));
#64528=CARTESIAN_POINT('Ctrl Pts',(-0.67646538092208,-0.00970439412085054,
-10.1781655736244));
#64529=CARTESIAN_POINT('Ctrl Pts',(-0.67359920801602,-0.13217276423391,
-10.1724176360363));
#64530=CARTESIAN_POINT('Ctrl Pts',(-0.604785322978651,-0.364132513572057,
-10.1613741656167));
#64531=CARTESIAN_POINT('Ctrl Pts',(-0.356816358110809,-0.607381249430332,
-10.1454875671223));
#64532=CARTESIAN_POINT('Ctrl Pts',(0.0908551895918876,-0.740698527863264,
-10.1243054357964));
#64533=CARTESIAN_POINT('Ctrl Pts',(0.543127711937286,-0.512033916001494,
-10.1031233044706));
#64534=CARTESIAN_POINT('Ctrl Pts',(0.69994058004243,-0.0729056387183608,
-10.0819411731447));
#64535=CARTESIAN_POINT('Ctrl Pts',(0.637628208112178,0.386897000631171,
-10.0607590418189));
#64536=CARTESIAN_POINT('Ctrl Pts',(0.142798839180318,0.788062006426542,
-10.0342813776615));
#64537=CARTESIAN_POINT('Ctrl Pts',(-0.525979911312534,0.564879541526795,
-10.0051358455718));
#64538=CARTESIAN_POINT('Ctrl Pts',(-0.67464464550151,0.169098391751588,
-9.98658137914492));
#64539=CARTESIAN_POINT('Ctrl Pts',(-0.67610244318158,-0.00026759660913226,
-9.978617978381));
#64540=CARTESIAN_POINT('Ctrl Pts',(-0.676977044559859,-0.000480244224215366,
-10.139182021619));
#64541=CARTESIAN_POINT('Ctrl Pts',(-0.677246035158063,-0.0505808665251606,
-10.1368224962279));
#64542=CARTESIAN_POINT('Ctrl Pts',(-0.648092810473929,-0.325072929503903,
-10.1238719051738));
#64543=CARTESIAN_POINT('Ctrl Pts',(-0.275804889831566,-0.751907505740747,
-10.1003302484568));
#64544=CARTESIAN_POINT('Ctrl Pts',(0.484188776139409,-0.637213310460941,
-10.0685570514681));
#64545=CARTESIAN_POINT('Ctrl Pts',(0.743655850199394,-0.0570496061916968,
-10.0420793873107));
#64546=CARTESIAN_POINT('Ctrl Pts',(0.591145954131398,0.383114078749073,
-10.0208972559849));
#64547=CARTESIAN_POINT('Ctrl Pts',(0.336618815106218,0.62052038455411,-10.0050106574905));
#64548=CARTESIAN_POINT('Ctrl Pts',(-0.000452053710239919,0.704435725401867,
-9.98912405899608));
#64549=CARTESIAN_POINT('Ctrl Pts',(-0.453902103296527,0.592335931104618,
-9.96794192767022));
#64550=CARTESIAN_POINT('Ctrl Pts',(-0.669133831075285,0.257202722580053,
-9.95129458187786));
#64551=CARTESIAN_POINT('Ctrl Pts',(-0.677514243797703,0.0165838220017427,
-9.93994276891696));
#64552=CARTESIAN_POINT('Ctrl Pts',(-0.677469765816856,0.000446699746677286,
-9.93918202161899));
#64553=CARTESIAN_POINT('Origin',(0.,0.,-12.278617978381));
#64554=CARTESIAN_POINT('',(-0.6767,6.63200977852672E-14,-10.378617978381));
#64555=CARTESIAN_POINT('',(-0.675326265922369,-7.01824404411022E-5,-10.339182021619));
#64556=CARTESIAN_POINT('',(-0.6767,6.12423655037739E-13,-12.278617978381));
#64557=CARTESIAN_POINT('Ctrl Pts',(-0.6767,6.63200977852672E-14,-10.378617978381));
#64558=CARTESIAN_POINT('Ctrl Pts',(-0.676700000000012,-0.122190759824434,
-10.3728703018844));
#64559=CARTESIAN_POINT('Ctrl Pts',(-0.642782324826098,-0.244335729754349,
-10.3671166238281));
#64560=CARTESIAN_POINT('Ctrl Pts',(-0.579718464473323,-0.349069322554551,
-10.3613659465517));
#64561=CARTESIAN_POINT('Ctrl Pts',(-0.478701924588147,-0.516833000439738,
-10.3521544343287));
#64562=CARTESIAN_POINT('Ctrl Pts',(-0.301547908367897,-0.636663758908016,
-10.3429429221058));
#64563=CARTESIAN_POINT('Ctrl Pts',(-0.108240294415161,-0.667987221932365,
-10.3337314098829));
#64564=CARTESIAN_POINT('Ctrl Pts',(0.0850673195375753,-0.699310684956715,
-10.32451989766));
#64565=CARTESIAN_POINT('Ctrl Pts',(0.290997402097898,-0.641554670250488,
-10.3153083854371));
#64566=CARTESIAN_POINT('Ctrl Pts',(0.439822575154538,-0.514275210742682,
-10.3060968732142));
#64567=CARTESIAN_POINT('Ctrl Pts',(0.588647748211179,-0.386995751234877,
-10.2968853609913));
#64568=CARTESIAN_POINT('Ctrl Pts',(0.677649438541112,-0.192517846946338,
-10.2876738487684));
#64569=CARTESIAN_POINT('Ctrl Pts',(0.676691910573216,0.00330880110782365,
-10.2784623365455));
#64570=CARTESIAN_POINT('Ctrl Pts',(0.675734382605319,0.199135449161986,
-10.2692508243226));
#64571=CARTESIAN_POINT('Ctrl Pts',(0.584835127398669,0.392733696935367,
-10.2600393120997));
#64572=CARTESIAN_POINT('Ctrl Pts',(0.434772390943479,0.518551692768706,
-10.2508277998768));
#64573=CARTESIAN_POINT('Ctrl Pts',(0.28470965448829,0.644369688602045,-10.2416162876539));
#64574=CARTESIAN_POINT('Ctrl Pts',(0.0782246164433667,0.700109128872225,
-10.232404775431));
#64575=CARTESIAN_POINT('Ctrl Pts',(-0.114767438629307,0.666896787389524,
-10.2231932632081));
#64576=CARTESIAN_POINT('Ctrl Pts',(-0.307759493701982,0.633684445906823,
-10.2139817509851));
#64577=CARTESIAN_POINT('Ctrl Pts',(-0.483733200957191,0.51212700889491,
-10.2047702387622));
#64578=CARTESIAN_POINT('Ctrl Pts',(-0.583104331267889,0.343383501142131,
-10.1955587265393));
#64579=CARTESIAN_POINT('Ctrl Pts',(-0.644021628814161,0.239938985228529,
-10.1899118104866));
#64580=CARTESIAN_POINT('Ctrl Pts',(-0.676699999999986,0.119990517192851,
-10.1842621586486));
#64581=CARTESIAN_POINT('Ctrl Pts',(-0.6767,8.09105695617297E-14,-10.178617978381));
#64582=CARTESIAN_POINT('Ctrl Pts',(-0.675326265922369,-7.01824404411369E-5,
-10.339182021619));
#64583=CARTESIAN_POINT('Ctrl Pts',(-0.675452075247173,-0.116937975956912,
-10.3337022235388));
#64584=CARTESIAN_POINT('Ctrl Pts',(-0.591837088309436,-0.459635281089491,
-10.3176313597956));
#64585=CARTESIAN_POINT('Ctrl Pts',(-0.0434573418998398,-0.79911891067786,
-10.2909694303896));
#64586=CARTESIAN_POINT('Ctrl Pts',(0.529876458749172,-0.524890102369867,
-10.2644917662322));
#64587=CARTESIAN_POINT('Ctrl Pts',(0.698575844497316,-0.0906737332777898,
-10.2433096349064));
#64588=CARTESIAN_POINT('Ctrl Pts',(0.658263143903542,0.255043932899648,
-10.227423036412));
#64589=CARTESIAN_POINT('Ctrl Pts',(0.455673622452517,0.537207078672659,
-10.2115364379176));
#64590=CARTESIAN_POINT('Ctrl Pts',(0.0374900855372222,0.745307633223355,
-10.1903543065917));
#64591=CARTESIAN_POINT('Ctrl Pts',(-0.447291532886714,0.597575708356613,
-10.1691721752659));
#64592=CARTESIAN_POINT('Ctrl Pts',(-0.651478821048851,0.237033566356607,
-10.1503495693311));
#64593=CARTESIAN_POINT('Ctrl Pts',(-0.676642333858851,0.061861021690888,
-10.1421180290593));
#64594=CARTESIAN_POINT('Ctrl Pts',(-0.676977044559859,-0.000480244224215366,
-10.139182021619));
#64595=CARTESIAN_POINT('Origin',(0.,0.,-12.278617978381));
#64596=CARTESIAN_POINT('',(-0.6767,7.09625967803593E-14,-10.578617978381));
#64597=CARTESIAN_POINT('',(-0.677129451882474,0.000855468478137583,-10.539182021619));
#64598=CARTESIAN_POINT('',(-0.6767,6.12423655037739E-13,-12.278617978381));
#64599=CARTESIAN_POINT('Ctrl Pts',(-0.6767,9.01955675519137E-14,-10.578617978381));
#64600=CARTESIAN_POINT('Ctrl Pts',(-0.676700000000023,-0.16852564549507,
-10.5706907759225));
#64601=CARTESIAN_POINT('Ctrl Pts',(-0.610812984105749,-0.336600349346967,
-10.5627444616155));
#64602=CARTESIAN_POINT('Ctrl Pts',(-0.496045337245928,-0.460284600433876,
-10.5548077032327));
#64603=CARTESIAN_POINT('Ctrl Pts',(-0.362844409252623,-0.603834263372039,
-10.5455961910098));
#64604=CARTESIAN_POINT('Ctrl Pts',(-0.1649223581656,-0.684888676154772,
-10.5363846787869));
#64605=CARTESIAN_POINT('Ctrl Pts',(0.0307049360566569,-0.676003030245987,
-10.527173166564));
#64606=CARTESIAN_POINT('Ctrl Pts',(0.226332230278914,-0.667117384337202,
-10.5179616543411));
#64607=CARTESIAN_POINT('Ctrl Pts',(0.416091265164732,-0.568453992862703,
-10.5087501421182));
#64608=CARTESIAN_POINT('Ctrl Pts',(0.535730136324974,-0.41342001769777,
-10.4995386298953));
#64609=CARTESIAN_POINT('Ctrl Pts',(0.655369007485216,-0.258386042532837,
-10.4903271176724));
#64610=CARTESIAN_POINT('Ctrl Pts',(0.702702284694006,-0.049813472412212,
-10.4811156054494));
#64611=CARTESIAN_POINT('Ctrl Pts',(0.661703046210972,0.141675575294828,
-10.4719040932265));
#64612=CARTESIAN_POINT('Ctrl Pts',(0.620703807727938,0.333164623001869,
-10.4626925810036));
#64613=CARTESIAN_POINT('Ctrl Pts',(0.49212098217594,0.504072238721918,-10.4534810687807));
#64614=CARTESIAN_POINT('Ctrl Pts',(0.319492372213088,0.596529558444218,
-10.4442695565578));
#64615=CARTESIAN_POINT('Ctrl Pts',(0.146863762250237,0.688986878166518,
-10.4350580443349));
#64616=CARTESIAN_POINT('Ctrl Pts',(-0.0666572441116555,0.701304994104118,
-10.425846532112));
#64617=CARTESIAN_POINT('Ctrl Pts',(-0.248773002156532,0.629313024970901,
-10.4166350198891));
#64618=CARTESIAN_POINT('Ctrl Pts',(-0.430888760201408,0.557321055837685,
-10.4074235076662));
#64619=CARTESIAN_POINT('Ctrl Pts',(-0.578272581216982,0.402334071090911,
-10.3982119954433));
#64620=CARTESIAN_POINT('Ctrl Pts',(-0.641020695498184,0.21683025144805,
-10.3890004832204));
#64621=CARTESIAN_POINT('Ctrl Pts',(-0.664595637535239,0.147135060670931,
-10.3855396482739));
#64622=CARTESIAN_POINT('Ctrl Pts',(-0.676699999999993,0.0735360430443412,
-10.3820770074178));
#64623=CARTESIAN_POINT('Ctrl Pts',(-0.6767,6.63200977852672E-14,-10.378617978381));
#64624=CARTESIAN_POINT('Ctrl Pts',(-0.677129451882474,0.000855468478137604,
-10.539182021619));
#64625=CARTESIAN_POINT('Ctrl Pts',(-0.675347882449493,-0.181846972849585,
-10.5305819508497));
#64626=CARTESIAN_POINT('Ctrl Pts',(-0.504225925926224,-0.593140613922127,
-10.5113908144174));
#64627=CARTESIAN_POINT('Ctrl Pts',(0.0640780911147829,-0.743083225043802,
-10.4869041451538));
#64628=CARTESIAN_POINT('Ctrl Pts',(0.473750232264011,-0.521335452325531,
-10.4657220138279));
#64629=CARTESIAN_POINT('Ctrl Pts',(0.666825430939749,-0.231736097711846,
-10.4498354153335));
#64630=CARTESIAN_POINT('Ctrl Pts',(0.695072554279996,0.114472878279935,
-10.4339488168391));
#64631=CARTESIAN_POINT('Ctrl Pts',(0.511051301097596,0.5437973356877,-10.4127666855133));
#64632=CARTESIAN_POINT('Ctrl Pts',(0.0459205840941021,0.745021974552772,
-10.3915845541874));
#64633=CARTESIAN_POINT('Ctrl Pts',(-0.39187382810385,0.584522840096347,
-10.3704024228615));
#64634=CARTESIAN_POINT('Ctrl Pts',(-0.624243083129975,0.33091208544373,
-10.3547000896159));
#64635=CARTESIAN_POINT('Ctrl Pts',(-0.675208917597839,0.108937951749951,
-10.3442932892017));
#64636=CARTESIAN_POINT('Ctrl Pts',(-0.675326265922369,-7.01824404411369E-5,
-10.339182021619));
#64637=CARTESIAN_POINT('Origin',(0.,0.,-12.278617978381));
#64638=CARTESIAN_POINT('',(-0.676458265251918,-5.37981942149026E-5,-10.778617978381));
#64639=CARTESIAN_POINT('',(-0.677536220770138,-0.000773839678422261,-10.739182021619));
#64640=CARTESIAN_POINT('',(-0.6767,6.12423655037739E-13,-12.278617978381));
#64641=CARTESIAN_POINT('Ctrl Pts',(-0.675361946382602,-0.000297784530493374,
-10.778617978381));
#64642=CARTESIAN_POINT('Ctrl Pts',(-0.675700118216433,-0.0963995788455786,
-10.7741002883886));
#64643=CARTESIAN_POINT('Ctrl Pts',(-0.634006218158301,-0.304924171127997,
-10.7642870655646));
#64644=CARTESIAN_POINT('Ctrl Pts',(-0.423251854828125,-0.562218743134393,
-10.7491783099093));
#64645=CARTESIAN_POINT('Ctrl Pts',(0.0028831951113741,-0.745822169195642,
-10.7279961785834));
#64646=CARTESIAN_POINT('Ctrl Pts',(0.601706547663041,-0.528566424343903,
-10.7015185144261));
#64647=CARTESIAN_POINT('Ctrl Pts',(0.769006630385937,0.221604098315976,
-10.6697453174373));
#64648=CARTESIAN_POINT('Ctrl Pts',(0.321574591885842,0.672955022981378,
-10.64326765328));
#64649=CARTESIAN_POINT('Ctrl Pts',(-0.143965254934612,0.689567938489952,
-10.6220855219541));
#64650=CARTESIAN_POINT('Ctrl Pts',(-0.457226793531636,0.537867487033261,
-10.6061989234597));
#64651=CARTESIAN_POINT('Ctrl Pts',(-0.639545145736122,0.278781774607292,
-10.5917097422687));
#64652=CARTESIAN_POINT('Ctrl Pts',(-0.677073472553969,0.0825194861469949,
-10.5825160939091));
#64653=CARTESIAN_POINT('Ctrl Pts',(-0.677379594393192,-0.000411018920503776,
-10.578617978381));
#64654=CARTESIAN_POINT('Ctrl Pts',(-0.677536220770138,-0.000773839678422372,
-10.739182021619));
#64655=CARTESIAN_POINT('Ctrl Pts',(-0.677711236608313,-0.0247038387901337,
-10.7380527438235));
#64656=CARTESIAN_POINT('Ctrl Pts',(-0.665747438455249,-0.272785151399114,
-10.7263324003651));
#64657=CARTESIAN_POINT('Ctrl Pts',(-0.432196993595701,-0.60785231744993,
-10.7093165240753));
#64658=CARTESIAN_POINT('Ctrl Pts',(0.0236003080504614,-0.704040454719466,
-10.6881343927494));
#64659=CARTESIAN_POINT('Ctrl Pts',(0.358233295234271,-0.608298183883769,
-10.672247794255));
#64660=CARTESIAN_POINT('Ctrl Pts',(0.603882212681613,-0.36270672558111,
-10.6563611957606));
#64661=CARTESIAN_POINT('Ctrl Pts',(0.741547131220323,0.0836470372069074,
-10.6351790644348));
#64662=CARTESIAN_POINT('Ctrl Pts',(0.517292027842344,0.53812210560505,-10.6139969331089));
#64663=CARTESIAN_POINT('Ctrl Pts',(0.0797096438481298,0.699198412773276,
-10.5928148017831));
#64664=CARTESIAN_POINT('Ctrl Pts',(-0.380677283636059,0.641360917581681,
-10.5716326704572));
#64665=CARTESIAN_POINT('Ctrl Pts',(-0.654778622651578,0.30990463904442,
-10.5537550770692));
#64666=CARTESIAN_POINT('Ctrl Pts',(-0.677541901470257,0.0431527515463504,
-10.5411730165126));
#64667=CARTESIAN_POINT('Ctrl Pts',(-0.677129451882474,0.000855468478137604,
-10.539182021619));
#64668=CARTESIAN_POINT('Origin',(0.,0.,-12.278617978381));
#64669=CARTESIAN_POINT('',(-0.6767,8.02475947705433E-14,-10.978617978381));
#64670=CARTESIAN_POINT('',(-0.67542960639225,3.49951570662865E-5,-10.939182021619));
#64671=CARTESIAN_POINT('',(-0.6767,6.12423655037739E-13,-12.278617978381));
#64672=CARTESIAN_POINT('Ctrl Pts',(-0.6767,9.46723228492091E-14,-10.978617978381));
#64673=CARTESIAN_POINT('Ctrl Pts',(-0.676700000000009,-0.0658041958681062,
-10.9755226442452));
#64674=CARTESIAN_POINT('Ctrl Pts',(-0.667020980110906,-0.131688646825892,
-10.972423161636));
#64675=CARTESIAN_POINT('Ctrl Pts',(-0.64807015609023,-0.194751027687109,
-10.9693257532635));
#64676=CARTESIAN_POINT('Ctrl Pts',(-0.591711508438059,-0.382294877980198,
-10.9601142410406));
#64677=CARTESIAN_POINT('Ctrl Pts',(-0.449721734150075,-0.542238180858732,
-10.9509027288177));
#64678=CARTESIAN_POINT('Ctrl Pts',(-0.270178193059374,-0.620424559471312,
-10.9416912165948));
#64679=CARTESIAN_POINT('Ctrl Pts',(-0.0906346519686727,-0.698610938083892,
-10.9324797043719));
#64680=CARTESIAN_POINT('Ctrl Pts',(0.123182953619341,-0.693612170370124,
-10.923268192149));
#64681=CARTESIAN_POINT('Ctrl Pts',(0.298876551279699,-0.607120825779477,
-10.9140566799261));
#64682=CARTESIAN_POINT('Ctrl Pts',(0.474570148940057,-0.52062948118883,
-10.9048451677032));
#64683=CARTESIAN_POINT('Ctrl Pts',(0.608930362864581,-0.354225487690465,
-10.8956336554803));
#64684=CARTESIAN_POINT('Ctrl Pts',(0.656463182062029,-0.164252794792037,
-10.8864221432573));
#64685=CARTESIAN_POINT('Ctrl Pts',(0.703996001259478,0.0257198981063917,
-10.8772106310344));
#64686=CARTESIAN_POINT('Ctrl Pts',(0.663833148899857,0.235791079919573,
-10.8679991188115));
#64687=CARTESIAN_POINT('Ctrl Pts',(0.549573659945365,0.394831207345944,
-10.8587876065886));
#64688=CARTESIAN_POINT('Ctrl Pts',(0.435314170990874,0.553871334772315,
-10.8495760943657));
#64689=CARTESIAN_POINT('Ctrl Pts',(0.249045211078671,0.658975239130211,
-10.8403645821428));
#64690=CARTESIAN_POINT('Ctrl Pts',(0.0538369544966078,0.674555018015974,
-10.8311530699199));
#64691=CARTESIAN_POINT('Ctrl Pts',(-0.141371302085456,0.690134796901736,
-10.821941557697));
#64692=CARTESIAN_POINT('Ctrl Pts',(-0.341953007380628,0.615905856191741,
-10.8127300454741));
#64693=CARTESIAN_POINT('Ctrl Pts',(-0.479991729591128,0.47700191773631,
-10.8035185332512));
#64694=CARTESIAN_POINT('Ctrl Pts',(-0.604373796054446,0.351840233910857,
-10.7952183482945));
#64695=CARTESIAN_POINT('Ctrl Pts',(-0.67669999999998,0.17626379960763,-10.7869091724096));
#64696=CARTESIAN_POINT('Ctrl Pts',(-0.6767,7.56050957754512E-14,-10.778617978381));
#64697=CARTESIAN_POINT('Ctrl Pts',(-0.67542960639225,3.4995157066342E-5,
-10.939182021619));
#64698=CARTESIAN_POINT('Ctrl Pts',(-0.675726540320146,-0.0905086959147912,
-10.9349324711344));
#64699=CARTESIAN_POINT('Ctrl Pts',(-0.637546849478435,-0.293800002514061,
-10.9253873878184));
#64700=CARTESIAN_POINT('Ctrl Pts',(-0.437774356145965,-0.551890885522362,
-10.9105467716709));
#64701=CARTESIAN_POINT('Ctrl Pts',(-0.120741175465174,-0.695542481001687,
-10.8946601731765));
#64702=CARTESIAN_POINT('Ctrl Pts',(0.225474399042472,-0.667376348810361,
-10.8787735746821));
#64703=CARTESIAN_POINT('Ctrl Pts',(0.619349525511595,-0.416287328540213,
-10.8575914433563));
#64704=CARTESIAN_POINT('Ctrl Pts',(0.7426298818878,0.0752814793781906,-10.8364093120304));
#64705=CARTESIAN_POINT('Ctrl Pts',(0.513381745134516,0.481322377944037,
-10.8152271807046));
#64706=CARTESIAN_POINT('Ctrl Pts',(0.12503781439124,0.735271763261725,-10.7940450493787));
#64707=CARTESIAN_POINT('Ctrl Pts',(-0.475417762247048,0.628657006331378,
-10.7686966630169));
#64708=CARTESIAN_POINT('Ctrl Pts',(-0.676069829824612,0.199726494404265,
-10.7486438094865));
#64709=CARTESIAN_POINT('Ctrl Pts',(-0.677536220770138,-0.000773839678422372,
-10.739182021619));
#64710=CARTESIAN_POINT('Origin',(0.,0.,-12.278617978381));
#64711=CARTESIAN_POINT('',(-0.677468338356203,7.29499899796481E-5,-11.178617978381));
#64712=CARTESIAN_POINT('',(-0.676834075999803,0.000191052801950281,-11.139182021619));
#64713=CARTESIAN_POINT('',(-0.6767,6.12423655037739E-13,-12.278617978381));
#64714=CARTESIAN_POINT('Ctrl Pts',(-0.677468338356203,7.29499899795568E-5,
-11.178617978381));
#64715=CARTESIAN_POINT('Ctrl Pts',(-0.677463317556368,-0.00346603282166678,
-11.1784508086733));
#64716=CARTESIAN_POINT('Ctrl Pts',(-0.67522084717329,-0.23121412904218,
-11.1676925733027));
#64717=CARTESIAN_POINT('Ctrl Pts',(-0.424197719174421,-0.679330206520831,
-11.1463432722691));
#64718=CARTESIAN_POINT('Ctrl Pts',(0.343160473225332,-0.722994096502876,
-11.1145700752803));
#64719=CARTESIAN_POINT('Ctrl Pts',(0.716133365261885,-0.208402697353022,
-11.088092411123));
#64720=CARTESIAN_POINT('Ctrl Pts',(0.657170405500786,0.253686804061263,
-11.0669102797971));
#64721=CARTESIAN_POINT('Ctrl Pts',(0.456763012508479,0.538261390715488,
-11.0510236813027));
#64722=CARTESIAN_POINT('Ctrl Pts',(0.144077853390088,0.689544391419175,
-11.0351370828084));
#64723=CARTESIAN_POINT('Ctrl Pts',(-0.322724961404119,0.672857766501242,
-11.0139549514825));
#64724=CARTESIAN_POINT('Ctrl Pts',(-0.638930029937868,0.351628493840238,
-10.9951152500067));
#64725=CARTESIAN_POINT('Ctrl Pts',(-0.6769768490303,0.0634282862764284,
-10.9815710813624));
#64726=CARTESIAN_POINT('Ctrl Pts',(-0.67664771829584,0.000479233537379581,
-10.978617978381));
#64727=CARTESIAN_POINT('Ctrl Pts',(-0.676834075999803,0.000191052801950271,
-11.139182021619));
#64728=CARTESIAN_POINT('Ctrl Pts',(-0.676650335253473,-0.0439955398353917,
-11.1371077312768));
#64729=CARTESIAN_POINT('Ctrl Pts',(-0.660795208169657,-0.201066433598618,
-11.1297379081032));
#64730=CARTESIAN_POINT('Ctrl Pts',(-0.542288925423647,-0.451973998913277,
-11.117072552098));
#64731=CARTESIAN_POINT('Ctrl Pts',(-0.260173180138369,-0.654629522639962,
-11.1011859536036));
#64732=CARTESIAN_POINT('Ctrl Pts',(0.20257790968715,-0.718227794756728,
-11.0800038222778));
#64733=CARTESIAN_POINT('Ctrl Pts',(0.61475932399721,-0.423364401158974,
-11.0588216909519));
#64734=CARTESIAN_POINT('Ctrl Pts',(0.702880058995295,0.0345205795692396,
-11.0376395596261));
#64735=CARTESIAN_POINT('Ctrl Pts',(0.571282631286294,0.479473853373007,
-11.0164574283002));
#64736=CARTESIAN_POINT('Ctrl Pts',(0.0211398831226441,0.800616225032851,
-10.9899797641429));
#64737=CARTESIAN_POINT('Ctrl Pts',(-0.570966914673425,0.496146330447829,
-10.9624561176387));
#64738=CARTESIAN_POINT('Ctrl Pts',(-0.674986498111135,0.135151448844078,
-10.9455235367974));
#64739=CARTESIAN_POINT('Ctrl Pts',(-0.67542960639225,3.4995157066342E-5,
-10.939182021619));
#64740=CARTESIAN_POINT('Origin',(0.,0.,-12.278617978381));
#64741=CARTESIAN_POINT('',(-0.676225509870168,-0.000584572772009204,-11.378617978381));
#64742=CARTESIAN_POINT('',(-0.676899469727254,-2.06163719228738E-5,-11.339182021619));
#64743=CARTESIAN_POINT('',(-0.6767,6.12423655037739E-13,-12.278617978381));
#64744=CARTESIAN_POINT('Ctrl Pts',(-0.676225509870168,-0.000584572772009233,
-11.378617978381));
#64745=CARTESIAN_POINT('Ctrl Pts',(-0.676904850538366,-0.0704961224808199,
-11.3753305359842));
#64746=CARTESIAN_POINT('Ctrl Pts',(-0.635139734798044,-0.365010782622285,
-11.3614520279245));
#64747=CARTESIAN_POINT('Ctrl Pts',(-0.206478220428704,-0.773205223454543,
-11.3369824542018));
#64748=CARTESIAN_POINT('Ctrl Pts',(0.410920283938739,-0.622433291638274,
-11.3105047900445));
#64749=CARTESIAN_POINT('Ctrl Pts',(0.665114014783227,-0.232063101779371,
-11.2893226587187));
#64750=CARTESIAN_POINT('Ctrl Pts',(0.696585389017661,0.11457124582531,-11.2734360602242));
#64751=CARTESIAN_POINT('Ctrl Pts',(0.55619304910803,0.432295255177504,-11.2575494617299));
#64752=CARTESIAN_POINT('Ctrl Pts',(0.189598103717612,0.721762795994409,
-11.236367330404));
#64753=CARTESIAN_POINT('Ctrl Pts',(-0.315180024953703,0.676629880018334,
-11.2151851990782));
#64754=CARTESIAN_POINT('Ctrl Pts',(-0.620884112411212,0.329425838331515,
-11.19417023746));
#64755=CARTESIAN_POINT('Ctrl Pts',(-0.677622364376125,0.10864040037347,
-11.1837463415048));
#64756=CARTESIAN_POINT('Ctrl Pts',(-0.677468338356203,7.29499899795568E-5,
-11.178617978381));
#64757=CARTESIAN_POINT('Ctrl Pts',(-0.676899469727254,-2.06163719228681E-5,
-11.339182021619));
#64758=CARTESIAN_POINT('Ctrl Pts',(-0.676893857161047,-0.110082133649128,
-11.3339874585877));
#64759=CARTESIAN_POINT('Ctrl Pts',(-0.620592612576125,-0.332187875396714,
-11.323497362725));
#64760=CARTESIAN_POINT('Ctrl Pts',(-0.310543480858139,-0.67856592981927,
-11.3024162011993));
#64761=CARTESIAN_POINT('Ctrl Pts',(0.194497940172004,-0.720650396469946,
-11.2812340698734));
#64762=CARTESIAN_POINT('Ctrl Pts',(0.558075706772724,-0.428699840487657,
-11.2600519385476));
#64763=CARTESIAN_POINT('Ctrl Pts',(0.745814935827746,-0.00437062783121209,
-11.2388698072217));
#64764=CARTESIAN_POINT('Ctrl Pts',(0.534393477883215,0.596537379583458,
-11.2123921430644));
#64765=CARTESIAN_POINT('Ctrl Pts',(-0.21411444420791,0.771125527228726,
-11.1806189460756));
#64766=CARTESIAN_POINT('Ctrl Pts',(-0.634097054479883,0.362811161644489,
-11.1562155722605));
#64767=CARTESIAN_POINT('Ctrl Pts',(-0.677119413826939,0.0688100531245896,
-11.1424032641083));
#64768=CARTESIAN_POINT('Ctrl Pts',(-0.676834075999803,0.000191052801950271,
-11.139182021619));
#64769=CARTESIAN_POINT('Origin',(0.,0.,-12.278617978381));
#64770=CARTESIAN_POINT('',(-0.67577016846339,0.000469772489560586,-11.578617978381));
#64771=CARTESIAN_POINT('',(-0.6767,1.01008828037874E-13,-11.539182021619));
#64772=CARTESIAN_POINT('',(-0.6767,6.12423655037739E-13,-12.278617978381));
#64773=CARTESIAN_POINT('Ctrl Pts',(-0.67577016846339,0.000469772489560594,
-11.578617978381));
#64774=CARTESIAN_POINT('Ctrl Pts',(-0.675013010550184,-0.13640120609862,
-11.5722102632951));
#64775=CARTESIAN_POINT('Ctrl Pts',(-0.56814302722758,-0.500655806665067,
-11.5552114825463));
#64776=CARTESIAN_POINT('Ctrl Pts',(-0.0897337187244002,-0.740423380881239,
-11.532917168966));
#64777=CARTESIAN_POINT('Ctrl Pts',(0.356717037324203,-0.607439441065005,
-11.5117350376402));
#64778=CARTESIAN_POINT('Ctrl Pts',(0.605099039586646,-0.36361113891817,
-11.4958484391458));
#64779=CARTESIAN_POINT('Ctrl Pts',(0.703772576709861,-0.0305614200295496,
-11.4799618406514));
#64780=CARTESIAN_POINT('Ctrl Pts',(0.611744859212238,0.427384163050785,
-11.4587797093255));
#64781=CARTESIAN_POINT('Ctrl Pts',(0.197790656500237,0.719753643173289,
-11.4375975779997));
#64782=CARTESIAN_POINT('Ctrl Pts',(-0.263619000263347,0.652485296666156,
-11.4164154466738));
#64783=CARTESIAN_POINT('Ctrl Pts',(-0.58209335344289,0.423941526590339,
-11.3985207577448));
#64784=CARTESIAN_POINT('Ctrl Pts',(-0.674716236790673,0.154736056274489,
-11.3859216016471));
#64785=CARTESIAN_POINT('Ctrl Pts',(-0.676225509870168,-0.000584572772009233,
-11.378617978381));
#64786=CARTESIAN_POINT('Ctrl Pts',(-0.676859540333324,-0.000246342469780166,
-11.539182021619));
#64787=CARTESIAN_POINT('Ctrl Pts',(-0.677143312751866,-0.0646519608093662,
-11.5361627187301));
#64788=CARTESIAN_POINT('Ctrl Pts',(-0.637526896910174,-0.354745471226495,
-11.5225523501783));
#64789=CARTESIAN_POINT('Ctrl Pts',(-0.318270223098515,-0.675181839024747,
-11.5036464487949));
#64790=CARTESIAN_POINT('Ctrl Pts',(0.147840292895422,-0.688022737605352,
-11.4824643174691));
#64791=CARTESIAN_POINT('Ctrl Pts',(0.565623962158729,-0.486136361723975,
-11.4612821861432));
#64792=CARTESIAN_POINT('Ctrl Pts',(0.793479716880401,0.108734401743206,
-11.4348045219859));
#64793=CARTESIAN_POINT('Ctrl Pts',(0.335993916742615,0.726352298131389,
-11.4030313249971));
#64794=CARTESIAN_POINT('Ctrl Pts',(-0.298112918637422,0.683671975462962,
-11.3765536608398));
#64795=CARTESIAN_POINT('Ctrl Pts',(-0.615475022766798,0.342666648827597,
-11.3553715295139));
#64796=CARTESIAN_POINT('Ctrl Pts',(-0.67634254234158,0.116460459871167,
-11.3446794940508));
#64797=CARTESIAN_POINT('Ctrl Pts',(-0.67689957882203,0.00211871456710879,
-11.3392829914192));
#64798=CARTESIAN_POINT('Ctrl Pts',(-0.676899469727254,-2.06163719228681E-5,
-11.339182021619));
#64799=CARTESIAN_POINT('Origin',(0.,0.,-12.278617978381));
#64800=CARTESIAN_POINT('',(-0.677716351375759,0.000193615723412327,-11.778617978381));
#64801=CARTESIAN_POINT('',(-0.6767,9.60347966456048E-14,-11.739182021619));
#64802=CARTESIAN_POINT('',(-0.6767,6.12423655037739E-13,-12.278617978381));
#64803=CARTESIAN_POINT('Ctrl Pts',(-0.677716351375759,0.000193615723412331,
-11.778617978381));
#64804=CARTESIAN_POINT('Ctrl Pts',(-0.676288025918613,-0.201313555190218,
-11.769089990606));
#64805=CARTESIAN_POINT('Ctrl Pts',(-0.526186147067614,-0.515751982643562,
-11.7542664699996));
#64806=CARTESIAN_POINT('Ctrl Pts',(-0.121403177164881,-0.693866619017976,
-11.7341474165617));
#64807=CARTESIAN_POINT('Ctrl Pts',(0.225850498452994,-0.668875211131948,
-11.7182608180673));
#64808=CARTESIAN_POINT('Ctrl Pts',(0.516608588870761,-0.478872034799853,
-11.7023742195729));
#64809=CARTESIAN_POINT('Ctrl Pts',(0.742947756127913,-0.0702747149864332,
-11.681192088247));
#64810=CARTESIAN_POINT('Ctrl Pts',(0.616681960998304,0.420553527772077,
-11.6600099569212));
#64811=CARTESIAN_POINT('Ctrl Pts',(0.221462490922912,0.667971079462276,
-11.6388278255953));
#64812=CARTESIAN_POINT('Ctrl Pts',(-0.241001769318581,0.705818539717338,
-11.6176456942695));
#64813=CARTESIAN_POINT('Ctrl Pts',(-0.618508626704561,0.404758836325352,
-11.597575745198));
#64814=CARTESIAN_POINT('Ctrl Pts',(-0.676264487725508,0.0898275668955524,
-11.582801328958));
#64815=CARTESIAN_POINT('Ctrl Pts',(-0.67577016846339,0.000469772489560594,
-11.578617978381));
#64816=CARTESIAN_POINT('Ctrl Pts',(-0.6767,8.52162505866054E-14,-11.739182021619));
#64817=CARTESIAN_POINT('Ctrl Pts',(-0.676700000000021,-0.167912749481023,
-11.731283648902));
#64818=CARTESIAN_POINT('Ctrl Pts',(-0.611309698394134,-0.335389744095952,
-11.723366169419));
#64819=CARTESIAN_POINT('Ctrl Pts',(-0.497294271809351,-0.458934959689941,
-11.715458243319));
#64820=CARTESIAN_POINT('Ctrl Pts',(-0.364483913909809,-0.602846049542439,
-11.7062467310961));
#64821=CARTESIAN_POINT('Ctrl Pts',(-0.16678284882323,-0.684437991556829,
-11.6970352188731));
#64822=CARTESIAN_POINT('Ctrl Pts',(0.028867868763758,-0.676083971229195,
-11.6878237066502));
#64823=CARTESIAN_POINT('Ctrl Pts',(0.224518586350746,-0.667729950901561,
-11.6786121944273));
#64824=CARTESIAN_POINT('Ctrl Pts',(0.414545026094418,-0.56958257021113,
-11.6694006822044));
#64825=CARTESIAN_POINT('Ctrl Pts',(0.534604741032153,-0.414874271154461,
-11.6601891699815));
#64826=CARTESIAN_POINT('Ctrl Pts',(0.654664455969888,-0.260165972097792,
-11.6509776577586));
#64827=CARTESIAN_POINT('Ctrl Pts',(0.702564328368376,-0.0517227943196359,
-11.6417661455357));
#64828=CARTESIAN_POINT('Ctrl Pts',(0.662085588863346,0.139876956713662,
-11.6325546333128));
#64829=CARTESIAN_POINT('Ctrl Pts',(0.621606849358317,0.331476707746961,
-11.6233431210899));
#64830=CARTESIAN_POINT('Ctrl Pts',(0.493488918674505,0.502733100256395,
-11.614131608867));
#64831=CARTESIAN_POINT('Ctrl Pts',(0.321112187304428,0.595659175338184,
-11.6049200966441));
#64832=CARTESIAN_POINT('Ctrl Pts',(0.148735455934352,0.688585250419974,
-11.5957085844212));
#64833=CARTESIAN_POINT('Ctrl Pts',(-0.0647512891489894,0.701483537584085,
-11.5864970721983));
#64834=CARTESIAN_POINT('Ctrl Pts',(-0.24706200400731,0.629986711110554,
-11.5772855599754));
#64835=CARTESIAN_POINT('Ctrl Pts',(-0.42937271886563,0.558489884637023,
-11.5680740477525));
#64836=CARTESIAN_POINT('Ctrl Pts',(-0.577177153531771,0.403903969266088,
-11.5588625355295));
#64837=CARTESIAN_POINT('Ctrl Pts',(-0.640429119637554,0.218571344691539,
-11.5496510233066));
#64838=CARTESIAN_POINT('Ctrl Pts',(-0.664391342990392,0.148360377064131,
-11.5461613560774));
#64839=CARTESIAN_POINT('Ctrl Pts',(-0.676699999999989,0.0741494619493284,
-11.5426699049933));
#64840=CARTESIAN_POINT('Ctrl Pts',(-0.6767,1.0100878303629E-13,-11.539182021619));
#64841=CARTESIAN_POINT('Ctrl Pts',(-0.292633023485541,-0.00545700788497927,
1.));
#64842=CARTESIAN_POINT('Ctrl Pts',(-0.292633023485541,-0.00545700788497927,
0.96));
#64843=CARTESIAN_POINT('Ctrl Pts',(-0.335948136076331,-0.00545700788497927,
1.));
#64844=CARTESIAN_POINT('Ctrl Pts',(-0.335948136076331,-0.00545700788497927,
0.96));
#64845=CARTESIAN_POINT('Ctrl Pts',(-0.364426996931434,-0.0341063976287842,
1.));
#64846=CARTESIAN_POINT('Ctrl Pts',(-0.364426996931434,-0.0341063976287842,
0.96));
#64847=CARTESIAN_POINT('',(-0.292633023485541,-0.00545700788497927,1.));
#64848=CARTESIAN_POINT('',(-0.364426996931434,-0.0341063976287842,1.));
#64849=CARTESIAN_POINT('Ctrl Pts',(-0.292633023485541,-0.00545700788497927,
1.));
#64850=CARTESIAN_POINT('Ctrl Pts',(-0.335948136076331,-0.00545700788497927,
1.));
#64851=CARTESIAN_POINT('Ctrl Pts',(-0.364426996931434,-0.0341063976287842,
1.));
#64852=CARTESIAN_POINT('',(-0.292633023485541,-0.00545700788497927,0.96));
#64853=CARTESIAN_POINT('',(-0.292633023485541,-0.00545700788497927,1.));
#64854=CARTESIAN_POINT('',(-0.364426996931434,-0.0341063976287842,0.96));
#64855=CARTESIAN_POINT('Ctrl Pts',(-0.292633023485541,-0.00545700788497927,
0.96));
#64856=CARTESIAN_POINT('Ctrl Pts',(-0.335948136076331,-0.00545700788497927,
0.96));
#64857=CARTESIAN_POINT('Ctrl Pts',(-0.364426996931434,-0.0341063976287842,
0.96));
#64858=CARTESIAN_POINT('',(-0.364426996931434,-0.0341063976287842,1.));
#64859=CARTESIAN_POINT('Ctrl Pts',(-0.218792613968253,-0.034447455406189,
1.));
#64860=CARTESIAN_POINT('Ctrl Pts',(-0.218792613968253,-0.034447455406189,
0.96));
#64861=CARTESIAN_POINT('Ctrl Pts',(-0.248294677957892,-0.00545700788497927,
1.));
#64862=CARTESIAN_POINT('Ctrl Pts',(-0.248294677957892,-0.00545700788497927,
0.96));
#64863=CARTESIAN_POINT('Ctrl Pts',(-0.292633023485541,-0.00545700788497927,
1.));
#64864=CARTESIAN_POINT('Ctrl Pts',(-0.292633023485541,-0.00545700788497927,
0.96));
#64865=CARTESIAN_POINT('',(-0.218792613968253,-0.034447455406189,1.));
#64866=CARTESIAN_POINT('Ctrl Pts',(-0.218792613968253,-0.034447455406189,
1.));
#64867=CARTESIAN_POINT('Ctrl Pts',(-0.248294677957892,-0.00545700788497927,
1.));
#64868=CARTESIAN_POINT('Ctrl Pts',(-0.292633023485541,-0.00545700788497927,
1.));
#64869=CARTESIAN_POINT('',(-0.218792613968253,-0.034447455406189,0.96));
#64870=CARTESIAN_POINT('',(-0.218792613968253,-0.034447455406189,1.));
#64871=CARTESIAN_POINT('Ctrl Pts',(-0.218792613968253,-0.034447455406189,
0.96));
#64872=CARTESIAN_POINT('Ctrl Pts',(-0.248294677957892,-0.00545700788497927,
0.96));
#64873=CARTESIAN_POINT('Ctrl Pts',(-0.292633023485541,-0.00545700788497927,
0.96));
#64874=CARTESIAN_POINT('Ctrl Pts',(-0.189290579780936,-0.107776248455048,
1.));
#64875=CARTESIAN_POINT('Ctrl Pts',(-0.189290579780936,-0.107776248455048,
0.96));
#64876=CARTESIAN_POINT('Ctrl Pts',(-0.189290579780936,-0.0634379029273987,
1.));
#64877=CARTESIAN_POINT('Ctrl Pts',(-0.189290579780936,-0.0634379029273987,
0.96));
#64878=CARTESIAN_POINT('Ctrl Pts',(-0.218792613968253,-0.034447455406189,
1.));
#64879=CARTESIAN_POINT('Ctrl Pts',(-0.218792613968253,-0.034447455406189,
0.96));
#64880=CARTESIAN_POINT('',(-0.189290579780936,-0.107776248455048,1.));
#64881=CARTESIAN_POINT('Ctrl Pts',(-0.189290579780936,-0.107776248455048,
1.));
#64882=CARTESIAN_POINT('Ctrl Pts',(-0.189290579780936,-0.0634379029273987,
1.));
#64883=CARTESIAN_POINT('Ctrl Pts',(-0.218792613968253,-0.034447455406189,
1.));
#64884=CARTESIAN_POINT('',(-0.189290579780936,-0.107776248455048,0.96));
#64885=CARTESIAN_POINT('',(-0.189290579780936,-0.107776248455048,1.));
#64886=CARTESIAN_POINT('Ctrl Pts',(-0.189290579780936,-0.107776248455048,
0.96));
#64887=CARTESIAN_POINT('Ctrl Pts',(-0.189290579780936,-0.0634379029273987,
0.96));
#64888=CARTESIAN_POINT('Ctrl Pts',(-0.218792613968253,-0.034447455406189,
0.96));
#64889=CARTESIAN_POINT('Ctrl Pts',(-0.217939969524741,-0.179740750789642,
1.));
#64890=CARTESIAN_POINT('Ctrl Pts',(-0.217939969524741,-0.179740750789642,
0.96));
#64891=CARTESIAN_POINT('Ctrl Pts',(-0.189290579780936,-0.151432418823242,
1.));
#64892=CARTESIAN_POINT('Ctrl Pts',(-0.189290579780936,-0.151432418823242,
0.96));
#64893=CARTESIAN_POINT('Ctrl Pts',(-0.189290579780936,-0.107776248455048,
1.));
#64894=CARTESIAN_POINT('Ctrl Pts',(-0.189290579780936,-0.107776248455048,
0.96));
#64895=CARTESIAN_POINT('',(-0.217939969524741,-0.179740750789642,1.));
#64896=CARTESIAN_POINT('Ctrl Pts',(-0.217939969524741,-0.179740750789642,
1.));
#64897=CARTESIAN_POINT('Ctrl Pts',(-0.189290579780936,-0.151432418823242,
1.));
#64898=CARTESIAN_POINT('Ctrl Pts',(-0.189290579780936,-0.107776248455048,
1.));
#64899=CARTESIAN_POINT('',(-0.217939969524741,-0.179740750789642,0.96));
#64900=CARTESIAN_POINT('',(-0.217939969524741,-0.179740750789642,1.));
#64901=CARTESIAN_POINT('Ctrl Pts',(-0.217939969524741,-0.179740750789642,
0.96));
#64902=CARTESIAN_POINT('Ctrl Pts',(-0.189290579780936,-0.151432418823242,
0.96));
#64903=CARTESIAN_POINT('Ctrl Pts',(-0.189290579780936,-0.107776248455048,
0.96));
#64904=CARTESIAN_POINT('Ctrl Pts',(-0.290586617216468,-0.208049082756043,
1.));
#64905=CARTESIAN_POINT('Ctrl Pts',(-0.290586617216468,-0.208049082756043,
0.96));
#64906=CARTESIAN_POINT('Ctrl Pts',(-0.246589359268546,-0.208049082756043,
1.));
#64907=CARTESIAN_POINT('Ctrl Pts',(-0.246589359268546,-0.208049082756043,
0.96));
#64908=CARTESIAN_POINT('Ctrl Pts',(-0.217939969524741,-0.179740750789642,
1.));
#64909=CARTESIAN_POINT('Ctrl Pts',(-0.217939969524741,-0.179740750789642,
0.96));
#64910=CARTESIAN_POINT('',(-0.290586617216468,-0.208049082756043,1.));
#64911=CARTESIAN_POINT('Ctrl Pts',(-0.290586617216468,-0.208049082756043,
1.));
#64912=CARTESIAN_POINT('Ctrl Pts',(-0.246589359268546,-0.208049082756043,
1.));
#64913=CARTESIAN_POINT('Ctrl Pts',(-0.217939969524741,-0.179740750789642,
1.));
#64914=CARTESIAN_POINT('',(-0.290586617216468,-0.208049082756043,0.96));
#64915=CARTESIAN_POINT('',(-0.290586617216468,-0.208049082756043,1.));
#64916=CARTESIAN_POINT('Ctrl Pts',(-0.290586617216468,-0.208049082756043,
0.96));
#64917=CARTESIAN_POINT('Ctrl Pts',(-0.246589359268546,-0.208049082756043,
0.96));
#64918=CARTESIAN_POINT('Ctrl Pts',(-0.217939969524741,-0.179740750789642,
0.96));
#64919=CARTESIAN_POINT('Ctrl Pts',(-0.343451556190848,-0.194577062129974,
1.));
#64920=CARTESIAN_POINT('Ctrl Pts',(-0.343451556190848,-0.194577062129974,
0.96));
#64921=CARTESIAN_POINT('Ctrl Pts',(-0.318894949182868,-0.208049082756043,
1.));
#64922=CARTESIAN_POINT('Ctrl Pts',(-0.318894949182868,-0.208049082756043,
0.96));
#64923=CARTESIAN_POINT('Ctrl Pts',(-0.290586617216468,-0.208049082756043,
1.));
#64924=CARTESIAN_POINT('Ctrl Pts',(-0.290586617216468,-0.208049082756043,
0.96));
#64925=CARTESIAN_POINT('',(-0.343451556190848,-0.194577062129974,1.));
#64926=CARTESIAN_POINT('Ctrl Pts',(-0.343451556190848,-0.194577062129974,
1.));
#64927=CARTESIAN_POINT('Ctrl Pts',(-0.318894949182868,-0.208049082756043,
1.));
#64928=CARTESIAN_POINT('Ctrl Pts',(-0.290586617216468,-0.208049082756043,
1.));
#64929=CARTESIAN_POINT('',(-0.343451556190848,-0.194577062129974,0.96));
#64930=CARTESIAN_POINT('',(-0.343451556190848,-0.194577062129974,1.));
#64931=CARTESIAN_POINT('Ctrl Pts',(-0.343451556190848,-0.194577062129974,
0.96));
#64932=CARTESIAN_POINT('Ctrl Pts',(-0.318894949182868,-0.208049082756043,
0.96));
#64933=CARTESIAN_POINT('Ctrl Pts',(-0.290586617216468,-0.208049082756043,
0.96));
#64934=CARTESIAN_POINT('Ctrl Pts',(-0.380457010492682,-0.156548404693604,
1.));
#64935=CARTESIAN_POINT('Ctrl Pts',(-0.380457010492682,-0.156548404693604,
0.96));
#64936=CARTESIAN_POINT('Ctrl Pts',(-0.368008163198829,-0.181104981899261,
1.));
#64937=CARTESIAN_POINT('Ctrl Pts',(-0.368008163198829,-0.181104981899261,
0.96));
#64938=CARTESIAN_POINT('Ctrl Pts',(-0.343451556190848,-0.194577062129974,
1.));
#64939=CARTESIAN_POINT('Ctrl Pts',(-0.343451556190848,-0.194577062129974,
0.96));
#64940=CARTESIAN_POINT('',(-0.380457010492682,-0.156548404693604,1.));
#64941=CARTESIAN_POINT('Ctrl Pts',(-0.380457010492682,-0.156548404693604,
1.));
#64942=CARTESIAN_POINT('Ctrl Pts',(-0.368008163198829,-0.181104981899261,
1.));
#64943=CARTESIAN_POINT('Ctrl Pts',(-0.343451556190848,-0.194577062129974,
1.));
#64944=CARTESIAN_POINT('',(-0.380457010492682,-0.156548404693604,0.96));
#64945=CARTESIAN_POINT('',(-0.380457010492682,-0.156548404693604,1.));
#64946=CARTESIAN_POINT('Ctrl Pts',(-0.380457010492682,-0.156548404693604,
0.96));
#64947=CARTESIAN_POINT('Ctrl Pts',(-0.368008163198829,-0.181104981899261,
0.96));
#64948=CARTESIAN_POINT('Ctrl Pts',(-0.343451556190848,-0.194577062129974,
0.96));
#64949=CARTESIAN_POINT('Ctrl Pts',(-0.392905857786536,-0.105729842185974,
1.));
#64950=CARTESIAN_POINT('Ctrl Pts',(-0.392905857786536,-0.105729842185974,
0.96));
#64951=CARTESIAN_POINT('Ctrl Pts',(-0.392905857786536,-0.131991767883301,
1.));
#64952=CARTESIAN_POINT('Ctrl Pts',(-0.392905857786536,-0.131991767883301,
0.96));
#64953=CARTESIAN_POINT('Ctrl Pts',(-0.380457010492682,-0.156548404693604,
1.));
#64954=CARTESIAN_POINT('Ctrl Pts',(-0.380457010492682,-0.156548404693604,
0.96));
#64955=CARTESIAN_POINT('',(-0.392905857786536,-0.105729842185974,1.));
#64956=CARTESIAN_POINT('Ctrl Pts',(-0.392905857786536,-0.105729842185974,
1.));
#64957=CARTESIAN_POINT('Ctrl Pts',(-0.392905857786536,-0.131991767883301,
1.));
#64958=CARTESIAN_POINT('Ctrl Pts',(-0.380457010492682,-0.156548404693604,
1.));
#64959=CARTESIAN_POINT('',(-0.392905857786536,-0.105729842185974,0.96));
#64960=CARTESIAN_POINT('',(-0.392905857786536,-0.105729842185974,1.));
#64961=CARTESIAN_POINT('Ctrl Pts',(-0.392905857786536,-0.105729842185974,
0.96));
#64962=CARTESIAN_POINT('Ctrl Pts',(-0.392905857786536,-0.131991767883301,
0.96));
#64963=CARTESIAN_POINT('Ctrl Pts',(-0.380457010492682,-0.156548404693604,
0.96));
#64964=CARTESIAN_POINT('Ctrl Pts',(-0.364426996931434,-0.0341063976287842,
1.));
#64965=CARTESIAN_POINT('Ctrl Pts',(-0.364426996931434,-0.0341063976287842,
0.96));
#64966=CARTESIAN_POINT('Ctrl Pts',(-0.392905857786536,-0.0627557873725891,
1.));
#64967=CARTESIAN_POINT('Ctrl Pts',(-0.392905857786536,-0.0627557873725891,
0.96));
#64968=CARTESIAN_POINT('Ctrl Pts',(-0.392905857786536,-0.105729842185974,
1.));
#64969=CARTESIAN_POINT('Ctrl Pts',(-0.392905857786536,-0.105729842185974,
0.96));
#64970=CARTESIAN_POINT('Ctrl Pts',(-0.364426996931434,-0.0341063976287842,
1.));
#64971=CARTESIAN_POINT('Ctrl Pts',(-0.392905857786536,-0.0627557873725891,
1.));
#64972=CARTESIAN_POINT('Ctrl Pts',(-0.392905857786536,-0.105729842185974,
1.));
#64973=CARTESIAN_POINT('Ctrl Pts',(-0.364426996931434,-0.0341063976287842,
0.96));
#64974=CARTESIAN_POINT('Ctrl Pts',(-0.392905857786536,-0.0627557873725891,
0.96));
#64975=CARTESIAN_POINT('Ctrl Pts',(-0.392905857786536,-0.105729842185974,
0.96));
#64976=CARTESIAN_POINT('Ctrl Pts',(-0.291609820351005,0.201568937301636,
1.));
#64977=CARTESIAN_POINT('Ctrl Pts',(-0.291609820351005,0.201568937301636,
0.96));
#64978=CARTESIAN_POINT('Ctrl Pts',(-0.32673942707479,0.201568937301636,
1.));
#64979=CARTESIAN_POINT('Ctrl Pts',(-0.32673942707479,0.201568937301636,
0.96));
#64980=CARTESIAN_POINT('Ctrl Pts',(-0.349931773170829,0.179058706760406,
1.));
#64981=CARTESIAN_POINT('Ctrl Pts',(-0.349931773170829,0.179058706760406,
0.96));
#64982=CARTESIAN_POINT('',(-0.291609820351005,0.201568937301636,1.));
#64983=CARTESIAN_POINT('',(-0.349931773170829,0.179058706760406,1.));
#64984=CARTESIAN_POINT('Ctrl Pts',(-0.291609820351005,0.201568937301636,
1.));
#64985=CARTESIAN_POINT('Ctrl Pts',(-0.32673942707479,0.201568937301636,
1.));
#64986=CARTESIAN_POINT('Ctrl Pts',(-0.349931773170829,0.179058706760406,
1.));
#64987=CARTESIAN_POINT('',(-0.291609820351005,0.201568937301636,0.96));
#64988=CARTESIAN_POINT('',(-0.291609820351005,0.201568937301636,1.));
#64989=CARTESIAN_POINT('',(-0.349931773170829,0.179058706760406,0.96));
#64990=CARTESIAN_POINT('Ctrl Pts',(-0.291609820351005,0.201568937301636,
0.96));
#64991=CARTESIAN_POINT('Ctrl Pts',(-0.32673942707479,0.201568937301636,
0.96));
#64992=CARTESIAN_POINT('Ctrl Pts',(-0.349931773170829,0.179058706760406,
0.96));
#64993=CARTESIAN_POINT('',(-0.349931773170829,0.179058706760406,1.));
#64994=CARTESIAN_POINT('Ctrl Pts',(-0.23345836661756,0.178547120094299,
1.));
#64995=CARTESIAN_POINT('Ctrl Pts',(-0.23345836661756,0.178547120094299,
0.96));
#64996=CARTESIAN_POINT('Ctrl Pts',(-0.256821271404624,0.201568937301636,
1.));
#64997=CARTESIAN_POINT('Ctrl Pts',(-0.256821271404624,0.201568937301636,
0.96));
#64998=CARTESIAN_POINT('Ctrl Pts',(-0.291609820351005,0.201568937301636,
1.));
#64999=CARTESIAN_POINT('Ctrl Pts',(-0.291609820351005,0.201568937301636,
0.96));
#65000=CARTESIAN_POINT('',(-0.23345836661756,0.178547120094299,1.));
#65001=CARTESIAN_POINT('Ctrl Pts',(-0.23345836661756,0.178547120094299,
1.));
#65002=CARTESIAN_POINT('Ctrl Pts',(-0.256821271404624,0.201568937301636,
1.));
#65003=CARTESIAN_POINT('Ctrl Pts',(-0.291609820351005,0.201568937301636,
1.));
#65004=CARTESIAN_POINT('',(-0.23345836661756,0.178547120094299,0.96));
#65005=CARTESIAN_POINT('',(-0.23345836661756,0.178547120094299,1.));
#65006=CARTESIAN_POINT('Ctrl Pts',(-0.23345836661756,0.178547120094299,
0.96));
#65007=CARTESIAN_POINT('Ctrl Pts',(-0.256821271404624,0.201568937301636,
0.96));
#65008=CARTESIAN_POINT('Ctrl Pts',(-0.291609820351005,0.201568937301636,
0.96));
#65009=CARTESIAN_POINT('Ctrl Pts',(-0.210095491632819,0.121759927272797,
1.));
#65010=CARTESIAN_POINT('Ctrl Pts',(-0.210095491632819,0.121759927272797,
0.96));
#65011=CARTESIAN_POINT('Ctrl Pts',(-0.210095491632819,0.15552527308464,
1.));
#65012=CARTESIAN_POINT('Ctrl Pts',(-0.210095491632819,0.15552527308464,
0.96));
#65013=CARTESIAN_POINT('Ctrl Pts',(-0.23345836661756,0.178547120094299,
1.));
#65014=CARTESIAN_POINT('Ctrl Pts',(-0.23345836661756,0.178547120094299,
0.96));
#65015=CARTESIAN_POINT('',(-0.210095491632819,0.121759927272797,1.));
#65016=CARTESIAN_POINT('Ctrl Pts',(-0.210095491632819,0.121759927272797,
1.));
#65017=CARTESIAN_POINT('Ctrl Pts',(-0.210095491632819,0.15552527308464,
1.));
#65018=CARTESIAN_POINT('Ctrl Pts',(-0.23345836661756,0.178547120094299,
1.));
#65019=CARTESIAN_POINT('',(-0.210095491632819,0.121759927272797,0.96));
#65020=CARTESIAN_POINT('',(-0.210095491632819,0.121759927272797,1.));
#65021=CARTESIAN_POINT('Ctrl Pts',(-0.210095491632819,0.121759927272797,
0.96));
#65022=CARTESIAN_POINT('Ctrl Pts',(-0.210095491632819,0.15552527308464,
0.96));
#65023=CARTESIAN_POINT('Ctrl Pts',(-0.23345836661756,0.178547120094299,
0.96));
#65024=CARTESIAN_POINT('Ctrl Pts',(-0.232776251062751,0.0670191407203674,
1.));
#65025=CARTESIAN_POINT('Ctrl Pts',(-0.232776251062751,0.0670191407203674,
0.96));
#65026=CARTESIAN_POINT('Ctrl Pts',(-0.210095491632819,0.0893588423728943,
1.));
#65027=CARTESIAN_POINT('Ctrl Pts',(-0.210095491632819,0.0893588423728943,
0.96));
#65028=CARTESIAN_POINT('Ctrl Pts',(-0.210095491632819,0.121759927272797,
1.));
#65029=CARTESIAN_POINT('Ctrl Pts',(-0.210095491632819,0.121759927272797,
0.96));
#65030=CARTESIAN_POINT('',(-0.232776251062751,0.0670191407203674,1.));
#65031=CARTESIAN_POINT('Ctrl Pts',(-0.232776251062751,0.0670191407203674,
1.));
#65032=CARTESIAN_POINT('Ctrl Pts',(-0.210095491632819,0.0893588423728943,
1.));
#65033=CARTESIAN_POINT('Ctrl Pts',(-0.210095491632819,0.121759927272797,
1.));
#65034=CARTESIAN_POINT('',(-0.232776251062751,0.0670191407203674,0.96));
#65035=CARTESIAN_POINT('',(-0.232776251062751,0.0670191407203674,1.));
#65036=CARTESIAN_POINT('Ctrl Pts',(-0.232776251062751,0.0670191407203674,
0.96));
#65037=CARTESIAN_POINT('Ctrl Pts',(-0.210095491632819,0.0893588423728943,
0.96));
#65038=CARTESIAN_POINT('Ctrl Pts',(-0.210095491632819,0.121759927272797,
0.96));
#65039=CARTESIAN_POINT('Ctrl Pts',(-0.290927674993873,0.0446794390678406,
1.));
#65040=CARTESIAN_POINT('Ctrl Pts',(-0.290927674993873,0.0446794390678406,
0.96));
#65041=CARTESIAN_POINT('Ctrl Pts',(-0.255457010492682,0.0446794390678406,
1.));
#65042=CARTESIAN_POINT('Ctrl Pts',(-0.255457010492682,0.0446794390678406,
0.96));
#65043=CARTESIAN_POINT('Ctrl Pts',(-0.232776251062751,0.0670191407203674,
1.));
#65044=CARTESIAN_POINT('Ctrl Pts',(-0.232776251062751,0.0670191407203674,
0.96));
#65045=CARTESIAN_POINT('',(-0.290927674993873,0.0446794390678406,1.));
#65046=CARTESIAN_POINT('Ctrl Pts',(-0.290927674993873,0.0446794390678406,
1.));
#65047=CARTESIAN_POINT('Ctrl Pts',(-0.255457010492682,0.0446794390678406,
1.));
#65048=CARTESIAN_POINT('Ctrl Pts',(-0.232776251062751,0.0670191407203674,
1.));
#65049=CARTESIAN_POINT('',(-0.290927674993873,0.0446794390678406,0.96));
#65050=CARTESIAN_POINT('',(-0.290927674993873,0.0446794390678406,1.));
#65051=CARTESIAN_POINT('Ctrl Pts',(-0.290927674993873,0.0446794390678406,
0.96));
#65052=CARTESIAN_POINT('Ctrl Pts',(-0.255457010492682,0.0446794390678406,
0.96));
#65053=CARTESIAN_POINT('Ctrl Pts',(-0.232776251062751,0.0670191407203674,
0.96));
#65054=CARTESIAN_POINT('Ctrl Pts',(-0.350272860750556,0.0671896696090698,
1.));
#65055=CARTESIAN_POINT('Ctrl Pts',(-0.350272860750556,0.0671896696090698,
0.96));
#65056=CARTESIAN_POINT('Ctrl Pts',(-0.3274215426296,0.0446794390678406,
1.));
#65057=CARTESIAN_POINT('Ctrl Pts',(-0.3274215426296,0.0446794390678406,
0.96));
#65058=CARTESIAN_POINT('Ctrl Pts',(-0.290927674993873,0.0446794390678406,
1.));
#65059=CARTESIAN_POINT('Ctrl Pts',(-0.290927674993873,0.0446794390678406,
0.96));
#65060=CARTESIAN_POINT('',(-0.350272860750556,0.0671896696090698,1.));
#65061=CARTESIAN_POINT('Ctrl Pts',(-0.350272860750556,0.0671896696090698,
1.));
#65062=CARTESIAN_POINT('Ctrl Pts',(-0.3274215426296,0.0446794390678406,
1.));
#65063=CARTESIAN_POINT('Ctrl Pts',(-0.290927674993873,0.0446794390678406,
1.));
#65064=CARTESIAN_POINT('',(-0.350272860750556,0.0671896696090698,0.96));
#65065=CARTESIAN_POINT('',(-0.350272860750556,0.0671896696090698,1.));
#65066=CARTESIAN_POINT('Ctrl Pts',(-0.350272860750556,0.0671896696090698,
0.96));
#65067=CARTESIAN_POINT('Ctrl Pts',(-0.3274215426296,0.0446794390678406,
0.96));
#65068=CARTESIAN_POINT('Ctrl Pts',(-0.290927674993873,0.0446794390678406,
0.96));
#65069=CARTESIAN_POINT('Ctrl Pts',(-0.37312414906919,0.125170594453812,
1.));
#65070=CARTESIAN_POINT('Ctrl Pts',(-0.37312414906919,0.125170594453812,
0.96));
#65071=CARTESIAN_POINT('Ctrl Pts',(-0.37312414906919,0.0896999001502991,
1.));
#65072=CARTESIAN_POINT('Ctrl Pts',(-0.37312414906919,0.0896999001502991,
0.96));
#65073=CARTESIAN_POINT('Ctrl Pts',(-0.350272860750556,0.0671896696090698,
1.));
#65074=CARTESIAN_POINT('Ctrl Pts',(-0.350272860750556,0.0671896696090698,
0.96));
#65075=CARTESIAN_POINT('',(-0.37312414906919,0.125170594453812,1.));
#65076=CARTESIAN_POINT('Ctrl Pts',(-0.37312414906919,0.125170594453812,
1.));
#65077=CARTESIAN_POINT('Ctrl Pts',(-0.37312414906919,0.0896999001502991,
1.));
#65078=CARTESIAN_POINT('Ctrl Pts',(-0.350272860750556,0.0671896696090698,
1.));
#65079=CARTESIAN_POINT('',(-0.37312414906919,0.125170594453812,0.96));
#65080=CARTESIAN_POINT('',(-0.37312414906919,0.125170594453812,1.));
#65081=CARTESIAN_POINT('Ctrl Pts',(-0.37312414906919,0.125170594453812,
0.96));
#65082=CARTESIAN_POINT('Ctrl Pts',(-0.37312414906919,0.0896999001502991,
0.96));
#65083=CARTESIAN_POINT('Ctrl Pts',(-0.350272860750556,0.0671896696090698,
0.96));
#65084=CARTESIAN_POINT('Ctrl Pts',(-0.349931773170829,0.179058706760406,
1.));
#65085=CARTESIAN_POINT('Ctrl Pts',(-0.349931773170829,0.179058706760406,
0.96));
#65086=CARTESIAN_POINT('Ctrl Pts',(-0.37312414906919,0.156548476219177,
1.));
#65087=CARTESIAN_POINT('Ctrl Pts',(-0.37312414906919,0.156548476219177,
0.96));
#65088=CARTESIAN_POINT('Ctrl Pts',(-0.37312414906919,0.125170594453812,
1.));
#65089=CARTESIAN_POINT('Ctrl Pts',(-0.37312414906919,0.125170594453812,
0.96));
#65090=CARTESIAN_POINT('Ctrl Pts',(-0.349931773170829,0.179058706760406,
1.));
#65091=CARTESIAN_POINT('Ctrl Pts',(-0.37312414906919,0.156548476219177,
1.));
#65092=CARTESIAN_POINT('Ctrl Pts',(-0.37312414906919,0.125170594453812,
1.));
#65093=CARTESIAN_POINT('Ctrl Pts',(-0.349931773170829,0.179058706760406,
0.96));
#65094=CARTESIAN_POINT('Ctrl Pts',(-0.37312414906919,0.156548476219177,
0.96));
#65095=CARTESIAN_POINT('Ctrl Pts',(-0.37312414906919,0.125170594453812,
0.96));
#65096=CARTESIAN_POINT('Ctrl Pts',(-0.410641190037131,-0.214699828624725,
1.));
#65097=CARTESIAN_POINT('Ctrl Pts',(-0.410641190037131,-0.214699828624725,
0.96));
#65098=CARTESIAN_POINT('Ctrl Pts',(-0.456002723798156,-0.170873069763184,
1.));
#65099=CARTESIAN_POINT('Ctrl Pts',(-0.456002723798156,-0.170873069763184,
0.96));
#65100=CARTESIAN_POINT('Ctrl Pts',(-0.456002723798156,-0.105388784408569,
1.));
#65101=CARTESIAN_POINT('Ctrl Pts',(-0.456002723798156,-0.105388784408569,
0.96));
#65102=CARTESIAN_POINT('',(-0.410641190037131,-0.214699828624725,1.));
#65103=CARTESIAN_POINT('',(-0.456002723798156,-0.105388784408569,1.));
#65104=CARTESIAN_POINT('Ctrl Pts',(-0.410641190037131,-0.214699828624725,
1.));
#65105=CARTESIAN_POINT('Ctrl Pts',(-0.456002723798156,-0.170873069763184,
1.));
#65106=CARTESIAN_POINT('Ctrl Pts',(-0.456002723798156,-0.105388784408569,
1.));
#65107=CARTESIAN_POINT('',(-0.410641190037131,-0.214699828624725,0.96));
#65108=CARTESIAN_POINT('',(-0.410641190037131,-0.214699828624725,1.));
#65109=CARTESIAN_POINT('',(-0.456002723798156,-0.105388784408569,0.96));
#65110=CARTESIAN_POINT('Ctrl Pts',(-0.410641190037131,-0.214699828624725,
0.96));
#65111=CARTESIAN_POINT('Ctrl Pts',(-0.456002723798156,-0.170873069763184,
0.96));
#65112=CARTESIAN_POINT('Ctrl Pts',(-0.456002723798156,-0.105388784408569,
0.96));
#65113=CARTESIAN_POINT('',(-0.456002723798156,-0.105388784408569,1.));
#65114=CARTESIAN_POINT('Ctrl Pts',(-0.291268732771277,-0.258526587486267,
1.));
#65115=CARTESIAN_POINT('Ctrl Pts',(-0.291268732771277,-0.258526587486267,
0.96));
#65116=CARTESIAN_POINT('Ctrl Pts',(-0.365279641374946,-0.258526587486267,
1.));
#65117=CARTESIAN_POINT('Ctrl Pts',(-0.365279641374946,-0.258526587486267,
0.96));
#65118=CARTESIAN_POINT('Ctrl Pts',(-0.410641190037131,-0.214699828624725,
1.));
#65119=CARTESIAN_POINT('Ctrl Pts',(-0.410641190037131,-0.214699828624725,
0.96));
#65120=CARTESIAN_POINT('',(-0.291268732771277,-0.258526587486267,1.));
#65121=CARTESIAN_POINT('Ctrl Pts',(-0.291268732771277,-0.258526587486267,
1.));
#65122=CARTESIAN_POINT('Ctrl Pts',(-0.365279641374946,-0.258526587486267,
1.));
#65123=CARTESIAN_POINT('Ctrl Pts',(-0.410641190037131,-0.214699828624725,
1.));
#65124=CARTESIAN_POINT('',(-0.291268732771277,-0.258526587486267,0.96));
#65125=CARTESIAN_POINT('',(-0.291268732771277,-0.258526587486267,1.));
#65126=CARTESIAN_POINT('Ctrl Pts',(-0.291268732771277,-0.258526587486267,
0.96));
#65127=CARTESIAN_POINT('Ctrl Pts',(-0.365279641374946,-0.258526587486267,
0.96));
#65128=CARTESIAN_POINT('Ctrl Pts',(-0.410641190037131,-0.214699828624725,
0.96));
#65129=CARTESIAN_POINT('Ctrl Pts',(-0.171896305307746,-0.214870357513428,
1.));
#65130=CARTESIAN_POINT('Ctrl Pts',(-0.171896305307746,-0.214870357513428,
0.96));
#65131=CARTESIAN_POINT('Ctrl Pts',(-0.217257824167609,-0.258526587486267,
1.));
#65132=CARTESIAN_POINT('Ctrl Pts',(-0.217257824167609,-0.258526587486267,
0.96));
#65133=CARTESIAN_POINT('Ctrl Pts',(-0.291268732771277,-0.258526587486267,
1.));
#65134=CARTESIAN_POINT('Ctrl Pts',(-0.291268732771277,-0.258526587486267,
0.96));
#65135=CARTESIAN_POINT('',(-0.171896305307746,-0.214870357513428,1.));
#65136=CARTESIAN_POINT('Ctrl Pts',(-0.171896305307746,-0.214870357513428,
1.));
#65137=CARTESIAN_POINT('Ctrl Pts',(-0.217257824167609,-0.258526587486267,
1.));
#65138=CARTESIAN_POINT('Ctrl Pts',(-0.291268732771277,-0.258526587486267,
1.));
#65139=CARTESIAN_POINT('',(-0.171896305307746,-0.214870357513428,0.96));
#65140=CARTESIAN_POINT('',(-0.171896305307746,-0.214870357513428,1.));
#65141=CARTESIAN_POINT('Ctrl Pts',(-0.171896305307746,-0.214870357513428,
0.96));
#65142=CARTESIAN_POINT('Ctrl Pts',(-0.217257824167609,-0.258526587486267,
0.96));
#65143=CARTESIAN_POINT('Ctrl Pts',(-0.291268732771277,-0.258526587486267,
0.96));
#65144=CARTESIAN_POINT('Ctrl Pts',(-0.126534726843238,-0.107094132900238,
1.));
#65145=CARTESIAN_POINT('Ctrl Pts',(-0.126534726843238,-0.107094132900238,
0.96));
#65146=CARTESIAN_POINT('Ctrl Pts',(-0.126534726843238,-0.171214127540588,
1.));
#65147=CARTESIAN_POINT('Ctrl Pts',(-0.126534726843238,-0.171214127540588,
0.96));
#65148=CARTESIAN_POINT('Ctrl Pts',(-0.171896305307746,-0.214870357513428,
1.));
#65149=CARTESIAN_POINT('Ctrl Pts',(-0.171896305307746,-0.214870357513428,
0.96));
#65150=CARTESIAN_POINT('',(-0.126534726843238,-0.107094132900238,1.));
#65151=CARTESIAN_POINT('Ctrl Pts',(-0.126534726843238,-0.107094132900238,
1.));
#65152=CARTESIAN_POINT('Ctrl Pts',(-0.126534726843238,-0.171214127540588,
1.));
#65153=CARTESIAN_POINT('Ctrl Pts',(-0.171896305307746,-0.214870357513428,
1.));
#65154=CARTESIAN_POINT('',(-0.126534726843238,-0.107094132900238,0.96));
#65155=CARTESIAN_POINT('',(-0.126534726843238,-0.107094132900238,1.));
#65156=CARTESIAN_POINT('Ctrl Pts',(-0.126534726843238,-0.107094132900238,
0.96));
#65157=CARTESIAN_POINT('Ctrl Pts',(-0.126534726843238,-0.171214127540588,
0.96));
#65158=CARTESIAN_POINT('Ctrl Pts',(-0.171896305307746,-0.214870357513428,
0.96));
#65159=CARTESIAN_POINT('Ctrl Pts',(-0.150579776987433,-0.0272850632667542,
1.));
#65160=CARTESIAN_POINT('Ctrl Pts',(-0.150579776987433,-0.0272850632667542,
0.96));
#65161=CARTESIAN_POINT('Ctrl Pts',(-0.126534726843238,-0.0607093811035156,
1.));
#65162=CARTESIAN_POINT('Ctrl Pts',(-0.126534726843238,-0.0607093811035156,
0.96));
#65163=CARTESIAN_POINT('Ctrl Pts',(-0.126534726843238,-0.107094132900238,
1.));
#65164=CARTESIAN_POINT('Ctrl Pts',(-0.126534726843238,-0.107094132900238,
0.96));
#65165=CARTESIAN_POINT('',(-0.150579776987433,-0.0272850632667542,1.));
#65166=CARTESIAN_POINT('Ctrl Pts',(-0.150579776987433,-0.0272850632667542,
1.));
#65167=CARTESIAN_POINT('Ctrl Pts',(-0.126534726843238,-0.0607093811035156,
1.));
#65168=CARTESIAN_POINT('Ctrl Pts',(-0.126534726843238,-0.107094132900238,
1.));
#65169=CARTESIAN_POINT('',(-0.150579776987433,-0.0272850632667542,0.96));
#65170=CARTESIAN_POINT('',(-0.150579776987433,-0.0272850632667542,1.));
#65171=CARTESIAN_POINT('Ctrl Pts',(-0.150579776987433,-0.0272850632667542,
0.96));
#65172=CARTESIAN_POINT('Ctrl Pts',(-0.126534726843238,-0.0607093811035156,
0.96));
#65173=CARTESIAN_POINT('Ctrl Pts',(-0.126534726843238,-0.107094132900238,
0.96));
#65174=CARTESIAN_POINT('Ctrl Pts',(-0.220668461546302,0.021146035194397,
1.));
#65175=CARTESIAN_POINT('Ctrl Pts',(-0.220668461546302,0.021146035194397,
0.96));
#65176=CARTESIAN_POINT('Ctrl Pts',(-0.174624797329307,0.00613919496536253,
1.));
#65177=CARTESIAN_POINT('Ctrl Pts',(-0.174624797329307,0.00613919496536253,
0.96));
#65178=CARTESIAN_POINT('Ctrl Pts',(-0.150579776987433,-0.0272850632667542,
1.));
#65179=CARTESIAN_POINT('Ctrl Pts',(-0.150579776987433,-0.0272850632667542,
0.96));
#65180=CARTESIAN_POINT('',(-0.220668461546302,0.021146035194397,1.));
#65181=CARTESIAN_POINT('Ctrl Pts',(-0.220668461546302,0.021146035194397,
1.));
#65182=CARTESIAN_POINT('Ctrl Pts',(-0.174624797329307,0.00613919496536253,
1.));
#65183=CARTESIAN_POINT('Ctrl Pts',(-0.150579776987433,-0.0272850632667542,
1.));
#65184=CARTESIAN_POINT('',(-0.220668461546302,0.021146035194397,0.96));
#65185=CARTESIAN_POINT('',(-0.220668461546302,0.021146035194397,1.));
#65186=CARTESIAN_POINT('Ctrl Pts',(-0.220668461546302,0.021146035194397,
0.96));
#65187=CARTESIAN_POINT('Ctrl Pts',(-0.174624797329307,0.00613919496536253,
0.96));
#65188=CARTESIAN_POINT('Ctrl Pts',(-0.150579776987433,-0.0272850632667542,
0.96));
#65189=CARTESIAN_POINT('Ctrl Pts',(-0.165245559439063,0.0608799815177917,
1.));
#65190=CARTESIAN_POINT('Ctrl Pts',(-0.165245559439063,0.0608799815177917,
0.96));
#65191=CARTESIAN_POINT('Ctrl Pts',(-0.183492478355765,0.0351296424865722,
1.));
#65192=CARTESIAN_POINT('Ctrl Pts',(-0.183492478355765,0.0351296424865722,
0.96));
#65193=CARTESIAN_POINT('Ctrl Pts',(-0.220668461546302,0.021146035194397,
1.));
#65194=CARTESIAN_POINT('Ctrl Pts',(-0.220668461546302,0.021146035194397,
0.96));
#65195=CARTESIAN_POINT('',(-0.165245559439063,0.0608799815177917,1.));
#65196=CARTESIAN_POINT('Ctrl Pts',(-0.165245559439063,0.0608799815177917,
1.));
#65197=CARTESIAN_POINT('Ctrl Pts',(-0.183492478355765,0.0351296424865722,
1.));
#65198=CARTESIAN_POINT('Ctrl Pts',(-0.220668461546302,0.021146035194397,
1.));
#65199=CARTESIAN_POINT('',(-0.165245559439063,0.0608799815177917,0.96));
#65200=CARTESIAN_POINT('',(-0.165245559439063,0.0608799815177917,1.));
#65201=CARTESIAN_POINT('Ctrl Pts',(-0.165245559439063,0.0608799815177917,
0.96));
#65202=CARTESIAN_POINT('Ctrl Pts',(-0.183492478355765,0.0351296424865722,
0.96));
#65203=CARTESIAN_POINT('Ctrl Pts',(-0.220668461546302,0.021146035194397,
0.96));
#65204=CARTESIAN_POINT('Ctrl Pts',(-0.146998610720038,0.121418869495392,
1.));
#65205=CARTESIAN_POINT('Ctrl Pts',(-0.146998610720038,0.121418869495392,
0.96));
#65206=CARTESIAN_POINT('Ctrl Pts',(-0.146998610720038,0.0866303205490112,
1.));
#65207=CARTESIAN_POINT('Ctrl Pts',(-0.146998610720038,0.0866303205490112,
0.96));
#65208=CARTESIAN_POINT('Ctrl Pts',(-0.165245559439063,0.0608799815177917,
1.));
#65209=CARTESIAN_POINT('Ctrl Pts',(-0.165245559439063,0.0608799815177917,
0.96));
#65210=CARTESIAN_POINT('',(-0.146998610720038,0.121418869495392,1.));
#65211=CARTESIAN_POINT('Ctrl Pts',(-0.146998610720038,0.121418869495392,
1.));
#65212=CARTESIAN_POINT('Ctrl Pts',(-0.146998610720038,0.0866303205490112,
1.));
#65213=CARTESIAN_POINT('Ctrl Pts',(-0.165245559439063,0.0608799815177917,
1.));
#65214=CARTESIAN_POINT('',(-0.146998610720038,0.121418869495392,0.96));
#65215=CARTESIAN_POINT('',(-0.146998610720038,0.121418869495392,1.));
#65216=CARTESIAN_POINT('Ctrl Pts',(-0.146998610720038,0.121418869495392,
0.96));
#65217=CARTESIAN_POINT('Ctrl Pts',(-0.146998610720038,0.0866303205490112,
0.96));
#65218=CARTESIAN_POINT('Ctrl Pts',(-0.165245559439063,0.0608799815177917,
0.96));
#65219=CARTESIAN_POINT('Ctrl Pts',(-0.186903115734458,0.214017784595489,
1.));
#65220=CARTESIAN_POINT('Ctrl Pts',(-0.186903115734458,0.214017784595489,
0.96));
#65221=CARTESIAN_POINT('Ctrl Pts',(-0.146998610720038,0.175989127159119,
1.));
#65222=CARTESIAN_POINT('Ctrl Pts',(-0.146998610720038,0.175989127159119,
0.96));
#65223=CARTESIAN_POINT('Ctrl Pts',(-0.146998610720038,0.121418869495392,
1.));
#65224=CARTESIAN_POINT('Ctrl Pts',(-0.146998610720038,0.121418869495392,
0.96));
#65225=CARTESIAN_POINT('',(-0.186903115734458,0.214017784595489,1.));
#65226=CARTESIAN_POINT('Ctrl Pts',(-0.186903115734458,0.214017784595489,
1.));
#65227=CARTESIAN_POINT('Ctrl Pts',(-0.146998610720038,0.175989127159119,
1.));
#65228=CARTESIAN_POINT('Ctrl Pts',(-0.146998610720038,0.121418869495392,
1.));
#65229=CARTESIAN_POINT('',(-0.186903115734458,0.214017784595489,0.96));
#65230=CARTESIAN_POINT('',(-0.186903115734458,0.214017784595489,1.));
#65231=CARTESIAN_POINT('Ctrl Pts',(-0.186903115734458,0.214017784595489,
0.96));
#65232=CARTESIAN_POINT('Ctrl Pts',(-0.146998610720038,0.175989127159119,
0.96));
#65233=CARTESIAN_POINT('Ctrl Pts',(-0.146998610720038,0.121418869495392,
0.96));
#65234=CARTESIAN_POINT('Ctrl Pts',(-0.292291965708137,0.252046382427216,
1.));
#65235=CARTESIAN_POINT('Ctrl Pts',(-0.292291965708137,0.252046382427216,
0.96));
#65236=CARTESIAN_POINT('Ctrl Pts',(-0.226807620748878,0.252046382427216,
1.));
#65237=CARTESIAN_POINT('Ctrl Pts',(-0.226807620748878,0.252046382427216,
0.96));
#65238=CARTESIAN_POINT('Ctrl Pts',(-0.186903115734458,0.214017784595489,
1.));
#65239=CARTESIAN_POINT('Ctrl Pts',(-0.186903115734458,0.214017784595489,
0.96));
#65240=CARTESIAN_POINT('',(-0.292291965708137,0.252046382427216,1.));
#65241=CARTESIAN_POINT('Ctrl Pts',(-0.292291965708137,0.252046382427216,
1.));
#65242=CARTESIAN_POINT('Ctrl Pts',(-0.226807620748878,0.252046382427216,
1.));
#65243=CARTESIAN_POINT('Ctrl Pts',(-0.186903115734458,0.214017784595489,
1.));
#65244=CARTESIAN_POINT('',(-0.292291965708137,0.252046382427216,0.96));
#65245=CARTESIAN_POINT('',(-0.292291965708137,0.252046382427216,1.));
#65246=CARTESIAN_POINT('Ctrl Pts',(-0.292291965708137,0.252046382427216,
0.96));
#65247=CARTESIAN_POINT('Ctrl Pts',(-0.226807620748878,0.252046382427216,
0.96));
#65248=CARTESIAN_POINT('Ctrl Pts',(-0.186903115734458,0.214017784595489,
0.96));
#65249=CARTESIAN_POINT('Ctrl Pts',(-0.396657552942634,0.214870429039001,
1.));
#65250=CARTESIAN_POINT('Ctrl Pts',(-0.396657552942634,0.214870429039001,
0.96));
#65251=CARTESIAN_POINT('Ctrl Pts',(-0.357435193285346,0.252046382427216,
1.));
#65252=CARTESIAN_POINT('Ctrl Pts',(-0.357435193285346,0.252046382427216,
0.96));
#65253=CARTESIAN_POINT('Ctrl Pts',(-0.292291965708137,0.252046382427216,
1.));
#65254=CARTESIAN_POINT('Ctrl Pts',(-0.292291965708137,0.252046382427216,
0.96));
#65255=CARTESIAN_POINT('',(-0.396657552942634,0.214870429039001,1.));
#65256=CARTESIAN_POINT('Ctrl Pts',(-0.396657552942634,0.214870429039001,
1.));
#65257=CARTESIAN_POINT('Ctrl Pts',(-0.357435193285346,0.252046382427216,
1.));
#65258=CARTESIAN_POINT('Ctrl Pts',(-0.292291965708137,0.252046382427216,
1.));
#65259=CARTESIAN_POINT('',(-0.396657552942634,0.214870429039001,0.96));
#65260=CARTESIAN_POINT('',(-0.396657552942634,0.214870429039001,1.));
#65261=CARTESIAN_POINT('Ctrl Pts',(-0.396657552942634,0.214870429039001,
0.96));
#65262=CARTESIAN_POINT('Ctrl Pts',(-0.357435193285346,0.252046382427216,
0.96));
#65263=CARTESIAN_POINT('Ctrl Pts',(-0.292291965708137,0.252046382427216,
0.96));
#65264=CARTESIAN_POINT('Ctrl Pts',(-0.435879942402244,0.123124188184738,
1.));
#65265=CARTESIAN_POINT('Ctrl Pts',(-0.435879942402244,0.123124188184738,
0.96));
#65266=CARTESIAN_POINT('Ctrl Pts',(-0.435879942402244,0.177694445848465,
1.));
#65267=CARTESIAN_POINT('Ctrl Pts',(-0.435879942402244,0.177694445848465,
0.96));
#65268=CARTESIAN_POINT('Ctrl Pts',(-0.396657552942634,0.214870429039001,
1.));
#65269=CARTESIAN_POINT('Ctrl Pts',(-0.396657552942634,0.214870429039001,
0.96));
#65270=CARTESIAN_POINT('',(-0.435879942402244,0.123124188184738,1.));
#65271=CARTESIAN_POINT('Ctrl Pts',(-0.435879942402244,0.123124188184738,
1.));
#65272=CARTESIAN_POINT('Ctrl Pts',(-0.435879942402244,0.177694445848465,
1.));
#65273=CARTESIAN_POINT('Ctrl Pts',(-0.396657552942634,0.214870429039001,
1.));
#65274=CARTESIAN_POINT('',(-0.435879942402244,0.123124188184738,0.96));
#65275=CARTESIAN_POINT('',(-0.435879942402244,0.123124188184738,1.));
#65276=CARTESIAN_POINT('Ctrl Pts',(-0.435879942402244,0.123124188184738,
0.96));
#65277=CARTESIAN_POINT('Ctrl Pts',(-0.435879942402244,0.177694445848465,
0.96));
#65278=CARTESIAN_POINT('Ctrl Pts',(-0.396657552942634,0.214870429039001,
0.96));
#65279=CARTESIAN_POINT('Ctrl Pts',(-0.417462464794517,0.0610505104064941,
1.));
#65280=CARTESIAN_POINT('Ctrl Pts',(-0.417462464794517,0.0610505104064941,
0.96));
#65281=CARTESIAN_POINT('Ctrl Pts',(-0.435879942402244,0.0869714081287384,
1.));
#65282=CARTESIAN_POINT('Ctrl Pts',(-0.435879942402244,0.0869714081287384,
0.96));
#65283=CARTESIAN_POINT('Ctrl Pts',(-0.435879942402244,0.123124188184738,
1.));
#65284=CARTESIAN_POINT('Ctrl Pts',(-0.435879942402244,0.123124188184738,
0.96));
#65285=CARTESIAN_POINT('',(-0.417462464794517,0.0610505104064941,1.));
#65286=CARTESIAN_POINT('Ctrl Pts',(-0.417462464794517,0.0610505104064941,
1.));
#65287=CARTESIAN_POINT('Ctrl Pts',(-0.435879942402244,0.0869714081287384,
1.));
#65288=CARTESIAN_POINT('Ctrl Pts',(-0.435879942402244,0.123124188184738,
1.));
#65289=CARTESIAN_POINT('',(-0.417462464794517,0.0610505104064941,0.96));
#65290=CARTESIAN_POINT('',(-0.417462464794517,0.0610505104064941,1.));
#65291=CARTESIAN_POINT('Ctrl Pts',(-0.417462464794517,0.0610505104064941,
0.96));
#65292=CARTESIAN_POINT('Ctrl Pts',(-0.435879942402244,0.0869714081287384,
0.96));
#65293=CARTESIAN_POINT('Ctrl Pts',(-0.435879942402244,0.123124188184738,
0.96));
#65294=CARTESIAN_POINT('Ctrl Pts',(-0.360845830664039,0.021146035194397,
1.));
#65295=CARTESIAN_POINT('Ctrl Pts',(-0.360845830664039,0.021146035194397,
0.96));
#65296=CARTESIAN_POINT('Ctrl Pts',(-0.399045016989112,0.0351296424865722,
1.));
#65297=CARTESIAN_POINT('Ctrl Pts',(-0.399045016989112,0.0351296424865722,
0.96));
#65298=CARTESIAN_POINT('Ctrl Pts',(-0.417462464794517,0.0610505104064941,
1.));
#65299=CARTESIAN_POINT('Ctrl Pts',(-0.417462464794517,0.0610505104064941,
0.96));
#65300=CARTESIAN_POINT('',(-0.360845830664039,0.021146035194397,1.));
#65301=CARTESIAN_POINT('Ctrl Pts',(-0.360845830664039,0.021146035194397,
1.));
#65302=CARTESIAN_POINT('Ctrl Pts',(-0.399045016989112,0.0351296424865722,
1.));
#65303=CARTESIAN_POINT('Ctrl Pts',(-0.417462464794517,0.0610505104064941,
1.));
#65304=CARTESIAN_POINT('',(-0.360845830664039,0.021146035194397,0.96));
#65305=CARTESIAN_POINT('',(-0.360845830664039,0.021146035194397,1.));
#65306=CARTESIAN_POINT('Ctrl Pts',(-0.360845830664039,0.021146035194397,
0.96));
#65307=CARTESIAN_POINT('Ctrl Pts',(-0.399045016989112,0.0351296424865722,
0.96));
#65308=CARTESIAN_POINT('Ctrl Pts',(-0.417462464794517,0.0610505104064941,
0.96));
#65309=CARTESIAN_POINT('Ctrl Pts',(-0.431275573000312,-0.0237038969993592,
1.));
#65310=CARTESIAN_POINT('Ctrl Pts',(-0.431275573000312,-0.0237038969993592,
0.96));
#65311=CARTESIAN_POINT('Ctrl Pts',(-0.406548422202468,0.00920877456665037,
1.));
#65312=CARTESIAN_POINT('Ctrl Pts',(-0.406548422202468,0.00920877456665037,
0.96));
#65313=CARTESIAN_POINT('Ctrl Pts',(-0.360845830664039,0.021146035194397,
1.));
#65314=CARTESIAN_POINT('Ctrl Pts',(-0.360845830664039,0.021146035194397,
0.96));
#65315=CARTESIAN_POINT('',(-0.431275573000312,-0.0237038969993592,1.));
#65316=CARTESIAN_POINT('Ctrl Pts',(-0.431275573000312,-0.0237038969993592,
1.));
#65317=CARTESIAN_POINT('Ctrl Pts',(-0.406548422202468,0.00920877456665037,
1.));
#65318=CARTESIAN_POINT('Ctrl Pts',(-0.360845830664039,0.021146035194397,
1.));
#65319=CARTESIAN_POINT('',(-0.431275573000312,-0.0237038969993592,0.96));
#65320=CARTESIAN_POINT('',(-0.431275573000312,-0.0237038969993592,1.));
#65321=CARTESIAN_POINT('Ctrl Pts',(-0.431275573000312,-0.0237038969993592,
0.96));
#65322=CARTESIAN_POINT('Ctrl Pts',(-0.406548422202468,0.00920877456665037,
0.96));
#65323=CARTESIAN_POINT('Ctrl Pts',(-0.360845830664039,0.021146035194397,
0.96));
#65324=CARTESIAN_POINT('Ctrl Pts',(-0.456002723798156,-0.105388784408569,
1.));
#65325=CARTESIAN_POINT('Ctrl Pts',(-0.456002723798156,-0.105388784408569,
0.96));
#65326=CARTESIAN_POINT('Ctrl Pts',(-0.456002723798156,-0.0566166281700134,
1.));
#65327=CARTESIAN_POINT('Ctrl Pts',(-0.456002723798156,-0.0566166281700134,
0.96));
#65328=CARTESIAN_POINT('Ctrl Pts',(-0.431275573000312,-0.0237038969993592,
1.));
#65329=CARTESIAN_POINT('Ctrl Pts',(-0.431275573000312,-0.0237038969993592,
0.96));
#65330=CARTESIAN_POINT('Ctrl Pts',(-0.456002723798156,-0.105388784408569,
1.));
#65331=CARTESIAN_POINT('Ctrl Pts',(-0.456002723798156,-0.0566166281700134,
1.));
#65332=CARTESIAN_POINT('Ctrl Pts',(-0.431275573000312,-0.0237038969993592,
1.));
#65333=CARTESIAN_POINT('Ctrl Pts',(-0.456002723798156,-0.105388784408569,
0.96));
#65334=CARTESIAN_POINT('Ctrl Pts',(-0.456002723798156,-0.0566166281700134,
0.96));
#65335=CARTESIAN_POINT('Ctrl Pts',(-0.431275573000312,-0.0237038969993592,
0.96));
#65336=CARTESIAN_POINT('Origin',(-0.291268725320697,-0.00324010252952578,
0.96));
#65337=CARTESIAN_POINT('Origin',(-0.0324011113494634,-0.180081808567047,
1.));
#65338=CARTESIAN_POINT('',(-0.0324011113494634,-0.180081808567047,1.));
#65339=CARTESIAN_POINT('',(0.0375170443207026,-0.180081808567047,1.));
#65340=CARTESIAN_POINT('',(-0.0162005556747317,-0.180081808567047,1.));
#65341=CARTESIAN_POINT('',(-0.0324011113494634,-0.180081808567047,0.96));
#65342=CARTESIAN_POINT('',(-0.0324011113494634,-0.180081808567047,1.));
#65343=CARTESIAN_POINT('',(0.0375170443207026,-0.180081808567047,0.96));
#65344=CARTESIAN_POINT('',(-0.0324011113494634,-0.180081808567047,0.96));
#65345=CARTESIAN_POINT('',(0.0375170443207026,-0.180081808567047,1.));
#65346=CARTESIAN_POINT('Origin',(-0.0324011113494634,-0.249999964237213,
1.));
#65347=CARTESIAN_POINT('',(-0.0324011113494634,-0.249999964237213,1.));
#65348=CARTESIAN_POINT('',(-0.0324011113494634,-0.124999982118607,1.));
#65349=CARTESIAN_POINT('',(-0.0324011113494634,-0.249999964237213,0.96));
#65350=CARTESIAN_POINT('',(-0.0324011113494634,-0.249999964237213,1.));
#65351=CARTESIAN_POINT('',(-0.0324011113494634,-0.249999964237213,0.96));
#65352=CARTESIAN_POINT('Origin',(0.0375170443207026,-0.249999964237213,
1.));
#65353=CARTESIAN_POINT('',(0.0375170443207026,-0.249999964237213,1.));
#65354=CARTESIAN_POINT('',(0.0187585221603513,-0.249999964237213,1.));
#65355=CARTESIAN_POINT('',(0.0375170443207026,-0.249999964237213,0.96));
#65356=CARTESIAN_POINT('',(0.0375170443207026,-0.249999964237213,1.));
#65357=CARTESIAN_POINT('',(0.0375170443207026,-0.249999964237213,0.96));
#65358=CARTESIAN_POINT('Origin',(0.0375170443207026,-0.180081808567047,
1.));
#65359=CARTESIAN_POINT('',(0.0375170443207026,-0.0900409042835236,1.));
#65360=CARTESIAN_POINT('',(0.0375170443207026,-0.180081808567047,0.96));
#65361=CARTESIAN_POINT('Origin',(0.00255796648561957,-0.21504088640213,
0.96));
#65362=CARTESIAN_POINT('Ctrl Pts',(0.289904567971826,-0.00545700788497927,
1.));
#65363=CARTESIAN_POINT('Ctrl Pts',(0.289904567971826,-0.00545700788497927,
0.96));
#65364=CARTESIAN_POINT('Ctrl Pts',(0.246589395776391,-0.00545700788497927,
1.));
#65365=CARTESIAN_POINT('Ctrl Pts',(0.246589395776391,-0.00545700788497927,
0.96));
#65366=CARTESIAN_POINT('Ctrl Pts',(0.218110534921289,-0.0341063976287842,
1.));
#65367=CARTESIAN_POINT('Ctrl Pts',(0.218110534921289,-0.0341063976287842,
0.96));
#65368=CARTESIAN_POINT('',(0.289904567971826,-0.00545700788497927,1.));
#65369=CARTESIAN_POINT('',(0.218110534921289,-0.0341063976287842,1.));
#65370=CARTESIAN_POINT('Ctrl Pts',(0.289904567971826,-0.00545700788497927,
1.));
#65371=CARTESIAN_POINT('Ctrl Pts',(0.246589395776391,-0.00545700788497927,
1.));
#65372=CARTESIAN_POINT('Ctrl Pts',(0.218110534921289,-0.0341063976287842,
1.));
#65373=CARTESIAN_POINT('',(0.289904567971826,-0.00545700788497927,0.96));
#65374=CARTESIAN_POINT('',(0.289904567971826,-0.00545700788497927,1.));
#65375=CARTESIAN_POINT('',(0.218110534921289,-0.0341063976287842,0.96));
#65376=CARTESIAN_POINT('Ctrl Pts',(0.289904567971826,-0.00545700788497927,
0.96));
#65377=CARTESIAN_POINT('Ctrl Pts',(0.246589395776391,-0.00545700788497927,
0.96));
#65378=CARTESIAN_POINT('Ctrl Pts',(0.218110534921289,-0.0341063976287842,
0.96));
#65379=CARTESIAN_POINT('',(0.218110534921289,-0.0341063976287842,1.));
#65380=CARTESIAN_POINT('Ctrl Pts',(0.363744947686791,-0.034447455406189,
1.));
#65381=CARTESIAN_POINT('Ctrl Pts',(0.363744947686791,-0.034447455406189,
0.96));
#65382=CARTESIAN_POINT('Ctrl Pts',(0.334242913499475,-0.00545700788497927,
1.));
#65383=CARTESIAN_POINT('Ctrl Pts',(0.334242913499475,-0.00545700788497927,
0.96));
#65384=CARTESIAN_POINT('Ctrl Pts',(0.289904567971826,-0.00545700788497927,
1.));
#65385=CARTESIAN_POINT('Ctrl Pts',(0.289904567971826,-0.00545700788497927,
0.96));
#65386=CARTESIAN_POINT('',(0.363744947686791,-0.034447455406189,1.));
#65387=CARTESIAN_POINT('Ctrl Pts',(0.363744947686791,-0.034447455406189,
1.));
#65388=CARTESIAN_POINT('Ctrl Pts',(0.334242913499475,-0.00545700788497927,
1.));
#65389=CARTESIAN_POINT('Ctrl Pts',(0.289904567971826,-0.00545700788497927,
1.));
#65390=CARTESIAN_POINT('',(0.363744947686791,-0.034447455406189,0.96));
#65391=CARTESIAN_POINT('',(0.363744947686791,-0.034447455406189,1.));
#65392=CARTESIAN_POINT('Ctrl Pts',(0.363744947686791,-0.034447455406189,
0.96));
#65393=CARTESIAN_POINT('Ctrl Pts',(0.334242913499475,-0.00545700788497927,
0.96));
#65394=CARTESIAN_POINT('Ctrl Pts',(0.289904567971826,-0.00545700788497927,
0.96));
#65395=CARTESIAN_POINT('Ctrl Pts',(0.393246981874108,-0.107776248455048,
1.));
#65396=CARTESIAN_POINT('Ctrl Pts',(0.393246981874108,-0.107776248455048,
0.96));
#65397=CARTESIAN_POINT('Ctrl Pts',(0.393246981874108,-0.0634379029273987,
1.));
#65398=CARTESIAN_POINT('Ctrl Pts',(0.393246981874108,-0.0634379029273987,
0.96));
#65399=CARTESIAN_POINT('Ctrl Pts',(0.363744947686791,-0.034447455406189,
1.));
#65400=CARTESIAN_POINT('Ctrl Pts',(0.363744947686791,-0.034447455406189,
0.96));
#65401=CARTESIAN_POINT('',(0.393246981874108,-0.107776248455048,1.));
#65402=CARTESIAN_POINT('Ctrl Pts',(0.393246981874108,-0.107776248455048,
1.));
#65403=CARTESIAN_POINT('Ctrl Pts',(0.393246981874108,-0.0634379029273987,
1.));
#65404=CARTESIAN_POINT('Ctrl Pts',(0.363744947686791,-0.034447455406189,
1.));
#65405=CARTESIAN_POINT('',(0.393246981874108,-0.107776248455048,0.96));
#65406=CARTESIAN_POINT('',(0.393246981874108,-0.107776248455048,1.));
#65407=CARTESIAN_POINT('Ctrl Pts',(0.393246981874108,-0.107776248455048,
0.96));
#65408=CARTESIAN_POINT('Ctrl Pts',(0.393246981874108,-0.0634379029273987,
0.96));
#65409=CARTESIAN_POINT('Ctrl Pts',(0.363744947686791,-0.034447455406189,
0.96));
#65410=CARTESIAN_POINT('Ctrl Pts',(0.364597532525659,-0.179740750789642,
1.));
#65411=CARTESIAN_POINT('Ctrl Pts',(0.364597532525659,-0.179740750789642,
0.96));
#65412=CARTESIAN_POINT('Ctrl Pts',(0.393246981874108,-0.151432418823242,
1.));
#65413=CARTESIAN_POINT('Ctrl Pts',(0.393246981874108,-0.151432418823242,
0.96));
#65414=CARTESIAN_POINT('Ctrl Pts',(0.393246981874108,-0.107776248455048,
1.));
#65415=CARTESIAN_POINT('Ctrl Pts',(0.393246981874108,-0.107776248455048,
0.96));
#65416=CARTESIAN_POINT('',(0.364597532525659,-0.179740750789642,1.));
#65417=CARTESIAN_POINT('Ctrl Pts',(0.364597532525659,-0.179740750789642,
1.));
#65418=CARTESIAN_POINT('Ctrl Pts',(0.393246981874108,-0.151432418823242,
1.));
#65419=CARTESIAN_POINT('Ctrl Pts',(0.393246981874108,-0.107776248455048,
1.));
#65420=CARTESIAN_POINT('',(0.364597532525659,-0.179740750789642,0.96));
#65421=CARTESIAN_POINT('',(0.364597532525659,-0.179740750789642,1.));
#65422=CARTESIAN_POINT('Ctrl Pts',(0.364597532525659,-0.179740750789642,
0.96));
#65423=CARTESIAN_POINT('Ctrl Pts',(0.393246981874108,-0.151432418823242,
0.96));
#65424=CARTESIAN_POINT('Ctrl Pts',(0.393246981874108,-0.107776248455048,
0.96));
#65425=CARTESIAN_POINT('Ctrl Pts',(0.291950914636254,-0.208049082756043,
1.));
#65426=CARTESIAN_POINT('Ctrl Pts',(0.291950914636254,-0.208049082756043,
0.96));
#65427=CARTESIAN_POINT('Ctrl Pts',(0.335948202386498,-0.208049082756043,
1.));
#65428=CARTESIAN_POINT('Ctrl Pts',(0.335948202386498,-0.208049082756043,
0.96));
#65429=CARTESIAN_POINT('Ctrl Pts',(0.364597532525659,-0.179740750789642,
1.));
#65430=CARTESIAN_POINT('Ctrl Pts',(0.364597532525659,-0.179740750789642,
0.96));
#65431=CARTESIAN_POINT('',(0.291950914636254,-0.208049082756043,1.));
#65432=CARTESIAN_POINT('Ctrl Pts',(0.291950914636254,-0.208049082756043,
1.));
#65433=CARTESIAN_POINT('Ctrl Pts',(0.335948202386498,-0.208049082756043,
1.));
#65434=CARTESIAN_POINT('Ctrl Pts',(0.364597532525659,-0.179740750789642,
1.));
#65435=CARTESIAN_POINT('',(0.291950914636254,-0.208049082756043,0.96));
#65436=CARTESIAN_POINT('',(0.291950914636254,-0.208049082756043,1.));
#65437=CARTESIAN_POINT('Ctrl Pts',(0.291950914636254,-0.208049082756043,
0.96));
#65438=CARTESIAN_POINT('Ctrl Pts',(0.335948202386498,-0.208049082756043,
0.96));
#65439=CARTESIAN_POINT('Ctrl Pts',(0.364597532525659,-0.179740750789642,
0.96));
#65440=CARTESIAN_POINT('Ctrl Pts',(0.239086005464196,-0.194577062129974,
1.));
#65441=CARTESIAN_POINT('Ctrl Pts',(0.239086005464196,-0.194577062129974,
0.96));
#65442=CARTESIAN_POINT('Ctrl Pts',(0.263642642274499,-0.208049082756043,
1.));
#65443=CARTESIAN_POINT('Ctrl Pts',(0.263642642274499,-0.208049082756043,
0.96));
#65444=CARTESIAN_POINT('Ctrl Pts',(0.291950914636254,-0.208049082756043,
1.));
#65445=CARTESIAN_POINT('Ctrl Pts',(0.291950914636254,-0.208049082756043,
0.96));
#65446=CARTESIAN_POINT('',(0.239086005464196,-0.194577062129974,1.));
#65447=CARTESIAN_POINT('Ctrl Pts',(0.239086005464196,-0.194577062129974,
1.));
#65448=CARTESIAN_POINT('Ctrl Pts',(0.263642642274499,-0.208049082756043,
1.));
#65449=CARTESIAN_POINT('Ctrl Pts',(0.291950914636254,-0.208049082756043,
1.));
#65450=CARTESIAN_POINT('',(0.239086005464196,-0.194577062129974,0.96));
#65451=CARTESIAN_POINT('',(0.239086005464196,-0.194577062129974,1.));
#65452=CARTESIAN_POINT('Ctrl Pts',(0.239086005464196,-0.194577062129974,
0.96));
#65453=CARTESIAN_POINT('Ctrl Pts',(0.263642642274499,-0.208049082756043,
0.96));
#65454=CARTESIAN_POINT('Ctrl Pts',(0.291950914636254,-0.208049082756043,
0.96));
#65455=CARTESIAN_POINT('Ctrl Pts',(0.202080580964685,-0.156548404693604,
1.));
#65456=CARTESIAN_POINT('Ctrl Pts',(0.202080580964685,-0.156548404693604,
0.96));
#65457=CARTESIAN_POINT('Ctrl Pts',(0.214529368653893,-0.181104981899261,
1.));
#65458=CARTESIAN_POINT('Ctrl Pts',(0.214529368653893,-0.181104981899261,
0.96));
#65459=CARTESIAN_POINT('Ctrl Pts',(0.239086005464196,-0.194577062129974,
1.));
#65460=CARTESIAN_POINT('Ctrl Pts',(0.239086005464196,-0.194577062129974,
0.96));
#65461=CARTESIAN_POINT('',(0.202080580964685,-0.156548404693604,1.));
#65462=CARTESIAN_POINT('Ctrl Pts',(0.202080580964685,-0.156548404693604,
1.));
#65463=CARTESIAN_POINT('Ctrl Pts',(0.214529368653893,-0.181104981899261,
1.));
#65464=CARTESIAN_POINT('Ctrl Pts',(0.239086005464196,-0.194577062129974,
1.));
#65465=CARTESIAN_POINT('',(0.202080580964685,-0.156548404693604,0.96));
#65466=CARTESIAN_POINT('',(0.202080580964685,-0.156548404693604,1.));
#65467=CARTESIAN_POINT('Ctrl Pts',(0.202080580964685,-0.156548404693604,
0.96));
#65468=CARTESIAN_POINT('Ctrl Pts',(0.214529368653893,-0.181104981899261,
0.96));
#65469=CARTESIAN_POINT('Ctrl Pts',(0.239086005464196,-0.194577062129974,
0.96));
#65470=CARTESIAN_POINT('Ctrl Pts',(0.189631674066186,-0.105729842185974,
1.));
#65471=CARTESIAN_POINT('Ctrl Pts',(0.189631674066186,-0.105729842185974,
0.96));
#65472=CARTESIAN_POINT('Ctrl Pts',(0.189631674066186,-0.131991767883301,
1.));
#65473=CARTESIAN_POINT('Ctrl Pts',(0.189631674066186,-0.131991767883301,
0.96));
#65474=CARTESIAN_POINT('Ctrl Pts',(0.202080580964685,-0.156548404693604,
1.));
#65475=CARTESIAN_POINT('Ctrl Pts',(0.202080580964685,-0.156548404693604,
0.96));
#65476=CARTESIAN_POINT('',(0.189631674066186,-0.105729842185974,1.));
#65477=CARTESIAN_POINT('Ctrl Pts',(0.189631674066186,-0.105729842185974,
1.));
#65478=CARTESIAN_POINT('Ctrl Pts',(0.189631674066186,-0.131991767883301,
1.));
#65479=CARTESIAN_POINT('Ctrl Pts',(0.202080580964685,-0.156548404693604,
1.));
#65480=CARTESIAN_POINT('',(0.189631674066186,-0.105729842185974,0.96));
#65481=CARTESIAN_POINT('',(0.189631674066186,-0.105729842185974,1.));
#65482=CARTESIAN_POINT('Ctrl Pts',(0.189631674066186,-0.105729842185974,
0.96));
#65483=CARTESIAN_POINT('Ctrl Pts',(0.189631674066186,-0.131991767883301,
0.96));
#65484=CARTESIAN_POINT('Ctrl Pts',(0.202080580964685,-0.156548404693604,
0.96));
#65485=CARTESIAN_POINT('Ctrl Pts',(0.218110534921289,-0.0341063976287842,
1.));
#65486=CARTESIAN_POINT('Ctrl Pts',(0.218110534921289,-0.0341063976287842,
0.96));
#65487=CARTESIAN_POINT('Ctrl Pts',(0.189631674066186,-0.0627557873725891,
1.));
#65488=CARTESIAN_POINT('Ctrl Pts',(0.189631674066186,-0.0627557873725891,
0.96));
#65489=CARTESIAN_POINT('Ctrl Pts',(0.189631674066186,-0.105729842185974,
1.));
#65490=CARTESIAN_POINT('Ctrl Pts',(0.189631674066186,-0.105729842185974,
0.96));
#65491=CARTESIAN_POINT('Ctrl Pts',(0.218110534921289,-0.0341063976287842,
1.));
#65492=CARTESIAN_POINT('Ctrl Pts',(0.189631674066186,-0.0627557873725891,
1.));
#65493=CARTESIAN_POINT('Ctrl Pts',(0.189631674066186,-0.105729842185974,
1.));
#65494=CARTESIAN_POINT('Ctrl Pts',(0.218110534921289,-0.0341063976287842,
0.96));
#65495=CARTESIAN_POINT('Ctrl Pts',(0.189631674066186,-0.0627557873725891,
0.96));
#65496=CARTESIAN_POINT('Ctrl Pts',(0.189631674066186,-0.105729842185974,
0.96));
#65497=CARTESIAN_POINT('Ctrl Pts',(0.29092774130404,0.201568937301636,1.));
#65498=CARTESIAN_POINT('Ctrl Pts',(0.29092774130404,0.201568937301636,0.96));
#65499=CARTESIAN_POINT('Ctrl Pts',(0.25579807497561,0.201568937301636,1.));
#65500=CARTESIAN_POINT('Ctrl Pts',(0.25579807497561,0.201568937301636,0.96));
#65501=CARTESIAN_POINT('Ctrl Pts',(0.232605788484216,0.179058706760406,
1.));
#65502=CARTESIAN_POINT('Ctrl Pts',(0.232605788484216,0.179058706760406,
0.96));
#65503=CARTESIAN_POINT('',(0.29092774130404,0.201568937301636,1.));
#65504=CARTESIAN_POINT('',(0.232605788484216,0.179058706760406,1.));
#65505=CARTESIAN_POINT('Ctrl Pts',(0.29092774130404,0.201568937301636,1.));
#65506=CARTESIAN_POINT('Ctrl Pts',(0.25579807497561,0.201568937301636,1.));
#65507=CARTESIAN_POINT('Ctrl Pts',(0.232605788484216,0.179058706760406,
1.));
#65508=CARTESIAN_POINT('',(0.29092774130404,0.201568937301636,0.96));
#65509=CARTESIAN_POINT('',(0.29092774130404,0.201568937301636,1.));
#65510=CARTESIAN_POINT('',(0.232605788484216,0.179058706760406,0.96));
#65511=CARTESIAN_POINT('Ctrl Pts',(0.29092774130404,0.201568937301636,0.96));
#65512=CARTESIAN_POINT('Ctrl Pts',(0.25579807497561,0.201568937301636,0.96));
#65513=CARTESIAN_POINT('Ctrl Pts',(0.232605788484216,0.179058706760406,
0.96));
#65514=CARTESIAN_POINT('',(0.232605788484216,0.179058706760406,1.));
#65515=CARTESIAN_POINT('Ctrl Pts',(0.349079224839807,0.178547120094299,
1.));
#65516=CARTESIAN_POINT('Ctrl Pts',(0.349079224839807,0.178547120094299,
0.96));
#65517=CARTESIAN_POINT('Ctrl Pts',(0.325716230645776,0.201568937301636,
1.));
#65518=CARTESIAN_POINT('Ctrl Pts',(0.325716230645776,0.201568937301636,
0.96));
#65519=CARTESIAN_POINT('Ctrl Pts',(0.29092774130404,0.201568937301636,1.));
#65520=CARTESIAN_POINT('Ctrl Pts',(0.29092774130404,0.201568937301636,0.96));
#65521=CARTESIAN_POINT('',(0.349079224839807,0.178547120094299,1.));
#65522=CARTESIAN_POINT('Ctrl Pts',(0.349079224839807,0.178547120094299,
1.));
#65523=CARTESIAN_POINT('Ctrl Pts',(0.325716230645776,0.201568937301636,
1.));
#65524=CARTESIAN_POINT('Ctrl Pts',(0.29092774130404,0.201568937301636,1.));
#65525=CARTESIAN_POINT('',(0.349079224839807,0.178547120094299,0.96));
#65526=CARTESIAN_POINT('',(0.349079224839807,0.178547120094299,1.));
#65527=CARTESIAN_POINT('Ctrl Pts',(0.349079224839807,0.178547120094299,
0.96));
#65528=CARTESIAN_POINT('Ctrl Pts',(0.325716230645776,0.201568937301636,
0.96));
#65529=CARTESIAN_POINT('Ctrl Pts',(0.29092774130404,0.201568937301636,0.96));
#65530=CARTESIAN_POINT('Ctrl Pts',(0.372442099824548,0.121759927272797,
1.));
#65531=CARTESIAN_POINT('Ctrl Pts',(0.372442099824548,0.121759927272797,
0.96));
#65532=CARTESIAN_POINT('Ctrl Pts',(0.372442099824548,0.15552527308464,1.));
#65533=CARTESIAN_POINT('Ctrl Pts',(0.372442099824548,0.15552527308464,0.96));
#65534=CARTESIAN_POINT('Ctrl Pts',(0.349079224839807,0.178547120094299,
1.));
#65535=CARTESIAN_POINT('Ctrl Pts',(0.349079224839807,0.178547120094299,
0.96));
#65536=CARTESIAN_POINT('',(0.372442099824548,0.121759927272797,1.));
#65537=CARTESIAN_POINT('Ctrl Pts',(0.372442099824548,0.121759927272797,
1.));
#65538=CARTESIAN_POINT('Ctrl Pts',(0.372442099824548,0.15552527308464,1.));
#65539=CARTESIAN_POINT('Ctrl Pts',(0.349079224839807,0.178547120094299,
1.));
#65540=CARTESIAN_POINT('',(0.372442099824548,0.121759927272797,0.96));
#65541=CARTESIAN_POINT('',(0.372442099824548,0.121759927272797,1.));
#65542=CARTESIAN_POINT('Ctrl Pts',(0.372442099824548,0.121759927272797,
0.96));
#65543=CARTESIAN_POINT('Ctrl Pts',(0.372442099824548,0.15552527308464,0.96));
#65544=CARTESIAN_POINT('Ctrl Pts',(0.349079224839807,0.178547120094299,
0.96));
#65545=CARTESIAN_POINT('Ctrl Pts',(0.349761340394616,0.0670191407203674,
1.));
#65546=CARTESIAN_POINT('Ctrl Pts',(0.349761340394616,0.0670191407203674,
0.96));
#65547=CARTESIAN_POINT('Ctrl Pts',(0.372442099824548,0.0893588423728943,
1.));
#65548=CARTESIAN_POINT('Ctrl Pts',(0.372442099824548,0.0893588423728943,
0.96));
#65549=CARTESIAN_POINT('Ctrl Pts',(0.372442099824548,0.121759927272797,
1.));
#65550=CARTESIAN_POINT('Ctrl Pts',(0.372442099824548,0.121759927272797,
0.96));
#65551=CARTESIAN_POINT('',(0.349761340394616,0.0670191407203674,1.));
#65552=CARTESIAN_POINT('Ctrl Pts',(0.349761340394616,0.0670191407203674,
1.));
#65553=CARTESIAN_POINT('Ctrl Pts',(0.372442099824548,0.0893588423728943,
1.));
#65554=CARTESIAN_POINT('Ctrl Pts',(0.372442099824548,0.121759927272797,
1.));
#65555=CARTESIAN_POINT('',(0.349761340394616,0.0670191407203674,0.96));
#65556=CARTESIAN_POINT('',(0.349761340394616,0.0670191407203674,1.));
#65557=CARTESIAN_POINT('Ctrl Pts',(0.349761340394616,0.0670191407203674,
0.96));
#65558=CARTESIAN_POINT('Ctrl Pts',(0.372442099824548,0.0893588423728943,
0.96));
#65559=CARTESIAN_POINT('Ctrl Pts',(0.372442099824548,0.121759927272797,
0.96));
#65560=CARTESIAN_POINT('Ctrl Pts',(0.29160985685885,0.0446794390678406,
1.));
#65561=CARTESIAN_POINT('Ctrl Pts',(0.29160985685885,0.0446794390678406,
0.96));
#65562=CARTESIAN_POINT('Ctrl Pts',(0.327080580964685,0.0446794390678406,
1.));
#65563=CARTESIAN_POINT('Ctrl Pts',(0.327080580964685,0.0446794390678406,
0.96));
#65564=CARTESIAN_POINT('Ctrl Pts',(0.349761340394616,0.0670191407203674,
1.));
#65565=CARTESIAN_POINT('Ctrl Pts',(0.349761340394616,0.0670191407203674,
0.96));
#65566=CARTESIAN_POINT('',(0.29160985685885,0.0446794390678406,1.));
#65567=CARTESIAN_POINT('Ctrl Pts',(0.29160985685885,0.0446794390678406,
1.));
#65568=CARTESIAN_POINT('Ctrl Pts',(0.327080580964685,0.0446794390678406,
1.));
#65569=CARTESIAN_POINT('Ctrl Pts',(0.349761340394616,0.0670191407203674,
1.));
#65570=CARTESIAN_POINT('',(0.29160985685885,0.0446794390678406,0.96));
#65571=CARTESIAN_POINT('',(0.29160985685885,0.0446794390678406,1.));
#65572=CARTESIAN_POINT('Ctrl Pts',(0.29160985685885,0.0446794390678406,
0.96));
#65573=CARTESIAN_POINT('Ctrl Pts',(0.327080580964685,0.0446794390678406,
0.96));
#65574=CARTESIAN_POINT('Ctrl Pts',(0.349761340394616,0.0670191407203674,
0.96));
#65575=CARTESIAN_POINT('Ctrl Pts',(0.232264730706811,0.0671896696090698,
1.));
#65576=CARTESIAN_POINT('Ctrl Pts',(0.232264730706811,0.0671896696090698,
0.96));
#65577=CARTESIAN_POINT('Ctrl Pts',(0.2551159594208,0.0446794390678406,1.));
#65578=CARTESIAN_POINT('Ctrl Pts',(0.2551159594208,0.0446794390678406,0.96));
#65579=CARTESIAN_POINT('Ctrl Pts',(0.29160985685885,0.0446794390678406,
1.));
#65580=CARTESIAN_POINT('Ctrl Pts',(0.29160985685885,0.0446794390678406,
0.96));
#65581=CARTESIAN_POINT('',(0.232264730706811,0.0671896696090698,1.));
#65582=CARTESIAN_POINT('Ctrl Pts',(0.232264730706811,0.0671896696090698,
1.));
#65583=CARTESIAN_POINT('Ctrl Pts',(0.2551159594208,0.0446794390678406,1.));
#65584=CARTESIAN_POINT('Ctrl Pts',(0.29160985685885,0.0446794390678406,
1.));
#65585=CARTESIAN_POINT('',(0.232264730706811,0.0671896696090698,0.96));
#65586=CARTESIAN_POINT('',(0.232264730706811,0.0671896696090698,1.));
#65587=CARTESIAN_POINT('Ctrl Pts',(0.232264730706811,0.0671896696090698,
0.96));
#65588=CARTESIAN_POINT('Ctrl Pts',(0.2551159594208,0.0446794390678406,0.96));
#65589=CARTESIAN_POINT('Ctrl Pts',(0.29160985685885,0.0446794390678406,
0.96));
#65590=CARTESIAN_POINT('Ctrl Pts',(0.209413382783532,0.125170594453812,
1.));
#65591=CARTESIAN_POINT('Ctrl Pts',(0.209413382783532,0.125170594453812,
0.96));
#65592=CARTESIAN_POINT('Ctrl Pts',(0.209413382783532,0.0896999001502991,
1.));
#65593=CARTESIAN_POINT('Ctrl Pts',(0.209413382783532,0.0896999001502991,
0.96));
#65594=CARTESIAN_POINT('Ctrl Pts',(0.232264730706811,0.0671896696090698,
1.));
#65595=CARTESIAN_POINT('Ctrl Pts',(0.232264730706811,0.0671896696090698,
0.96));
#65596=CARTESIAN_POINT('',(0.209413382783532,0.125170594453812,1.));
#65597=CARTESIAN_POINT('Ctrl Pts',(0.209413382783532,0.125170594453812,
1.));
#65598=CARTESIAN_POINT('Ctrl Pts',(0.209413382783532,0.0896999001502991,
1.));
#65599=CARTESIAN_POINT('Ctrl Pts',(0.232264730706811,0.0671896696090698,
1.));
#65600=CARTESIAN_POINT('',(0.209413382783532,0.125170594453812,0.96));
#65601=CARTESIAN_POINT('',(0.209413382783532,0.125170594453812,1.));
#65602=CARTESIAN_POINT('Ctrl Pts',(0.209413382783532,0.125170594453812,
0.96));
#65603=CARTESIAN_POINT('Ctrl Pts',(0.209413382783532,0.0896999001502991,
0.96));
#65604=CARTESIAN_POINT('Ctrl Pts',(0.232264730706811,0.0671896696090698,
0.96));
#65605=CARTESIAN_POINT('Ctrl Pts',(0.232605788484216,0.179058706760406,
1.));
#65606=CARTESIAN_POINT('Ctrl Pts',(0.232605788484216,0.179058706760406,
0.96));
#65607=CARTESIAN_POINT('Ctrl Pts',(0.209413382783532,0.156548476219177,
1.));
#65608=CARTESIAN_POINT('Ctrl Pts',(0.209413382783532,0.156548476219177,
0.96));
#65609=CARTESIAN_POINT('Ctrl Pts',(0.209413382783532,0.125170594453812,
1.));
#65610=CARTESIAN_POINT('Ctrl Pts',(0.209413382783532,0.125170594453812,
0.96));
#65611=CARTESIAN_POINT('Ctrl Pts',(0.232605788484216,0.179058706760406,
1.));
#65612=CARTESIAN_POINT('Ctrl Pts',(0.209413382783532,0.156548476219177,
1.));
#65613=CARTESIAN_POINT('Ctrl Pts',(0.209413382783532,0.125170594453812,
1.));
#65614=CARTESIAN_POINT('Ctrl Pts',(0.232605788484216,0.179058706760406,
0.96));
#65615=CARTESIAN_POINT('Ctrl Pts',(0.209413382783532,0.156548476219177,
0.96));
#65616=CARTESIAN_POINT('Ctrl Pts',(0.209413382783532,0.125170594453812,
0.96));
#65617=CARTESIAN_POINT('Ctrl Pts',(0.171896312013268,-0.214699828624725,
1.));
#65618=CARTESIAN_POINT('Ctrl Pts',(0.171896312013268,-0.214699828624725,
0.96));
#65619=CARTESIAN_POINT('Ctrl Pts',(0.126534793153405,-0.170873069763184,
1.));
#65620=CARTESIAN_POINT('Ctrl Pts',(0.126534793153405,-0.170873069763184,
0.96));
#65621=CARTESIAN_POINT('Ctrl Pts',(0.126534793153405,-0.105388784408569,
1.));
#65622=CARTESIAN_POINT('Ctrl Pts',(0.126534793153405,-0.105388784408569,
0.96));
#65623=CARTESIAN_POINT('',(0.171896312013268,-0.214699828624725,1.));
#65624=CARTESIAN_POINT('',(0.126534793153405,-0.105388784408569,1.));
#65625=CARTESIAN_POINT('Ctrl Pts',(0.171896312013268,-0.214699828624725,
1.));
#65626=CARTESIAN_POINT('Ctrl Pts',(0.126534793153405,-0.170873069763184,
1.));
#65627=CARTESIAN_POINT('Ctrl Pts',(0.126534793153405,-0.105388784408569,
1.));
#65628=CARTESIAN_POINT('',(0.171896312013268,-0.214699828624725,0.96));
#65629=CARTESIAN_POINT('',(0.171896312013268,-0.214699828624725,1.));
#65630=CARTESIAN_POINT('',(0.126534793153405,-0.105388784408569,0.96));
#65631=CARTESIAN_POINT('Ctrl Pts',(0.171896312013268,-0.214699828624725,
0.96));
#65632=CARTESIAN_POINT('Ctrl Pts',(0.126534793153405,-0.170873069763184,
0.96));
#65633=CARTESIAN_POINT('Ctrl Pts',(0.126534793153405,-0.105388784408569,
0.96));
#65634=CARTESIAN_POINT('',(0.126534793153405,-0.105388784408569,1.));
#65635=CARTESIAN_POINT('Ctrl Pts',(0.291268799081445,-0.258526587486267,
1.));
#65636=CARTESIAN_POINT('Ctrl Pts',(0.291268799081445,-0.258526587486267,
0.96));
#65637=CARTESIAN_POINT('Ctrl Pts',(0.217257830873132,-0.258526587486267,
1.));
#65638=CARTESIAN_POINT('Ctrl Pts',(0.217257830873132,-0.258526587486267,
0.96));
#65639=CARTESIAN_POINT('Ctrl Pts',(0.171896312013268,-0.214699828624725,
1.));
#65640=CARTESIAN_POINT('Ctrl Pts',(0.171896312013268,-0.214699828624725,
0.96));
#65641=CARTESIAN_POINT('',(0.291268799081445,-0.258526587486267,1.));
#65642=CARTESIAN_POINT('Ctrl Pts',(0.291268799081445,-0.258526587486267,
1.));
#65643=CARTESIAN_POINT('Ctrl Pts',(0.217257830873132,-0.258526587486267,
1.));
#65644=CARTESIAN_POINT('Ctrl Pts',(0.171896312013268,-0.214699828624725,
1.));
#65645=CARTESIAN_POINT('',(0.291268799081445,-0.258526587486267,0.96));
#65646=CARTESIAN_POINT('',(0.291268799081445,-0.258526587486267,1.));
#65647=CARTESIAN_POINT('Ctrl Pts',(0.291268799081445,-0.258526587486267,
0.96));
#65648=CARTESIAN_POINT('Ctrl Pts',(0.217257830873132,-0.258526587486267,
0.96));
#65649=CARTESIAN_POINT('Ctrl Pts',(0.171896312013268,-0.214699828624725,
0.96));
#65650=CARTESIAN_POINT('Ctrl Pts',(0.410641286149621,-0.214870357513428,
1.));
#65651=CARTESIAN_POINT('Ctrl Pts',(0.410641286149621,-0.214870357513428,
0.96));
#65652=CARTESIAN_POINT('Ctrl Pts',(0.365279767289758,-0.258526587486267,
1.));
#65653=CARTESIAN_POINT('Ctrl Pts',(0.365279767289758,-0.258526587486267,
0.96));
#65654=CARTESIAN_POINT('Ctrl Pts',(0.291268799081445,-0.258526587486267,
1.));
#65655=CARTESIAN_POINT('Ctrl Pts',(0.291268799081445,-0.258526587486267,
0.96));
#65656=CARTESIAN_POINT('',(0.410641286149621,-0.214870357513428,1.));
#65657=CARTESIAN_POINT('Ctrl Pts',(0.410641286149621,-0.214870357513428,
1.));
#65658=CARTESIAN_POINT('Ctrl Pts',(0.365279767289758,-0.258526587486267,
1.));
#65659=CARTESIAN_POINT('Ctrl Pts',(0.291268799081445,-0.258526587486267,
1.));
#65660=CARTESIAN_POINT('',(0.410641286149621,-0.214870357513428,0.96));
#65661=CARTESIAN_POINT('',(0.410641286149621,-0.214870357513428,1.));
#65662=CARTESIAN_POINT('Ctrl Pts',(0.410641286149621,-0.214870357513428,
0.96));
#65663=CARTESIAN_POINT('Ctrl Pts',(0.365279767289758,-0.258526587486267,
0.96));
#65664=CARTESIAN_POINT('Ctrl Pts',(0.291268799081445,-0.258526587486267,
0.96));
#65665=CARTESIAN_POINT('Ctrl Pts',(0.456002805009484,-0.107094132900238,
1.));
#65666=CARTESIAN_POINT('Ctrl Pts',(0.456002805009484,-0.107094132900238,
0.96));
#65667=CARTESIAN_POINT('Ctrl Pts',(0.456002805009484,-0.171214127540588,
1.));
#65668=CARTESIAN_POINT('Ctrl Pts',(0.456002805009484,-0.171214127540588,
0.96));
#65669=CARTESIAN_POINT('Ctrl Pts',(0.410641286149621,-0.214870357513428,
1.));
#65670=CARTESIAN_POINT('Ctrl Pts',(0.410641286149621,-0.214870357513428,
0.96));
#65671=CARTESIAN_POINT('',(0.456002805009484,-0.107094132900238,1.));
#65672=CARTESIAN_POINT('Ctrl Pts',(0.456002805009484,-0.107094132900238,
1.));
#65673=CARTESIAN_POINT('Ctrl Pts',(0.456002805009484,-0.171214127540588,
1.));
#65674=CARTESIAN_POINT('Ctrl Pts',(0.410641286149621,-0.214870357513428,
1.));
#65675=CARTESIAN_POINT('',(0.456002805009484,-0.107094132900238,0.96));
#65676=CARTESIAN_POINT('',(0.456002805009484,-0.107094132900238,1.));
#65677=CARTESIAN_POINT('Ctrl Pts',(0.456002805009484,-0.107094132900238,
0.96));
#65678=CARTESIAN_POINT('Ctrl Pts',(0.456002805009484,-0.171214127540588,
0.96));
#65679=CARTESIAN_POINT('Ctrl Pts',(0.410641286149621,-0.214870357513428,
0.96));
#65680=CARTESIAN_POINT('Ctrl Pts',(0.431957814469934,-0.0272850632667542,
1.));
#65681=CARTESIAN_POINT('Ctrl Pts',(0.431957814469934,-0.0272850632667542,
0.96));
#65682=CARTESIAN_POINT('Ctrl Pts',(0.456002805009484,-0.0607093811035156,
1.));
#65683=CARTESIAN_POINT('Ctrl Pts',(0.456002805009484,-0.0607093811035156,
0.96));
#65684=CARTESIAN_POINT('Ctrl Pts',(0.456002805009484,-0.107094132900238,
1.));
#65685=CARTESIAN_POINT('Ctrl Pts',(0.456002805009484,-0.107094132900238,
0.96));
#65686=CARTESIAN_POINT('',(0.431957814469934,-0.0272850632667542,1.));
#65687=CARTESIAN_POINT('Ctrl Pts',(0.431957814469934,-0.0272850632667542,
1.));
#65688=CARTESIAN_POINT('Ctrl Pts',(0.456002805009484,-0.0607093811035156,
1.));
#65689=CARTESIAN_POINT('Ctrl Pts',(0.456002805009484,-0.107094132900238,
1.));
#65690=CARTESIAN_POINT('',(0.431957814469934,-0.0272850632667542,0.96));
#65691=CARTESIAN_POINT('',(0.431957814469934,-0.0272850632667542,1.));
#65692=CARTESIAN_POINT('Ctrl Pts',(0.431957814469934,-0.0272850632667542,
0.96));
#65693=CARTESIAN_POINT('Ctrl Pts',(0.456002805009484,-0.0607093811035156,
0.96));
#65694=CARTESIAN_POINT('Ctrl Pts',(0.456002805009484,-0.107094132900238,
0.96));
#65695=CARTESIAN_POINT('Ctrl Pts',(0.36186907030642,0.021146035194397,1.));
#65696=CARTESIAN_POINT('Ctrl Pts',(0.36186907030642,0.021146035194397,0.96));
#65697=CARTESIAN_POINT('Ctrl Pts',(0.407912704721093,0.00613919496536253,
1.));
#65698=CARTESIAN_POINT('Ctrl Pts',(0.407912704721093,0.00613919496536253,
0.96));
#65699=CARTESIAN_POINT('Ctrl Pts',(0.431957814469934,-0.0272850632667542,
1.));
#65700=CARTESIAN_POINT('Ctrl Pts',(0.431957814469934,-0.0272850632667542,
0.96));
#65701=CARTESIAN_POINT('',(0.36186907030642,0.021146035194397,1.));
#65702=CARTESIAN_POINT('Ctrl Pts',(0.36186907030642,0.021146035194397,1.));
#65703=CARTESIAN_POINT('Ctrl Pts',(0.407912704721093,0.00613919496536253,
1.));
#65704=CARTESIAN_POINT('Ctrl Pts',(0.431957814469934,-0.0272850632667542,
1.));
#65705=CARTESIAN_POINT('',(0.36186907030642,0.021146035194397,0.96));
#65706=CARTESIAN_POINT('',(0.36186907030642,0.021146035194397,1.));
#65707=CARTESIAN_POINT('Ctrl Pts',(0.36186907030642,0.021146035194397,0.96));
#65708=CARTESIAN_POINT('Ctrl Pts',(0.407912704721093,0.00613919496536253,
0.96));
#65709=CARTESIAN_POINT('Ctrl Pts',(0.431957814469934,-0.0272850632667542,
0.96));
#65710=CARTESIAN_POINT('Ctrl Pts',(0.417291972413659,0.0608799815177917,
1.));
#65711=CARTESIAN_POINT('Ctrl Pts',(0.417291972413659,0.0608799815177917,
0.96));
#65712=CARTESIAN_POINT('Ctrl Pts',(0.399045083299279,0.0351296424865722,
1.));
#65713=CARTESIAN_POINT('Ctrl Pts',(0.399045083299279,0.0351296424865722,
0.96));
#65714=CARTESIAN_POINT('Ctrl Pts',(0.36186907030642,0.021146035194397,1.));
#65715=CARTESIAN_POINT('Ctrl Pts',(0.36186907030642,0.021146035194397,0.96));
#65716=CARTESIAN_POINT('',(0.417291972413659,0.0608799815177917,1.));
#65717=CARTESIAN_POINT('Ctrl Pts',(0.417291972413659,0.0608799815177917,
1.));
#65718=CARTESIAN_POINT('Ctrl Pts',(0.399045083299279,0.0351296424865722,
1.));
#65719=CARTESIAN_POINT('Ctrl Pts',(0.36186907030642,0.021146035194397,1.));
#65720=CARTESIAN_POINT('',(0.417291972413659,0.0608799815177917,0.96));
#65721=CARTESIAN_POINT('',(0.417291972413659,0.0608799815177917,1.));
#65722=CARTESIAN_POINT('Ctrl Pts',(0.417291972413659,0.0608799815177917,
0.96));
#65723=CARTESIAN_POINT('Ctrl Pts',(0.399045083299279,0.0351296424865722,
0.96));
#65724=CARTESIAN_POINT('Ctrl Pts',(0.36186907030642,0.021146035194397,0.96));
#65725=CARTESIAN_POINT('Ctrl Pts',(0.435538980737329,0.121418869495392,
1.));
#65726=CARTESIAN_POINT('Ctrl Pts',(0.435538980737329,0.121418869495392,
0.96));
#65727=CARTESIAN_POINT('Ctrl Pts',(0.435538980737329,0.0866303205490112,
1.));
#65728=CARTESIAN_POINT('Ctrl Pts',(0.435538980737329,0.0866303205490112,
0.96));
#65729=CARTESIAN_POINT('Ctrl Pts',(0.417291972413659,0.0608799815177917,
1.));
#65730=CARTESIAN_POINT('Ctrl Pts',(0.417291972413659,0.0608799815177917,
0.96));
#65731=CARTESIAN_POINT('',(0.435538980737329,0.121418869495392,1.));
#65732=CARTESIAN_POINT('Ctrl Pts',(0.435538980737329,0.121418869495392,
1.));
#65733=CARTESIAN_POINT('Ctrl Pts',(0.435538980737329,0.0866303205490112,
1.));
#65734=CARTESIAN_POINT('Ctrl Pts',(0.417291972413659,0.0608799815177917,
1.));
#65735=CARTESIAN_POINT('',(0.435538980737329,0.121418869495392,0.96));
#65736=CARTESIAN_POINT('',(0.435538980737329,0.121418869495392,1.));
#65737=CARTESIAN_POINT('Ctrl Pts',(0.435538980737329,0.121418869495392,
0.96));
#65738=CARTESIAN_POINT('Ctrl Pts',(0.435538980737329,0.0866303205490112,
0.96));
#65739=CARTESIAN_POINT('Ctrl Pts',(0.417291972413659,0.0608799815177917,
0.96));
#65740=CARTESIAN_POINT('Ctrl Pts',(0.395634386315942,0.214017784595489,
1.));
#65741=CARTESIAN_POINT('Ctrl Pts',(0.395634386315942,0.214017784595489,
0.96));
#65742=CARTESIAN_POINT('Ctrl Pts',(0.435538980737329,0.175989127159119,
1.));
#65743=CARTESIAN_POINT('Ctrl Pts',(0.435538980737329,0.175989127159119,
0.96));
#65744=CARTESIAN_POINT('Ctrl Pts',(0.435538980737329,0.121418869495392,
1.));
#65745=CARTESIAN_POINT('Ctrl Pts',(0.435538980737329,0.121418869495392,
0.96));
#65746=CARTESIAN_POINT('',(0.395634386315942,0.214017784595489,1.));
#65747=CARTESIAN_POINT('Ctrl Pts',(0.395634386315942,0.214017784595489,
1.));
#65748=CARTESIAN_POINT('Ctrl Pts',(0.435538980737329,0.175989127159119,
1.));
#65749=CARTESIAN_POINT('Ctrl Pts',(0.435538980737329,0.121418869495392,
1.));
#65750=CARTESIAN_POINT('',(0.395634386315942,0.214017784595489,0.96));
#65751=CARTESIAN_POINT('',(0.395634386315942,0.214017784595489,1.));
#65752=CARTESIAN_POINT('Ctrl Pts',(0.395634386315942,0.214017784595489,
0.96));
#65753=CARTESIAN_POINT('Ctrl Pts',(0.435538980737329,0.175989127159119,
0.96));
#65754=CARTESIAN_POINT('Ctrl Pts',(0.435538980737329,0.121418869495392,
0.96));
#65755=CARTESIAN_POINT('Ctrl Pts',(0.29024562574923,0.252046382427216,1.));
#65756=CARTESIAN_POINT('Ctrl Pts',(0.29024562574923,0.252046382427216,0.96));
#65757=CARTESIAN_POINT('Ctrl Pts',(0.355729911103845,0.252046382427216,
1.));
#65758=CARTESIAN_POINT('Ctrl Pts',(0.355729911103845,0.252046382427216,
0.96));
#65759=CARTESIAN_POINT('Ctrl Pts',(0.395634386315942,0.214017784595489,
1.));
#65760=CARTESIAN_POINT('Ctrl Pts',(0.395634386315942,0.214017784595489,
0.96));
#65761=CARTESIAN_POINT('',(0.29024562574923,0.252046382427216,1.));
#65762=CARTESIAN_POINT('Ctrl Pts',(0.29024562574923,0.252046382427216,1.));
#65763=CARTESIAN_POINT('Ctrl Pts',(0.355729911103845,0.252046382427216,
1.));
#65764=CARTESIAN_POINT('Ctrl Pts',(0.395634386315942,0.214017784595489,
1.));
#65765=CARTESIAN_POINT('',(0.29024562574923,0.252046382427216,0.96));
#65766=CARTESIAN_POINT('',(0.29024562574923,0.252046382427216,1.));
#65767=CARTESIAN_POINT('Ctrl Pts',(0.29024562574923,0.252046382427216,0.96));
#65768=CARTESIAN_POINT('Ctrl Pts',(0.355729911103845,0.252046382427216,
0.96));
#65769=CARTESIAN_POINT('Ctrl Pts',(0.395634386315942,0.214017784595489,
0.96));
#65770=CARTESIAN_POINT('Ctrl Pts',(0.185880038514733,0.214870429039001,
1.));
#65771=CARTESIAN_POINT('Ctrl Pts',(0.185880038514733,0.214870429039001,
0.96));
#65772=CARTESIAN_POINT('Ctrl Pts',(0.225102398172021,0.252046382427216,
1.));
#65773=CARTESIAN_POINT('Ctrl Pts',(0.225102398172021,0.252046382427216,
0.96));
#65774=CARTESIAN_POINT('Ctrl Pts',(0.29024562574923,0.252046382427216,1.));
#65775=CARTESIAN_POINT('Ctrl Pts',(0.29024562574923,0.252046382427216,0.96));
#65776=CARTESIAN_POINT('',(0.185880038514733,0.214870429039001,1.));
#65777=CARTESIAN_POINT('Ctrl Pts',(0.185880038514733,0.214870429039001,
1.));
#65778=CARTESIAN_POINT('Ctrl Pts',(0.225102398172021,0.252046382427216,
1.));
#65779=CARTESIAN_POINT('Ctrl Pts',(0.29024562574923,0.252046382427216,1.));
#65780=CARTESIAN_POINT('',(0.185880038514733,0.214870429039001,0.96));
#65781=CARTESIAN_POINT('',(0.185880038514733,0.214870429039001,1.));
#65782=CARTESIAN_POINT('Ctrl Pts',(0.185880038514733,0.214870429039001,
0.96));
#65783=CARTESIAN_POINT('Ctrl Pts',(0.225102398172021,0.252046382427216,
0.96));
#65784=CARTESIAN_POINT('Ctrl Pts',(0.29024562574923,0.252046382427216,0.96));
#65785=CARTESIAN_POINT('Ctrl Pts',(0.146657559648156,0.123124188184738,
1.));
#65786=CARTESIAN_POINT('Ctrl Pts',(0.146657559648156,0.123124188184738,
0.96));
#65787=CARTESIAN_POINT('Ctrl Pts',(0.146657559648156,0.177694445848465,
1.));
#65788=CARTESIAN_POINT('Ctrl Pts',(0.146657559648156,0.177694445848465,
0.96));
#65789=CARTESIAN_POINT('Ctrl Pts',(0.185880038514733,0.214870429039001,
1.));
#65790=CARTESIAN_POINT('Ctrl Pts',(0.185880038514733,0.214870429039001,
0.96));
#65791=CARTESIAN_POINT('',(0.146657559648156,0.123124188184738,1.));
#65792=CARTESIAN_POINT('Ctrl Pts',(0.146657559648156,0.123124188184738,
1.));
#65793=CARTESIAN_POINT('Ctrl Pts',(0.146657559648156,0.177694445848465,
1.));
#65794=CARTESIAN_POINT('Ctrl Pts',(0.185880038514733,0.214870429039001,
1.));
#65795=CARTESIAN_POINT('',(0.146657559648156,0.123124188184738,0.96));
#65796=CARTESIAN_POINT('',(0.146657559648156,0.123124188184738,1.));
#65797=CARTESIAN_POINT('Ctrl Pts',(0.146657559648156,0.123124188184738,
0.96));
#65798=CARTESIAN_POINT('Ctrl Pts',(0.146657559648156,0.177694445848465,
0.96));
#65799=CARTESIAN_POINT('Ctrl Pts',(0.185880038514733,0.214870429039001,
0.96));
#65800=CARTESIAN_POINT('Ctrl Pts',(0.165075037255883,0.0610505104064941,
1.));
#65801=CARTESIAN_POINT('Ctrl Pts',(0.165075037255883,0.0610505104064941,
0.96));
#65802=CARTESIAN_POINT('Ctrl Pts',(0.146657559648156,0.0869714081287384,
1.));
#65803=CARTESIAN_POINT('Ctrl Pts',(0.146657559648156,0.0869714081287384,
0.96));
#65804=CARTESIAN_POINT('Ctrl Pts',(0.146657559648156,0.123124188184738,
1.));
#65805=CARTESIAN_POINT('Ctrl Pts',(0.146657559648156,0.123124188184738,
0.96));
#65806=CARTESIAN_POINT('',(0.165075037255883,0.0610505104064941,1.));
#65807=CARTESIAN_POINT('Ctrl Pts',(0.165075037255883,0.0610505104064941,
1.));
#65808=CARTESIAN_POINT('Ctrl Pts',(0.146657559648156,0.0869714081287384,
1.));
#65809=CARTESIAN_POINT('Ctrl Pts',(0.146657559648156,0.123124188184738,
1.));
#65810=CARTESIAN_POINT('',(0.165075037255883,0.0610505104064941,0.96));
#65811=CARTESIAN_POINT('',(0.165075037255883,0.0610505104064941,1.));
#65812=CARTESIAN_POINT('Ctrl Pts',(0.165075037255883,0.0610505104064941,
0.96));
#65813=CARTESIAN_POINT('Ctrl Pts',(0.146657559648156,0.0869714081287384,
0.96));
#65814=CARTESIAN_POINT('Ctrl Pts',(0.146657559648156,0.123124188184738,
0.96));
#65815=CARTESIAN_POINT('Ctrl Pts',(0.221691701188684,0.021146035194397,
1.));
#65816=CARTESIAN_POINT('Ctrl Pts',(0.221691701188684,0.021146035194397,
0.96));
#65817=CARTESIAN_POINT('Ctrl Pts',(0.18349251486361,0.0351296424865722,
1.));
#65818=CARTESIAN_POINT('Ctrl Pts',(0.18349251486361,0.0351296424865722,
0.96));
#65819=CARTESIAN_POINT('Ctrl Pts',(0.165075037255883,0.0610505104064941,
1.));
#65820=CARTESIAN_POINT('Ctrl Pts',(0.165075037255883,0.0610505104064941,
0.96));
#65821=CARTESIAN_POINT('',(0.221691701188684,0.021146035194397,1.));
#65822=CARTESIAN_POINT('Ctrl Pts',(0.221691701188684,0.021146035194397,
1.));
#65823=CARTESIAN_POINT('Ctrl Pts',(0.18349251486361,0.0351296424865722,
1.));
#65824=CARTESIAN_POINT('Ctrl Pts',(0.165075037255883,0.0610505104064941,
1.));
#65825=CARTESIAN_POINT('',(0.221691701188684,0.021146035194397,0.96));
#65826=CARTESIAN_POINT('',(0.221691701188684,0.021146035194397,1.));
#65827=CARTESIAN_POINT('Ctrl Pts',(0.221691701188684,0.021146035194397,
0.96));
#65828=CARTESIAN_POINT('Ctrl Pts',(0.18349251486361,0.0351296424865722,
0.96));
#65829=CARTESIAN_POINT('Ctrl Pts',(0.165075037255883,0.0610505104064941,
0.96));
#65830=CARTESIAN_POINT('Ctrl Pts',(0.151262018457055,-0.0237038969993592,
1.));
#65831=CARTESIAN_POINT('Ctrl Pts',(0.151262018457055,-0.0237038969993592,
0.96));
#65832=CARTESIAN_POINT('Ctrl Pts',(0.175989124551415,0.00920877456665037,
1.));
#65833=CARTESIAN_POINT('Ctrl Pts',(0.175989124551415,0.00920877456665037,
0.96));
#65834=CARTESIAN_POINT('Ctrl Pts',(0.221691701188684,0.021146035194397,
1.));
#65835=CARTESIAN_POINT('Ctrl Pts',(0.221691701188684,0.021146035194397,
0.96));
#65836=CARTESIAN_POINT('',(0.151262018457055,-0.0237038969993592,1.));
#65837=CARTESIAN_POINT('Ctrl Pts',(0.151262018457055,-0.0237038969993592,
1.));
#65838=CARTESIAN_POINT('Ctrl Pts',(0.175989124551415,0.00920877456665037,
1.));
#65839=CARTESIAN_POINT('Ctrl Pts',(0.221691701188684,0.021146035194397,
1.));
#65840=CARTESIAN_POINT('',(0.151262018457055,-0.0237038969993592,0.96));
#65841=CARTESIAN_POINT('',(0.151262018457055,-0.0237038969993592,1.));
#65842=CARTESIAN_POINT('Ctrl Pts',(0.151262018457055,-0.0237038969993592,
0.96));
#65843=CARTESIAN_POINT('Ctrl Pts',(0.175989124551415,0.00920877456665037,
0.96));
#65844=CARTESIAN_POINT('Ctrl Pts',(0.221691701188684,0.021146035194397,
0.96));
#65845=CARTESIAN_POINT('Ctrl Pts',(0.126534793153405,-0.105388784408569,
1.));
#65846=CARTESIAN_POINT('Ctrl Pts',(0.126534793153405,-0.105388784408569,
0.96));
#65847=CARTESIAN_POINT('Ctrl Pts',(0.126534793153405,-0.0566166281700134,
1.));
#65848=CARTESIAN_POINT('Ctrl Pts',(0.126534793153405,-0.0566166281700134,
0.96));
#65849=CARTESIAN_POINT('Ctrl Pts',(0.151262018457055,-0.0237038969993592,
1.));
#65850=CARTESIAN_POINT('Ctrl Pts',(0.151262018457055,-0.0237038969993592,
0.96));
#65851=CARTESIAN_POINT('Ctrl Pts',(0.126534793153405,-0.105388784408569,
1.));
#65852=CARTESIAN_POINT('Ctrl Pts',(0.126534793153405,-0.0566166281700134,
1.));
#65853=CARTESIAN_POINT('Ctrl Pts',(0.151262018457055,-0.0237038969993592,
1.));
#65854=CARTESIAN_POINT('Ctrl Pts',(0.126534793153405,-0.105388784408569,
0.96));
#65855=CARTESIAN_POINT('Ctrl Pts',(0.126534793153405,-0.0566166281700134,
0.96));
#65856=CARTESIAN_POINT('Ctrl Pts',(0.151262018457055,-0.0237038969993592,
0.96));
#65857=CARTESIAN_POINT('Origin',(0.291268799081445,-0.00324010252952578,
0.96));
#65858=CARTESIAN_POINT('Origin',(0.,0.,1.));
#65859=CARTESIAN_POINT('Origin',(0.,0.,1.));
#65860=CARTESIAN_POINT('Origin',(0.,0.,1.));
#65861=CARTESIAN_POINT('Origin',(0.,0.,1.));
#65862=CARTESIAN_POINT('Origin',(1.87869726832665E-16,-4.25270154953079E-17,
-0.0599999999999987));
#65863=CARTESIAN_POINT('Ctrl Pts',(0.564519729112616,0.374023388155322,
-0.06));
#65864=CARTESIAN_POINT('Ctrl Pts',(0.556017057337338,0.389715461663178,
-0.0599999999999997));
#65865=CARTESIAN_POINT('Ctrl Pts',(0.546881793340869,0.405030545447623,
-0.0600000000000022));
#65866=CARTESIAN_POINT('Ctrl Pts',(0.537121082038997,0.419926055265349,
-0.0600000000000023));
#65867=CARTESIAN_POINT('Ctrl Pts',(0.521265382290218,0.444122932313598,
-0.0600000000000025));
#65868=CARTESIAN_POINT('Ctrl Pts',(0.503760937756791,0.467213595952793,
-0.0600000000000015));
#65869=CARTESIAN_POINT('Ctrl Pts',(0.484792757621966,0.489116897605382,
-0.060000000000003));
#65870=CARTESIAN_POINT('Ctrl Pts',(0.477747354694951,0.497252500730066,
-0.0600000000000035));
#65871=CARTESIAN_POINT('Ctrl Pts',(0.47049970935453,0.505224152689485,-0.0600000000000051));
#65872=CARTESIAN_POINT('Ctrl Pts',(0.463058313081755,0.513027130461428,
-0.0600000000000055));
#65873=CARTESIAN_POINT('Ctrl Pts',(0.457142398647175,0.519230502401535,
-0.0600000000000059));
#65874=CARTESIAN_POINT('Ctrl Pts',(0.451104521358182,0.525326494138705,
-0.0600000000000083));
#65875=CARTESIAN_POINT('Ctrl Pts',(0.444958706598096,0.531303709121088,
-0.0600000000000078));
#65876=CARTESIAN_POINT('Ctrl Pts',(0.420677607542062,0.554918698301855,
-0.0600000000000056));
#65877=CARTESIAN_POINT('Ctrl Pts',(0.394678481543999,0.576721462967644,
-0.06));
#65878=CARTESIAN_POINT('Ctrl Pts',(0.367241084736883,0.596581858045739,
-0.0599999999999993));
#65879=CARTESIAN_POINT('Ctrl Pts',(0.349962505322962,0.60908885409792,-0.059999999999999));
#65880=CARTESIAN_POINT('Ctrl Pts',(0.332112498690617,0.620825037936489,
-0.0600000000000051));
#65881=CARTESIAN_POINT('Ctrl Pts',(0.313752738001227,0.631750795096854,
-0.0600000000000059));
#65882=CARTESIAN_POINT('Ctrl Pts',(0.307066444369792,0.635729758753072,
-0.0600000000000062));
#65883=CARTESIAN_POINT('Ctrl Pts',(0.300320585088648,0.639596340261989,
-0.0600000000000039));
#65884=CARTESIAN_POINT('Ctrl Pts',(0.293519801750991,0.643348510928835,
-0.0600000000000039));
#65885=CARTESIAN_POINT('Ctrl Pts',(0.289341260343745,0.645653921896958,
-0.0600000000000039));
#65886=CARTESIAN_POINT('Ctrl Pts',(0.285141833540485,0.647916228279921,
-0.0600000000000032));
#65887=CARTESIAN_POINT('Ctrl Pts',(0.280922298401405,0.650135110019904,
-0.0600000000000031));
#65888=CARTESIAN_POINT('Ctrl Pts',(0.25053489436036,0.666114608644694,-0.060000000000002));
#65889=CARTESIAN_POINT('Ctrl Pts',(0.219107606892874,0.679845250773148,
-0.0600000000000015));
#65890=CARTESIAN_POINT('Ctrl Pts',(0.186893278148277,0.691299397430587,
-0.0600000000000007));
#65891=CARTESIAN_POINT('Ctrl Pts',(0.154590738619216,0.702784908369121,
-0.0599999999999998));
#65892=CARTESIAN_POINT('Ctrl Pts',(0.121495760592277,0.711981939343559,
-0.0600000000000043));
#65893=CARTESIAN_POINT('Ctrl Pts',(0.087835924422175,0.718818063572574,
-0.0600000000000051));
#65894=CARTESIAN_POINT('Ctrl Pts',(0.078192029520663,0.720776684620672,
-0.0600000000000053));
#65895=CARTESIAN_POINT('Ctrl Pts',(0.0685016518516216,0.722541197386995,
-0.060000000000002));
#65896=CARTESIAN_POINT('Ctrl Pts',(0.0587699268909895,0.724109135045819,
-0.0600000000000022));
#65897=CARTESIAN_POINT('Ctrl Pts',(0.051744008636474,0.725241123656639,
-0.0600000000000024));
#65898=CARTESIAN_POINT('Ctrl Pts',(0.0446979572491356,0.72627029397537,
-0.0600000000000017));
#65899=CARTESIAN_POINT('Ctrl Pts',(0.0376459184080252,0.72719449158428,
-0.0600000000000016));
#65900=CARTESIAN_POINT('Ctrl Pts',(0.00302545646785632,0.731731640182775,
-0.0600000000000011));
#65901=CARTESIAN_POINT('Ctrl Pts',(-0.031815950771749,0.733755643496836,
-0.0600000000000015));
#65902=CARTESIAN_POINT('Ctrl Pts',(-0.0666351986914192,0.733220747553446,
-0.0600000000000016));
#65903=CARTESIAN_POINT('Ctrl Pts',(-0.0978099748576694,0.73274183826322,
-0.0600000000000017));
#65904=CARTESIAN_POINT('Ctrl Pts',(-0.128967916329204,0.730211415375235,
-0.0600000000000015));
#65905=CARTESIAN_POINT('Ctrl Pts',(-0.159918958605025,0.725709968094987,
-0.0600000000000019));
#65906=CARTESIAN_POINT('Ctrl Pts',(-0.177115326992562,0.72320896845115,
-0.0600000000000022));
#65907=CARTESIAN_POINT('Ctrl Pts',(-0.194247924239629,0.720098917582186,
-0.0600000000000003));
#65908=CARTESIAN_POINT('Ctrl Pts',(-0.211284081588466,0.716389152698896,
-0.0600000000000005));
#65909=CARTESIAN_POINT('Ctrl Pts',(-0.21877637839257,0.714757642786777,
-0.0600000000000005));
#65910=CARTESIAN_POINT('Ctrl Pts',(-0.226252210451876,0.713009546015677,
-0.0600000000000036));
#65911=CARTESIAN_POINT('Ctrl Pts',(-0.233701701874929,0.711147247282136,
-0.0600000000000037));
#65912=CARTESIAN_POINT('Ctrl Pts',(-0.268556898996262,0.702433794809997,
-0.0600000000000039));
#65913=CARTESIAN_POINT('Ctrl Pts',(-0.302694523266425,0.691261318242376,
-0.0599999999999986));
#65914=CARTESIAN_POINT('Ctrl Pts',(-0.335838445624681,0.677768486476775,
-0.0599999999999999));
#65915=CARTESIAN_POINT('Ctrl Pts',(-0.366475589801689,0.665296159644406,
-0.0600000000000011));
#65916=CARTESIAN_POINT('Ctrl Pts',(-0.396264622338141,0.650840433539252,
-0.0600000000000013));
#65917=CARTESIAN_POINT('Ctrl Pts',(-0.424984508158568,0.634471369253308,
-0.0600000000000007));
#65918=CARTESIAN_POINT('Ctrl Pts',(-0.439836175671524,0.626006575841765,
-0.0600000000000003));
#65919=CARTESIAN_POINT('Ctrl Pts',(-0.454401799726264,0.617029523971439,
-0.0600000000000031));
#65920=CARTESIAN_POINT('Ctrl Pts',(-0.46866343319739,0.607559896176671,
-0.060000000000003));
#65921=CARTESIAN_POINT('Ctrl Pts',(-0.476254270714066,0.602519631603962,
-0.060000000000003));
#65922=CARTESIAN_POINT('Ctrl Pts',(-0.483758966532017,0.597339781307538,
-0.0600000000000032));
#65923=CARTESIAN_POINT('Ctrl Pts',(-0.491174642031591,0.592023050064053,
-0.0600000000000034));
#65924=CARTESIAN_POINT('Ctrl Pts',(-0.497227421634385,0.587683458556044,
-0.0600000000000035));
#65925=CARTESIAN_POINT('Ctrl Pts',(-0.503220520759525,0.583252774240972,
-0.0600000000000041));
#65926=CARTESIAN_POINT('Ctrl Pts',(-0.509141502723096,0.57874116345263,
-0.0600000000000041));
#65927=CARTESIAN_POINT('Ctrl Pts',(-0.538044859697743,0.556717671750003,
-0.060000000000004));
#65928=CARTESIAN_POINT('Ctrl Pts',(-0.565299991169042,0.532721355130354,
-0.0600000000000025));
#65929=CARTESIAN_POINT('Ctrl Pts',(-0.590759649941275,0.506978100941496,
-0.0600000000000023));
#65930=CARTESIAN_POINT('Ctrl Pts',(-0.616419524097047,0.481032401167758,
-0.060000000000002));
#65931=CARTESIAN_POINT('Ctrl Pts',(-0.640256514113435,0.453311469631144,
-0.0600000000000016));
#65932=CARTESIAN_POINT('Ctrl Pts',(-0.662093299222365,0.424001632204223,
-0.0600000000000009));
#65933=CARTESIAN_POINT('Ctrl Pts',(-0.675906732853106,0.405460922479556,
-0.0600000000000005));
#65934=CARTESIAN_POINT('Ctrl Pts',(-0.688919204795322,0.386283542748579,
-0.0600000000000007));
#65935=CARTESIAN_POINT('Ctrl Pts',(-0.701077753000027,0.366509473613485,
-0.0600000000000005));
#65936=CARTESIAN_POINT('',(0.7911,-9.68818082805471E-17,-0.0599999999999996));
#65937=CARTESIAN_POINT('Origin',(0.,0.,-0.0599999999999996));
#65938=CARTESIAN_POINT('',(-0.725153241366725,-0.317623382068616,-0.0600000000000044));
#65939=CARTESIAN_POINT('Origin',(0.,0.,-0.0599999999999996));
#65940=CARTESIAN_POINT('Ctrl Pts',(-0.725153241366672,-0.31762338206874,
-0.059999999999999));
#65941=CARTESIAN_POINT('Ctrl Pts',(-0.71567638822314,-0.336030067509267,
-0.0599999999999988));
#65942=CARTESIAN_POINT('Ctrl Pts',(-0.705459356711865,-0.354019774411552,
-0.0599999999999999));
#65943=CARTESIAN_POINT('Ctrl Pts',(-0.69449898909459,-0.371543591325028,
-0.0599999999999991));
#65944=CARTESIAN_POINT('Ctrl Pts',(-0.677442366510842,-0.398814312687398,
-0.059999999999998));
#65945=CARTESIAN_POINT('Ctrl Pts',(-0.658586409729439,-0.42495799055036,
-0.0599999999999969));
#65946=CARTESIAN_POINT('Ctrl Pts',(-0.638101393125394,-0.449852933456938,
-0.0599999999999976));
#65947=CARTESIAN_POINT('Ctrl Pts',(-0.628212892280591,-0.461870188249615,
-0.059999999999998));
#65948=CARTESIAN_POINT('Ctrl Pts',(-0.617944473508911,-0.473596129144332,
-0.0600000000000003));
#65949=CARTESIAN_POINT('Ctrl Pts',(-0.607313831651076,-0.485014974644845,
-0.0600000000000007));
#65950=CARTESIAN_POINT('Ctrl Pts',(-0.60081457747583,-0.491996112781956,
-0.0600000000000009));
#65951=CARTESIAN_POINT('Ctrl Pts',(-0.594186380454014,-0.498855443847342,
-0.0600000000000002));
#65952=CARTESIAN_POINT('Ctrl Pts',(-0.587436138509517,-0.505587758432277,
-0.0600000000000002));
#65953=CARTESIAN_POINT('Ctrl Pts',(-0.562022501970022,-0.530933901183581,
-0.0600000000000004));
#65954=CARTESIAN_POINT('Ctrl Pts',(-0.534870946059782,-0.554493762857957,
-0.0599999999999985));
#65955=CARTESIAN_POINT('Ctrl Pts',(-0.506214094516617,-0.576089885197481,
-0.0599999999999995));
#65956=CARTESIAN_POINT('Ctrl Pts',(-0.488437010443516,-0.589486893654757,
-0.0600000000000001));
#65957=CARTESIAN_POINT('Ctrl Pts',(-0.470080056783044,-0.602127431065171,
-0.0599999999999962));
#65958=CARTESIAN_POINT('Ctrl Pts',(-0.4511951475437,-0.613960201983324,
-0.0599999999999962));
#65959=CARTESIAN_POINT('Ctrl Pts',(-0.444140303534987,-0.618380575518637,
-0.0599999999999961));
#65960=CARTESIAN_POINT('Ctrl Pts',(-0.437018723894153,-0.622683725880098,
-0.0600000000000009));
#65961=CARTESIAN_POINT('Ctrl Pts',(-0.429837497145262,-0.626865226020263,
-0.0600000000000009));
#65962=CARTESIAN_POINT('Ctrl Pts',(-0.425253905882446,-0.629534169388592,
-0.0600000000000009));
#65963=CARTESIAN_POINT('Ctrl Pts',(-0.420645488243079,-0.632153880439322,
-0.0600000000000031));
#65964=CARTESIAN_POINT('Ctrl Pts',(-0.416013022974233,-0.634723838317226,
-0.060000000000003));
#65965=CARTESIAN_POINT('Ctrl Pts',(-0.384772265521933,-0.652055307862434,
-0.0600000000000021));
#65966=CARTESIAN_POINT('Ctrl Pts',(-0.352439280623423,-0.667128030309419,
-0.0599999999999987));
#65967=CARTESIAN_POINT('Ctrl Pts',(-0.319245655087293,-0.679866938257725,
-0.0599999999999985));
#65968=CARTESIAN_POINT('Ctrl Pts',(-0.286427032018807,-0.692461929359391,
-0.0599999999999983));
#65969=CARTESIAN_POINT('Ctrl Pts',(-0.252765977888783,-0.702775719150857,
-0.0599999999999996));
#65970=CARTESIAN_POINT('Ctrl Pts',(-0.21847902697937,-0.710686039402769,
-0.059999999999999));
#65971=CARTESIAN_POINT('Ctrl Pts',(-0.206107665761941,-0.713540228141817,
-0.0599999999999988));
#65972=CARTESIAN_POINT('Ctrl Pts',(-0.193654831169708,-0.716081022922348,
-0.0599999999999994));
#65973=CARTESIAN_POINT('Ctrl Pts',(-0.181130885406342,-0.718300992752236,
-0.0599999999999992));
#65974=CARTESIAN_POINT('Ctrl Pts',(-0.173595035779981,-0.719636782536796,
-0.059999999999999));
#65975=CARTESIAN_POINT('Ctrl Pts',(-0.166041024822709,-0.720854991242619,
-0.0600000000000011));
#65976=CARTESIAN_POINT('Ctrl Pts',(-0.158476926682109,-0.721953909943718,
-0.060000000000001));
#65977=CARTESIAN_POINT('Ctrl Pts',(-0.125718579853494,-0.726713070821577,
-0.0600000000000005));
#65978=CARTESIAN_POINT('Ctrl Pts',(-0.0927368516621256,-0.729244442193755,
-0.0600000000000052));
#65979=CARTESIAN_POINT('Ctrl Pts',(-0.0597155451061104,-0.729466847379534,
-0.0600000000000033));
#65980=CARTESIAN_POINT('Ctrl Pts',(-0.0298340896154985,-0.729668105032634,
-0.0600000000000016));
#65981=CARTESIAN_POINT('Ctrl Pts',(8.04126947938424E-5,-0.727977909840741,
-0.0599999999999993));
#65982=CARTESIAN_POINT('Ctrl Pts',(0.0298429891659583,-0.724431762203439,
-0.0600000000000001));
#65983=CARTESIAN_POINT('Ctrl Pts',(0.0450151293358453,-0.72262403399589,
-0.0600000000000005));
#65984=CARTESIAN_POINT('Ctrl Pts',(0.0601476579444566,-0.720333564472935,
-0.0599999999999992));
#65985=CARTESIAN_POINT('Ctrl Pts',(0.0752148178788815,-0.717562461013743,
-0.0599999999999992));
#65986=CARTESIAN_POINT('Ctrl Pts',(0.0841519166525747,-0.715918778632013,
-0.0599999999999991));
#65987=CARTESIAN_POINT('Ctrl Pts',(0.0930659974908798,-0.714105963589849,
-0.0600000000000014));
#65988=CARTESIAN_POINT('Ctrl Pts',(0.101951481945639,-0.712124184480052,
-0.0600000000000016));
#65989=CARTESIAN_POINT('Ctrl Pts',(0.108774015869091,-0.710602516722462,
-0.0600000000000018));
#65990=CARTESIAN_POINT('Ctrl Pts',(0.115570530759411,-0.708983264219682,
-0.0599999999999967));
#65991=CARTESIAN_POINT('Ctrl Pts',(0.12233784538292,-0.70726743743928,-0.0599999999999969));
#65992=CARTESIAN_POINT('Ctrl Pts',(0.155294287876727,-0.698911457295961,
-0.0599999999999979));
#65993=CARTESIAN_POINT('Ctrl Pts',(0.187566989762046,-0.688267264048053,
-0.0600000000000011));
#65994=CARTESIAN_POINT('Ctrl Pts',(0.218886517124081,-0.675398199752587,
-0.0600000000000005));
#65995=CARTESIAN_POINT('Ctrl Pts',(0.241740156394627,-0.666007733869806,
-0.06));
#65996=CARTESIAN_POINT('Ctrl Pts',(0.264086117884324,-0.655431560122243,
-0.0599999999999987));
#65997=CARTESIAN_POINT('Ctrl Pts',(0.285810299892495,-0.643679437283942,
-0.0599999999999986));
#65998=CARTESIAN_POINT('Ctrl Pts',(0.299989747415091,-0.636008786715737,
-0.0599999999999985));
#65999=CARTESIAN_POINT('Ctrl Pts',(0.313904101961907,-0.627836877170446,
-0.0599999999999994));
#66000=CARTESIAN_POINT('Ctrl Pts',(0.327530462491282,-0.619179691563123,
-0.0599999999999993));
#66001=CARTESIAN_POINT('Ctrl Pts',(0.334428494585131,-0.614797190158366,
-0.0599999999999992));
#66002=CARTESIAN_POINT('Ctrl Pts',(0.341252690027423,-0.610290304047882,
-0.0599999999999995));
#66003=CARTESIAN_POINT('Ctrl Pts',(0.347999856950083,-0.605660967794704,
-0.0599999999999994));
#66004=CARTESIAN_POINT('Ctrl Pts',(0.353764495005457,-0.601705759891582,
-0.0599999999999992));
#66005=CARTESIAN_POINT('Ctrl Pts',(0.359471946468096,-0.59766166929808,
-0.0600000000000004));
#66006=CARTESIAN_POINT('Ctrl Pts',(0.365110271189495,-0.593537654738276,
-0.0600000000000004));
#66007=CARTESIAN_POINT('Ctrl Pts',(0.392009677179333,-0.573862742874626,
-0.0600000000000001));
#66008=CARTESIAN_POINT('Ctrl Pts',(0.417402536256808,-0.552328568843849,
-0.059999999999997));
#66009=CARTESIAN_POINT('Ctrl Pts',(0.441115049422705,-0.529109016476954,
-0.059999999999997));
#66010=CARTESIAN_POINT('Ctrl Pts',(0.464440006753227,-0.506268963024899,
-0.059999999999997));
#66011=CARTESIAN_POINT('Ctrl Pts',(0.486139746646728,-0.481797195771757,
-0.0599999999999998));
#66012=CARTESIAN_POINT('Ctrl Pts',(0.506008214264659,-0.455831110125939,
-0.0599999999999989));
#66013=CARTESIAN_POINT('Ctrl Pts',(0.516926413410576,-0.441562123731379,
-0.0599999999999985));
#66014=CARTESIAN_POINT('Ctrl Pts',(0.527290837420226,-0.426841476968761,
-0.0599999999999988));
#66015=CARTESIAN_POINT('Ctrl Pts',(0.537060862935828,-0.411689834101626,
-0.0599999999999987));
#66016=CARTESIAN_POINT('Ctrl Pts',(-0.29260193430685,0.610169646934268,
-11.9749488707953));
#66017=CARTESIAN_POINT('Ctrl Pts',(-0.39411224040642,0.561491198135562,
-11.9696533379638));
#66018=CARTESIAN_POINT('Ctrl Pts',(-0.572019135180604,0.412886067482696,
-11.9590622723009));
#66019=CARTESIAN_POINT('Ctrl Pts',(-0.700345999063052,0.0876437013347023,
-11.9431756738065));
#66020=CARTESIAN_POINT('Ctrl Pts',(-0.655981217404692,-0.256375724037327,
-11.9272890753121));
#66021=CARTESIAN_POINT('Ctrl Pts',(-0.387452247378358,-0.637512366484492,
-11.9061069439862));
#66022=CARTESIAN_POINT('Ctrl Pts',(0.235314852578195,-0.765023683212307,
-11.879629279829));
#66023=CARTESIAN_POINT('Ctrl Pts',(0.77140418662287,-0.214212144206197,
-11.8478560828401));
#66024=CARTESIAN_POINT('Ctrl Pts',(0.626282581243407,0.404955323743999,
-11.8213784186828));
#66025=CARTESIAN_POINT('Ctrl Pts',(0.238575376523109,0.662775532235479,
-11.800196287357));
#66026=CARTESIAN_POINT('Ctrl Pts',(-0.1078208916813,0.6976941672648,-11.7843096888626));
#66027=CARTESIAN_POINT('Ctrl Pts',(-0.426851047433615,0.560357959801784,
-11.7684230903682));
#66028=CARTESIAN_POINT('Ctrl Pts',(-0.719896296594628,0.196619495603219,
-11.7472409590423));
#66029=CARTESIAN_POINT('Ctrl Pts',(-0.679657526711988,-0.308589625758868,
-11.7260588277165));
#66030=CARTESIAN_POINT('Ctrl Pts',(-0.332712891609252,-0.620107353319397,
-11.7048766963906));
#66031=CARTESIAN_POINT('Ctrl Pts',(0.116413504415669,-0.736688237868005,
-11.6836945650647));
#66032=CARTESIAN_POINT('Ctrl Pts',(0.675171437908528,-0.430783745523332,
-11.6572169009074));
#66033=CARTESIAN_POINT('Ctrl Pts',(0.726297966642536,0.336112054414775,
-11.6254437039186));
#66034=CARTESIAN_POINT('Ctrl Pts',(0.215357505998631,0.71407287292108,-11.5989660397613));
#66035=CARTESIAN_POINT('Ctrl Pts',(-0.247283197394635,0.659606503579982,
-11.5777839084354));
#66036=CARTESIAN_POINT('Ctrl Pts',(-0.533793635826822,0.461976473865101,
-11.5618973099411));
#66037=CARTESIAN_POINT('Ctrl Pts',(-0.688110478507896,0.150777350721831,
-11.5460107114466));
#66038=CARTESIAN_POINT('Ctrl Pts',(-0.675964715110877,-0.316165620402174,
-11.5248285801208));
#66039=CARTESIAN_POINT('Ctrl Pts',(-0.318270223098515,-0.675181839024747,
-11.5036464487949));
#66040=CARTESIAN_POINT('Ctrl Pts',(0.147840292895422,-0.688022737605352,
-11.4824643174691));
#66041=CARTESIAN_POINT('Ctrl Pts',(0.565623962158729,-0.486136361723975,
-11.4612821861432));
#66042=CARTESIAN_POINT('Ctrl Pts',(0.793479716880401,0.108734401743206,
-11.4348045219859));
#66043=CARTESIAN_POINT('Ctrl Pts',(0.335993916742615,0.726352298131389,
-11.4030313249971));
#66044=CARTESIAN_POINT('Ctrl Pts',(-0.298112918637422,0.683671975462962,
-11.3765536608398));
#66045=CARTESIAN_POINT('Ctrl Pts',(-0.615475022766798,0.342666648827597,
-11.3553715295139));
#66046=CARTESIAN_POINT('Ctrl Pts',(-0.705914102226468,0.00656161875215415,
-11.3394849310195));
#66047=CARTESIAN_POINT('Ctrl Pts',(-0.622077616086916,-0.330528871792904,
-11.3235983325252));
#66048=CARTESIAN_POINT('Ctrl Pts',(-0.310543480858139,-0.67856592981927,
-11.3024162011993));
#66049=CARTESIAN_POINT('Ctrl Pts',(0.194497940172004,-0.720650396469946,
-11.2812340698734));
#66050=CARTESIAN_POINT('Ctrl Pts',(0.558075706772724,-0.428699840487657,
-11.2600519385476));
#66051=CARTESIAN_POINT('Ctrl Pts',(0.745814935827746,-0.00437062783121209,
-11.2388698072217));
#66052=CARTESIAN_POINT('Ctrl Pts',(0.534393477883215,0.596537379583458,
-11.2123921430644));
#66053=CARTESIAN_POINT('Ctrl Pts',(-0.21411444420791,0.771125527228726,
-11.1806189460756));
#66054=CARTESIAN_POINT('Ctrl Pts',(-0.669795637756652,0.328104380872136,
-11.1541412819183));
#66055=CARTESIAN_POINT('Ctrl Pts',(-0.690935495823123,-0.137251874422689,
-11.1329591505924));
#66056=CARTESIAN_POINT('Ctrl Pts',(-0.542288925423647,-0.451973998913277,
-11.117072552098));
#66057=CARTESIAN_POINT('Ctrl Pts',(-0.260173180138369,-0.654629522639962,
-11.1011859536036));
#66058=CARTESIAN_POINT('Ctrl Pts',(0.20257790968715,-0.718227794756728,
-11.0800038222778));
#66059=CARTESIAN_POINT('Ctrl Pts',(0.61475932399721,-0.423364401158974,
-11.0588216909519));
#66060=CARTESIAN_POINT('Ctrl Pts',(0.702880058995295,0.0345205795692396,
-11.0376395596261));
#66061=CARTESIAN_POINT('Ctrl Pts',(0.571282631286294,0.479473853373007,
-11.0164574283002));
#66062=CARTESIAN_POINT('Ctrl Pts',(0.0211398831226441,0.800616225032851,
-10.9899797641429));
#66063=CARTESIAN_POINT('Ctrl Pts',(-0.66238604146316,0.449137290861845,
-10.9582065671541));
#66064=CARTESIAN_POINT('Ctrl Pts',(-0.722911249857644,-0.183515683067351,
-10.9317289029968));
#66065=CARTESIAN_POINT('Ctrl Pts',(-0.437774356145965,-0.551890885522362,
-10.9105467716709));
#66066=CARTESIAN_POINT('Ctrl Pts',(-0.120741175465174,-0.695542481001687,
-10.8946601731765));
#66067=CARTESIAN_POINT('Ctrl Pts',(0.225474399042472,-0.667376348810361,
-10.8787735746821));
#66068=CARTESIAN_POINT('Ctrl Pts',(0.619349525511595,-0.416287328540213,
-10.8575914433563));
#66069=CARTESIAN_POINT('Ctrl Pts',(0.7426298818878,0.0752814793781906,-10.8364093120304));
#66070=CARTESIAN_POINT('Ctrl Pts',(0.513381745134516,0.481322377944037,
-10.8152271807046));
#66071=CARTESIAN_POINT('Ctrl Pts',(0.12503781439124,0.735271763261725,-10.7940450493787));
#66072=CARTESIAN_POINT('Ctrl Pts',(-0.502168228339166,0.62390728869839,
-10.7675673852214));
#66073=CARTESIAN_POINT('Ctrl Pts',(-0.79561467114833,-0.0864688904838283,
-10.7357941882326));
#66074=CARTESIAN_POINT('Ctrl Pts',(-0.432196993595701,-0.60785231744993,
-10.7093165240753));
#66075=CARTESIAN_POINT('Ctrl Pts',(0.0236003080504614,-0.704040454719466,
-10.6881343927494));
#66076=CARTESIAN_POINT('Ctrl Pts',(0.358233295234271,-0.608298183883769,
-10.672247794255));
#66077=CARTESIAN_POINT('Ctrl Pts',(0.603882212681613,-0.36270672558111,
-10.6563611957606));
#66078=CARTESIAN_POINT('Ctrl Pts',(0.741547131220323,0.0836470372069074,
-10.6351790644348));
#66079=CARTESIAN_POINT('Ctrl Pts',(0.517292027842344,0.53812210560505,-10.6139969331089));
#66080=CARTESIAN_POINT('Ctrl Pts',(0.0797096438481298,0.699198412773276,
-10.5928148017831));
#66081=CARTESIAN_POINT('Ctrl Pts',(-0.380677283636059,0.641360917581681,
-10.5716326704572));
#66082=CARTESIAN_POINT('Ctrl Pts',(-0.786635906925367,0.150456586362906,
-10.5451550062999));
#66083=CARTESIAN_POINT('Ctrl Pts',(-0.550434349937227,-0.580948879314826,
-10.5133818093111));
#66084=CARTESIAN_POINT('Ctrl Pts',(0.0640780911147829,-0.743083225043802,
-10.4869041451538));
#66085=CARTESIAN_POINT('Ctrl Pts',(0.473750232264011,-0.521335452325531,
-10.4657220138279));
#66086=CARTESIAN_POINT('Ctrl Pts',(0.666825430939749,-0.231736097711846,
-10.4498354153335));
#66087=CARTESIAN_POINT('Ctrl Pts',(0.695072554279996,0.114472878279935,
-10.4339488168391));
#66088=CARTESIAN_POINT('Ctrl Pts',(0.511051301097596,0.5437973356877,-10.4127666855133));
#66089=CARTESIAN_POINT('Ctrl Pts',(0.0459205840941021,0.745021974552772,
-10.3915845541874));
#66090=CARTESIAN_POINT('Ctrl Pts',(-0.39187382810385,0.584522840096347,
-10.3704024228615));
#66091=CARTESIAN_POINT('Ctrl Pts',(-0.705335273549897,0.24240703942756,
-10.3492202915357));
#66092=CARTESIAN_POINT('Ctrl Pts',(-0.696965099795456,-0.394554031928942,
-10.3227426273783));
#66093=CARTESIAN_POINT('Ctrl Pts',(-0.0434573418998398,-0.79911891067786,
-10.2909694303896));
#66094=CARTESIAN_POINT('Ctrl Pts',(0.529876458749172,-0.524890102369867,
-10.2644917662322));
#66095=CARTESIAN_POINT('Ctrl Pts',(0.698575844497316,-0.0906737332777898,
-10.2433096349064));
#66096=CARTESIAN_POINT('Ctrl Pts',(0.658263143903542,0.255043932899648,
-10.227423036412));
#66097=CARTESIAN_POINT('Ctrl Pts',(0.455673622452517,0.537207078672659,
-10.2115364379176));
#66098=CARTESIAN_POINT('Ctrl Pts',(0.0374900855372222,0.745307633223355,
-10.1903543065917));
#66099=CARTESIAN_POINT('Ctrl Pts',(-0.447291532886714,0.597575708356613,
-10.1691721752659));
#66100=CARTESIAN_POINT('Ctrl Pts',(-0.677074909743126,0.191837468559726,
-10.14799004394));
#66101=CARTESIAN_POINT('Ctrl Pts',(-0.694522852254603,-0.271840079042577,
-10.1268079126142));
#66102=CARTESIAN_POINT('Ctrl Pts',(-0.275804889831566,-0.751907505740747,
-10.1003302484568));
#66103=CARTESIAN_POINT('Ctrl Pts',(0.484188776139409,-0.637213310460941,
-10.0685570514681));
#66104=CARTESIAN_POINT('Ctrl Pts',(0.743655850199394,-0.0570496061916968,
-10.0420793873107));
#66105=CARTESIAN_POINT('Ctrl Pts',(0.591145954131398,0.383114078749073,
-10.0208972559849));
#66106=CARTESIAN_POINT('Ctrl Pts',(0.336618815106218,0.62052038455411,-10.0050106574905));
#66107=CARTESIAN_POINT('Ctrl Pts',(-0.000452053710239919,0.704435725401867,
-9.98912405899608));
#66108=CARTESIAN_POINT('Ctrl Pts',(-0.453902103296527,0.592335931104618,
-9.96794192767022));
#66109=CARTESIAN_POINT('Ctrl Pts',(-0.727763581286154,0.165911459410156,
-9.94675979634436));
#66110=CARTESIAN_POINT('Ctrl Pts',(-0.640246728266517,-0.292089326561388,
-9.92557766501851));
#66111=CARTESIAN_POINT('Ctrl Pts',(-0.353382605913268,-0.65679506295015,
-9.90439553369265));
#66112=CARTESIAN_POINT('Ctrl Pts',(0.276533191529025,-0.751639959307012,
-9.87791786953533));
#66113=CARTESIAN_POINT('Ctrl Pts',(0.781545819003339,-0.172237355896938,
-9.84614467254655));
#66114=CARTESIAN_POINT('Ctrl Pts',(0.603738860340227,0.437924730538819,
-9.8196670083892));
#66115=CARTESIAN_POINT('Ctrl Pts',(0.202556190221955,0.674685798149359,
-9.79848487706338));
#66116=CARTESIAN_POINT('Ctrl Pts',(-0.145127604936405,0.690865944026855,
-9.78259827856895));
#66117=CARTESIAN_POINT('Ctrl Pts',(-0.456362724825398,0.536621802543421,
-9.76671168007457));
#66118=CARTESIAN_POINT('Ctrl Pts',(-0.729410114843622,0.157638380537224,
-9.74552954874872));
#66119=CARTESIAN_POINT('Ctrl Pts',(-0.662097903369506,-0.344663326978316,
-9.72434741742285));
#66120=CARTESIAN_POINT('Ctrl Pts',(-0.29890544321878,-0.637093073075865,
-9.70316528609701));
#66121=CARTESIAN_POINT('Ctrl Pts',(0.155832898486876,-0.729366251362731,
-9.68198315477112));
#66122=CARTESIAN_POINT('Ctrl Pts',(0.697347007828662,-0.393878642625726,
-9.65550549061384));
#66123=CARTESIAN_POINT('Ctrl Pts',(0.707185315458073,0.374657848667868,
-9.623732293625));
#66124=CARTESIAN_POINT('Ctrl Pts',(0.176672579446854,0.724614021927542,
-9.59725462946772));
#66125=CARTESIAN_POINT('Ctrl Pts',(-0.282373018168577,0.645364559789301,
-9.57607249814184));
#66126=CARTESIAN_POINT('Ctrl Pts',(-0.557848670468146,0.432622971174229,
-9.56018589964745));
#66127=CARTESIAN_POINT('Ctrl Pts',(-0.695218901859782,0.11358069409847,
-9.54429930115307));
#66128=CARTESIAN_POINT('Ctrl Pts',(-0.657997278472313,-0.352034879206046,
-9.52311716982719));
#66129=CARTESIAN_POINT('Ctrl Pts',(-0.281526301655526,-0.691309904519107,
-9.50193503850135));
#66130=CARTESIAN_POINT('Ctrl Pts',(0.184600760711549,-0.679083652352037,
-9.48075290717548));
#66131=CARTESIAN_POINT('Ctrl Pts',(0.590931414136129,-0.455037454134073,
-9.45957077584963));
#66132=CARTESIAN_POINT('Ctrl Pts',(0.786489778819108,0.151218590977907,
-9.43309311169231));
#66133=CARTESIAN_POINT('Ctrl Pts',(0.296474486791864,0.743358898950881,
-9.40131991470351));
#66134=CARTESIAN_POINT('Ctrl Pts',(-0.334422425230761,0.666663575280057,
-9.3748422505462));
#66135=CARTESIAN_POINT('Ctrl Pts',(-0.633000432686499,0.30909608318511,
-9.35366011922033));
#66136=CARTESIAN_POINT('Ctrl Pts',(-0.705246662148004,-0.0313834328873447,
-9.33777352072594));
#66137=CARTESIAN_POINT('Ctrl Pts',(-0.603416199871352,-0.363481478631069,
-9.32188692223156));
#66138=CARTESIAN_POINT('Ctrl Pts',(-0.273628850822219,-0.694273884466568,
-9.30070479090568));
#66139=CARTESIAN_POINT('Ctrl Pts',(0.23294438000554,-0.709156793970058,
-9.27952265957983));
#66140=CARTESIAN_POINT('Ctrl Pts',(0.580307452228801,-0.398089573632346,
-9.25834052825398));
#66141=CARTESIAN_POINT('Ctrl Pts',(0.744972095404132,0.0357155140929017,
-9.2371583969281));
#66142=CARTESIAN_POINT('Ctrl Pts',(0.501563565304761,0.624393485234313,
-9.2106807327708));
#66143=CARTESIAN_POINT('Ctrl Pts',(-0.255245053230173,0.758504803392499,
-9.17890753578199));
#66144=CARTESIAN_POINT('Ctrl Pts',(-0.68645998202962,0.291635687415495,
-9.15242987162469));
#66145=CARTESIAN_POINT('Ctrl Pts',(-0.682561214906084,-0.174184167844268,
-9.13124774029882));
#66146=CARTESIAN_POINT('Ctrl Pts',(-0.517216387829029,-0.48046329983859,
-9.11536114180443));
#66147=CARTESIAN_POINT('Ctrl Pts',(-0.224617670094119,-0.667665183948138,
-9.09947454331003));
#66148=CARTESIAN_POINT('Ctrl Pts',(0.240882484103758,-0.706303478333916,
-9.07829241198417));
#66149=CARTESIAN_POINT('Ctrl Pts',(0.636622435975274,-0.389715686909015,
-9.05711028065832));
#66150=CARTESIAN_POINT('Ctrl Pts',(0.700009260781494,0.0722432181399054,
-9.03592814933246));
#66151=CARTESIAN_POINT('Ctrl Pts',(0.544690364967499,0.509481527819525,
-9.0147460180066));
#66152=CARTESIAN_POINT('Ctrl Pts',(-0.0219154922400167,0.800595369487078,
-8.98826835384928));
#66153=CARTESIAN_POINT('Ctrl Pts',(-0.685565357771946,0.412891891650819,
-8.95649515686049));
#66154=CARTESIAN_POINT('Ctrl Pts',(-0.712004562954644,-0.22209948994579,
-8.93001749270316));
#66155=CARTESIAN_POINT('Ctrl Pts',(-0.407483346505639,-0.574619229353,-8.90883536137732));
#66156=CARTESIAN_POINT('Ctrl Pts',(-0.0831884995869038,-0.701025996570153,
-8.89294876288291));
#66157=CARTESIAN_POINT('Ctrl Pts',(0.261013149201355,-0.654295064568733,
-8.87706216438852));
#66158=CARTESIAN_POINT('Ctrl Pts',(0.640825685227696,-0.382402165013538,
-8.85588003306267));
#66159=CARTESIAN_POINT('Ctrl Pts',(0.737511168356077,0.11508135887323,-8.8346979017368));
#66160=CARTESIAN_POINT('Ctrl Pts',(0.486773807622215,0.508215808451524,
-8.81351577041096));
#66161=CARTESIAN_POINT('Ctrl Pts',(0.0853438924577135,0.740928769112059,
-8.79233363908507));
#66162=CARTESIAN_POINT('Ctrl Pts',(-0.534971139146889,0.596019391231656,
-8.76585597492778));
#66163=CARTESIAN_POINT('Ctrl Pts',(-0.789818186168672,-0.12909998747171,
-8.73408277793897));
#66164=CARTESIAN_POINT('Ctrl Pts',(-0.398906696132759,-0.630200070519562,
-8.70760511378165));
#66165=CARTESIAN_POINT('Ctrl Pts',(0.061401085864204,-0.701754831174225,
-8.68642298245581));
#66166=CARTESIAN_POINT('Ctrl Pts',(0.390405367007379,-0.588167853373958,
-8.67053638396139));
#66167=CARTESIAN_POINT('Ctrl Pts',(0.622501320628285,-0.329730194842773,
-8.65464978546701));
#66168=CARTESIAN_POINT('Ctrl Pts',(0.735980420215885,0.123376641684858,
-8.63346765414115));
#66169=CARTESIAN_POINT('Ctrl Pts',(0.487626042973425,0.565143596640834,
-8.61228552281528));
#66170=CARTESIAN_POINT('Ctrl Pts',(0.0420197908343311,0.702471625708329,
-8.59110339148945));
#66171=CARTESIAN_POINT('Ctrl Pts',(-0.414593702842348,0.619976678949471,
-8.56992126016356));
#66172=CARTESIAN_POINT('Ctrl Pts',(-0.793584686296887,0.107965643235917,
-8.54344359600627));
#66173=CARTESIAN_POINT('Ctrl Pts',(-0.518418978391269,-0.609689541333719,
-8.51167039901745));
#66174=CARTESIAN_POINT('Ctrl Pts',(0.10391852221122,-0.738565922476695,
-8.48519273486015));
#66175=CARTESIAN_POINT('Ctrl Pts',(0.501082034024498,-0.495122945943268,
-8.46401060353428));
#66176=CARTESIAN_POINT('Ctrl Pts',(0.678315270358112,-0.195566276054168,
-8.44812400503989));
#66177=CARTESIAN_POINT('Ctrl Pts',(0.687916430292161,0.151660411805788,
-8.43223740654549));
#66178=CARTESIAN_POINT('Ctrl Pts',(0.481089349371821,0.570475251501399,
-8.41105527521963));
#66179=CARTESIAN_POINT('Ctrl Pts',(0.00581701517587562,0.746413159680681,
-8.38987314389378));
#66180=CARTESIAN_POINT('Ctrl Pts',(-0.422719610264708,0.562619035266954,
-8.36869101256792));
#66181=CARTESIAN_POINT('Ctrl Pts',(-0.717342918101181,0.204152292977149,
-8.34750888124207));
#66182=CARTESIAN_POINT('Ctrl Pts',(-0.674754780631321,-0.43143854772082,
-8.32103121708474));
#66183=CARTESIAN_POINT('Ctrl Pts',(-0.000450182530976969,-0.800299550983042,
-8.28925802009595));
#66184=CARTESIAN_POINT('Ctrl Pts',(0.55731818268824,-0.495656256237618,
-8.26278035593863));
#66185=CARTESIAN_POINT('Ctrl Pts',(0.70243916327569,-0.0530014935470479,
-8.24159822461277));
#66186=CARTESIAN_POINT('Ctrl Pts',(0.643605972302399,0.290050214182614,
-8.22571162611838));
#66187=CARTESIAN_POINT('Ctrl Pts',(0.426145850537514,0.56091854100633,-8.20982502762398));
#66188=CARTESIAN_POINT('Ctrl Pts',(-0.00261665234877711,0.746245353610373,
-8.18864289629813));
#66189=CARTESIAN_POINT('Ctrl Pts',(-0.478758691882225,0.5726749143775,-8.16746076497226));
#66190=CARTESIAN_POINT('Ctrl Pts',(-0.686405800501428,0.155174497856633,
-8.14627863364641));
#66191=CARTESIAN_POINT('Ctrl Pts',(-0.678910665854216,-0.308770673262746,
-8.12509650232055));
#66192=CARTESIAN_POINT('Ctrl Pts',(-0.234999107869971,-0.765642641017721,
-8.09861883816322));
#66193=CARTESIAN_POINT('Ctrl Pts',(0.517732728409698,-0.610272394838091,
-8.06684564117445));
#66194=CARTESIAN_POINT('Ctrl Pts',(0.745647079045141,-0.0170033706618007,
-8.04036797701711));
#66195=CARTESIAN_POINT('Ctrl Pts',(0.569703324557914,0.414328442674807,
-8.01918584569126));
#66196=CARTESIAN_POINT('Ctrl Pts',(0.302785852511827,0.637713495113113,
-8.00329924719686));
#66197=CARTESIAN_POINT('Ctrl Pts',(-0.0383075228840123,0.70339350954178,
-7.98741264870248));
#66198=CARTESIAN_POINT('Ctrl Pts',(-0.485078126151442,0.567087459025494,
-7.96623051737661));
#66199=CARTESIAN_POINT('Ctrl Pts',(-0.735627971573747,0.126561961300988,
-7.94504838605076));
#66200=CARTESIAN_POINT('Ctrl Pts',(-0.62362478459429,-0.326073880871788,
-7.92386625472489));
#66201=CARTESIAN_POINT('Ctrl Pts',(-0.317576031167041,-0.674836636013439,
-7.90268412339904));
#66202=CARTESIAN_POINT('Ctrl Pts',(0.316526456894863,-0.73569303145392,
-7.87620645924171));
#66203=CARTESIAN_POINT('Ctrl Pts',(0.789672444363271,-0.129988478648325,
-7.84443326225293));
#66204=CARTESIAN_POINT('Ctrl Pts',(0.579332529080104,0.469736630306881,
-7.81795559809561));
#66205=CARTESIAN_POINT('Ctrl Pts',(0.166006120765101,0.684596161463233,
-7.79677346676974));
#66206=CARTESIAN_POINT('Ctrl Pts',(-0.182044780093774,0.68206852468891,
-7.78088686827537));
#66207=CARTESIAN_POINT('Ctrl Pts',(-0.484541134815908,0.511321605495331,
-7.76500026978095));
#66208=CARTESIAN_POINT('Ctrl Pts',(-0.736827533578104,0.118212353059201,
-7.74381813845511));
#66209=CARTESIAN_POINT('Ctrl Pts',(-0.642619076480737,-0.379746185172546,
-7.72263600712924));
#66210=CARTESIAN_POINT('Ctrl Pts',(-0.264236366826861,-0.652235532758837,
-7.70145387580339));
#66211=CARTESIAN_POINT('Ctrl Pts',(0.194803596959322,-0.719937899745148,
-7.68027174447751));
#66212=CARTESIAN_POINT('Ctrl Pts',(0.717506225022208,-0.355834303431602,
-7.65379408032022));
#66213=CARTESIAN_POINT('Ctrl Pts',(0.686029441622246,0.412120345524747,
-7.62202088333141));
#66214=CARTESIAN_POINT('Ctrl Pts',(0.137476787506733,0.733061262105183,
-7.59554321917409));
#66215=CARTESIAN_POINT('Ctrl Pts',(-0.316646643148811,0.629257371672559,
-7.57436108784824));
#66216=CARTESIAN_POINT('Ctrl Pts',(-0.580291571614595,0.402019236161356,
-7.55847448935384));
#66217=CARTESIAN_POINT('Ctrl Pts',(-0.700318083314065,0.0760557542749098,
-7.54258789085945));
#66218=CARTESIAN_POINT('Ctrl Pts',(-0.638128232498241,-0.386886719264509,
-7.52140575953358));
#66219=CARTESIAN_POINT('Ctrl Pts',(-0.243968745432271,-0.705440071063631,
-7.50022362820774));
#66220=CARTESIAN_POINT('Ctrl Pts',(0.22082772031363,-0.66818198545617,-7.47904149688187));
#66221=CARTESIAN_POINT('Ctrl Pts',(0.614531056354557,-0.422623475038358,
-7.45785936555602));
#66222=CARTESIAN_POINT('Ctrl Pts',(0.777226853872599,0.193265755020321,
-7.43138170139868));
#66223=CARTESIAN_POINT('Ctrl Pts',(0.256098235933003,0.758217163825756,
-7.39960850440991));
#66224=CARTESIAN_POINT('Ctrl Pts',(-0.369765439283066,0.64772849328574,
-7.37313084025257));
#66225=CARTESIAN_POINT('Ctrl Pts',(-0.64869644763536,0.27463221815172,-7.35194870892673));
#66226=CARTESIAN_POINT('Ctrl Pts',(-0.70254103328265,-0.0692377850948682,
-7.33606211043233));
#66227=CARTESIAN_POINT('Ctrl Pts',(-0.583010888431519,-0.39538361061797,
-7.32017551193793));
#66228=CARTESIAN_POINT('Ctrl Pts',(-0.235923423345702,-0.707975361839259,
-7.29899338061208));
#66229=CARTESIAN_POINT('Ctrl Pts',(0.270717601992387,-0.695613702123204,
-7.27781124928622));
#66230=CARTESIAN_POINT('Ctrl Pts',(0.600862087662645,-0.366328813167557,
-7.25662911796036));
#66231=CARTESIAN_POINT('Ctrl Pts',(0.741976258067605,0.0756984368513641,
-7.23544698663451));
#66232=CARTESIAN_POINT('Ctrl Pts',(0.467284115457725,0.650445070613317,
-7.20896932247717));
#66233=CARTESIAN_POINT('Ctrl Pts',(-0.295637994600642,0.743691972604572,
-7.1771961254884));
#66234=CARTESIAN_POINT('Ctrl Pts',(-0.701140431554866,0.254324156032159,
-7.15071846133106));
#66235=CARTESIAN_POINT('Ctrl Pts',(-0.672214306820377,-0.210613062576066,
-7.12953633000522));
#66236=CARTESIAN_POINT('Ctrl Pts',(-0.49064907573534,-0.507564044048387,
-7.11364973151081));
#66237=CARTESIAN_POINT('Ctrl Pts',(-0.188413006671554,-0.678771268169181,
-7.09776313301643));
#66238=CARTESIAN_POINT('Ctrl Pts',(0.278490899227765,-0.692337918723144,
-7.07658100169056));
#66239=CARTESIAN_POINT('Ctrl Pts',(0.656645685556425,-0.354940679903258,
-7.05539887036471));
#66240=CARTESIAN_POINT('Ctrl Pts',(0.695115409901483,0.109757071136956,
-7.03421673903885));
#66241=CARTESIAN_POINT('Ctrl Pts',(0.516523923338716,0.538016781798218,
-7.01303460771299));
#66242=CARTESIAN_POINT('Ctrl Pts',(-0.0649075310191635,0.798260763698985,
-6.98655694355567));
#66243=CARTESIAN_POINT('Ctrl Pts',(-0.706763364828739,0.375453219594602,
-6.95478374656687));
#66244=CARTESIAN_POINT('Ctrl Pts',(-0.699040156518267,-0.260041421079877,
-6.92830608240956));
#66245=CARTESIAN_POINT('Ctrl Pts',(-0.376014694915819,-0.595686902348158,
-6.90712395108369));
#66246=CARTESIAN_POINT('Ctrl Pts',(-0.0453954058664428,-0.704483521068271,
-6.89123735258931));
#66247=CARTESIAN_POINT('Ctrl Pts',(0.295797561700471,-0.639322843379747,
-6.8753507540949));
#66248=CARTESIAN_POINT('Ctrl Pts',(0.660449835001555,-0.347411845079441,
-6.85416862276907));
#66249=CARTESIAN_POINT('Ctrl Pts',(0.730261020256401,0.154548648981848,
-6.83298649144319));
#66250=CARTESIAN_POINT('Ctrl Pts',(0.458759075795143,0.533640476468047,
-6.81180436011734));
#66251=CARTESIAN_POINT('Ctrl Pts',(0.0454033235137405,0.744444463400547,
-6.79062222879148));
#66252=CARTESIAN_POINT('Ctrl Pts',(-0.566227963559903,0.566408975674883,
-6.76414456463416));
#66253=CARTESIAN_POINT('Ctrl Pts',(-0.781739097417529,-0.171357980727822,
-6.73237136764536));
#66254=CARTESIAN_POINT('Ctrl Pts',(-0.36446354353643,-0.650726522050533,
-6.70589370348805));
#66255=CARTESIAN_POINT('Ctrl Pts',(0.0990244122389695,-0.697441110221215,
-6.68471157216218));
#66256=CARTESIAN_POINT('Ctrl Pts',(0.421449152886381,-0.566337695957096,
-6.6688249736678));
#66257=CARTESIAN_POINT('Ctrl Pts',(0.639321376606824,-0.295800731727484,
-6.6529383751734));
#66258=CARTESIAN_POINT('Ctrl Pts',(0.72828669883045,0.162749683301894,-6.63175624384754));
#66259=CARTESIAN_POINT('Ctrl Pts',(0.456550800284682,0.590531801388853,
-6.61057411252168));
#66260=CARTESIAN_POINT('Ctrl Pts',(0.00420849966872835,0.703714670097329,
-6.58939198119583));
#66261=CARTESIAN_POINT('Ctrl Pts',(-0.447311932305929,0.59680068373128,
-6.56820984986996));
#66262=CARTESIAN_POINT('Ctrl Pts',(-0.798239973579876,0.0651626776248776,
-6.54173218571265));
#66263=CARTESIAN_POINT('Ctrl Pts',(-0.484905362068866,-0.63666818193181,
-6.50995898872385));
#66264=CARTESIAN_POINT('Ctrl Pts',(0.143458633831261,-0.731914130435804,
-6.48348132456653));
#66265=CARTESIAN_POINT('Ctrl Pts',(0.526965677843967,-0.467479525104637,
-6.46229919324067));
#66266=CARTESIAN_POINT('Ctrl Pts',(0.687844780422188,-0.158831240600472,
-6.44641259474628));
#66267=CARTESIAN_POINT('Ctrl Pts',(0.678772152266887,0.188409603808886,
-6.43052599625188));
#66268=CARTESIAN_POINT('Ctrl Pts',(0.449737145934374,0.595504557883058,
-6.40934386492603));
#66269=CARTESIAN_POINT('Ctrl Pts',(-0.0343035843211689,0.745647019873919,
-6.38816173360018));
#66270=CARTESIAN_POINT('Ctrl Pts',(-0.452343460848582,0.539089431506795,
-6.36697960227431));
#66271=CARTESIAN_POINT('Ctrl Pts',(-0.727278014373636,0.165307092403316,
-6.34579747094845));
#66272=CARTESIAN_POINT('Ctrl Pts',(-0.650593119328475,-0.467075239707729,
-6.31931980679114));
#66273=CARTESIAN_POINT('Ctrl Pts',(0.042556028366106,-0.799168971730803,
-6.28754660980234));
#66274=CARTESIAN_POINT('Ctrl Pts',(0.58315304606446,-0.46498710724797,-6.26106894564502));
#66275=CARTESIAN_POINT('Ctrl Pts',(0.704267131783399,-0.0151800071787377,
-6.23988681431916));
#66276=CARTESIAN_POINT('Ctrl Pts',(0.627100262560229,0.324226811612303,
-6.22400021582477));
#66277=CARTESIAN_POINT('Ctrl Pts',(0.395365052280528,0.582992949678207,
-6.20811361733038));
#66278=CARTESIAN_POINT('Ctrl Pts',(-0.0426668885056882,0.745062854587275,
-6.18693148600451));
#66279=CARTESIAN_POINT('Ctrl Pts',(-0.508936057342763,0.546049163939659,
-6.16574935467866));
#66280=CARTESIAN_POINT('Ctrl Pts',(-0.693643268548973,0.118144784487239,
-6.1445672233528));
#66281=CARTESIAN_POINT('Ctrl Pts',(-0.661592512142315,-0.344999832528101,
-6.12338509202694));
#66282=CARTESIAN_POINT('Ctrl Pts',(-0.192973643036106,-0.776760719460778,
-6.09690742786962));
#66283=CARTESIAN_POINT('Ctrl Pts',(0.548852666849259,-0.58226923395591,
-6.06513423088083));
#66284=CARTESIAN_POINT('Ctrl Pts',(0.786505655010167,0.145511346935457,
-6.03336103389204));
#66285=CARTESIAN_POINT('Ctrl Pts',(0.303954112232331,0.739849035349103,
-6.00158783690326));
#66286=CARTESIAN_POINT('Ctrl Pts',(-0.457122405947255,0.656746386895383,
-5.96981463991447));
#66287=CARTESIAN_POINT('Ctrl Pts',(-0.799835382276926,-0.0293155839405517,
-5.93804144292568));
#66288=CARTESIAN_POINT('Ctrl Pts',(-0.473532610433715,-0.576625011097358,
-5.91156377876836));
#66289=CARTESIAN_POINT('Ctrl Pts',(-0.0268458389766041,-0.703120526676957,
-5.8903816474425));
#66290=CARTESIAN_POINT('Ctrl Pts',(0.429873304441071,-0.610241380137162,
-5.86919951611663));
#66291=CARTESIAN_POINT('Ctrl Pts',(0.72041369487452,-0.194790217664389,
-5.84801738479079));
#66292=CARTESIAN_POINT('Ctrl Pts',(0.651769364779252,0.267190941228426,
-5.82683525346492));
#66293=CARTESIAN_POINT('Ctrl Pts',(0.446117917906169,0.547134871850125,
-5.81094865497054));
#66294=CARTESIAN_POINT('Ctrl Pts',(0.129797396400296,0.692369309990026,
-5.79506205647613));
#66295=CARTESIAN_POINT('Ctrl Pts',(-0.335295695534132,0.666226148989499,
-5.77387992515028));
#66296=CARTESIAN_POINT('Ctrl Pts',(-0.773388981349555,0.205794908719004,
-5.74740226099296));
#66297=CARTESIAN_POINT('Ctrl Pts',(-0.590746005142289,-0.540786319976765,
-5.71562906400416));
#66298=CARTESIAN_POINT('Ctrl Pts',(0.0124024706309206,-0.745725099290851,
-5.68915139984685));
#66299=CARTESIAN_POINT('Ctrl Pts',(0.434685861821545,-0.553425896816594,
-5.66796926852099));
#66300=CARTESIAN_POINT('Ctrl Pts',(0.72270319551117,-0.18672521346106,-5.64678713719512));
#66301=CARTESIAN_POINT('Ctrl Pts',(0.675182030054888,0.317833927049418,
-5.62560500586928));
#66302=CARTESIAN_POINT('Ctrl Pts',(0.323809686428931,0.625601391043243,
-5.6044228745434));
#66303=CARTESIAN_POINT('Ctrl Pts',(-0.0141641249760513,0.705802509565102,
-5.58853627604902));
#66304=CARTESIAN_POINT('Ctrl Pts',(-0.349275640818321,0.611748689208698,
-5.57264967755462));
#66305=CARTESIAN_POINT('Ctrl Pts',(-0.686843080444304,0.290732276842646,
-5.55146754622876));
#66306=CARTESIAN_POINT('Ctrl Pts',(-0.72269141693145,-0.343797469364027,
-5.52498988207144));
#66307=CARTESIAN_POINT('Ctrl Pts',(-0.100182069364385,-0.794604796709607,
-5.49321668508265));
#66308=CARTESIAN_POINT('Ctrl Pts',(0.492200104289347,-0.56035531426314,
-5.46673902092533));
#66309=CARTESIAN_POINT('Ctrl Pts',(0.689575122107159,-0.140421506011553,
-5.44555688959948));
#66310=CARTESIAN_POINT('Ctrl Pts',(0.671714796398658,0.325523691904682,
-5.42437475827361));
#66311=CARTESIAN_POINT('Ctrl Pts',(0.308866959837698,0.679330682531593,
-5.40319262694776));
#66312=CARTESIAN_POINT('Ctrl Pts',(-0.158179798246442,0.686446681763176,
-5.3820104956219));
#66313=CARTESIAN_POINT('Ctrl Pts',(-0.467698735375229,0.528786977202589,
-5.36612389712751));
#66314=CARTESIAN_POINT('Ctrl Pts',(-0.662231679827364,0.240164815655626,
-5.35023729863311));
#66315=CARTESIAN_POINT('Ctrl Pts',(-0.711711733586907,-0.223036071840036,
-5.32905516730725));
#66316=CARTESIAN_POINT('Ctrl Pts',(-0.328270635324783,-0.729875307140714,
-5.30257750314993));
#66317=CARTESIAN_POINT('Ctrl Pts',(0.438031486668258,-0.670493587687057,
-5.27080430616114));
#66318=CARTESIAN_POINT('Ctrl Pts',(0.737897769931333,-0.108470742618401,
-5.24432664200382));
#66319=CARTESIAN_POINT('Ctrl Pts',(0.616490027294739,0.339370143052669,
-5.22314451067796));
#66320=CARTESIAN_POINT('Ctrl Pts',(0.301246298432971,0.682947370072152,
-5.2019623793521));
#66321=CARTESIAN_POINT('Ctrl Pts',(-0.204350803094626,0.717725381973961,
-5.18078024802625));
#66322=CARTESIAN_POINT('Ctrl Pts',(-0.564936112187733,0.420805281242191,
-5.15959811670039));
#66323=CARTESIAN_POINT('Ctrl Pts',(-0.698787211838258,0.100270668202826,
-5.14371151820599));
#66324=CARTESIAN_POINT('Ctrl Pts',(-0.660218179971166,-0.245645865540907,
-5.1278249197116));
#66325=CARTESIAN_POINT('Ctrl Pts',(-0.398077205723047,-0.630724360863014,
-5.10664278838574));
#66326=CARTESIAN_POINT('Ctrl Pts',(0.222281684997194,-0.768811047320993,
-5.08016512422842));
#66327=CARTESIAN_POINT('Ctrl Pts',(0.767909224957921,-0.227483310747878,
-5.04839192723964));
#66328=CARTESIAN_POINT('Ctrl Pts',(0.632637701696453,0.39500450537932,-5.0219142630823));
#66329=CARTESIAN_POINT('Ctrl Pts',(0.250190952797296,0.657751119258226,
-5.00073213175645));
#66330=CARTESIAN_POINT('Ctrl Pts',(-0.212500472627088,0.715548734708769,
-4.97955000043058));
#66331=CARTESIAN_POINT('Ctrl Pts',(-0.620375570452808,0.414756707287463,
-4.95836786910474));
#66332=CARTESIAN_POINT('Ctrl Pts',(-0.702998434927052,-0.0449788401932196,
-4.93718573777888));
#66333=CARTESIAN_POINT('Ctrl Pts',(-0.597519655454011,-0.375936212244599,
-4.92129913928448));
#66334=CARTESIAN_POINT('Ctrl Pts',(-0.344192787318138,-0.61462286125708,
-4.90541254079009));
#66335=CARTESIAN_POINT('Ctrl Pts',(0.104890152807889,-0.738428559135105,
-4.88423040946423));
#66336=CARTESIAN_POINT('Ctrl Pts',(0.66711275320734,-0.442086132417752,
-4.85775274530691));
#66337=CARTESIAN_POINT('Ctrl Pts',(0.732555231440372,0.323722207044275,
-4.82597954831811));
#66338=CARTESIAN_POINT('Ctrl Pts',(0.226483522681462,0.710608355447316,
-4.7995018841608));
#66339=CARTESIAN_POINT('Ctrl Pts',(-0.235103534183009,0.66329358202965,
-4.77831975283493));
#66340=CARTESIAN_POINT('Ctrl Pts',(-0.6251781158456,0.407821978414359,-4.75713762150909));
#66341=CARTESIAN_POINT('Ctrl Pts',(-0.741338321875117,-0.0854778753477755,
-4.73595549018322));
#66342=CARTESIAN_POINT('Ctrl Pts',(-0.506701789827963,-0.489370199092825,
-4.71477335885737));
#66343=CARTESIAN_POINT('Ctrl Pts',(-0.212060776109364,-0.673340925212919,
-4.69888676036297));
#66344=CARTESIAN_POINT('Ctrl Pts',(0.13553701687756,-0.691273935193279,
-4.68300016186857));
#66345=CARTESIAN_POINT('Ctrl Pts',(0.557969828113902,-0.494922571739213,
-4.66181803054273));
#66346=CARTESIAN_POINT('Ctrl Pts',(0.794652742927993,0.0949030669946144,
-4.63534036638539));
#66347=CARTESIAN_POINT('Ctrl Pts',(0.348784514783706,0.720959497261372,
-4.6035671693966));
#66348=CARTESIAN_POINT('Ctrl Pts',(-0.287390379613016,0.68823381970347,
-4.57708950523929));
#66349=CARTESIAN_POINT('Ctrl Pts',(-0.608578462087337,0.353361434271592,
-4.55590737391342));
#66350=CARTESIAN_POINT('Ctrl Pts',(-0.740509564330208,-0.0938724014049983,
-4.53472524258757));
#66351=CARTESIAN_POINT('Ctrl Pts',(-0.509706951025825,-0.545057610469336,
-4.51354311126171));
#66352=CARTESIAN_POINT('Ctrl Pts',(-0.0694084667398682,-0.701008102891709,
-4.49236097993585));
#66353=CARTESIAN_POINT('Ctrl Pts',(0.274258103338072,-0.650492326691175,
-4.47647438144146));
#66354=CARTESIAN_POINT('Ctrl Pts',(0.550802926396446,-0.439142428711666,
-4.46058778294706));
#66355=CARTESIAN_POINT('Ctrl Pts',(0.745668804766385,-0.0160223188298255,
-4.4394056516212));
#66356=CARTESIAN_POINT('Ctrl Pts',(0.544241292482002,0.586754624630679,
-4.41292798746388));
#66357=CARTESIAN_POINT('Ctrl Pts',(-0.200874523336002,0.775295208497259,
-4.3811547904751));
#66358=CARTESIAN_POINT('Ctrl Pts',(-0.664576138776499,0.338522638307489,
-4.35467712631776));
#66359=CARTESIAN_POINT('Ctrl Pts',(-0.69260229547609,-0.124635901923627,
-4.33349499499192));
#66360=CARTESIAN_POINT('Ctrl Pts',(-0.503641062853606,-0.550919342933017,
-4.31231286366604));
#66361=CARTESIAN_POINT('Ctrl Pts',(-0.0356495923251104,-0.745397934811761,
-4.29113073234021));
#66362=CARTESIAN_POINT('Ctrl Pts',(0.400896797976255,-0.579233677324962,
-4.26994860101433));
#66363=CARTESIAN_POINT('Ctrl Pts',(0.630134791455414,-0.318257629803494,
-4.25406200251995));
#66364=CARTESIAN_POINT('Ctrl Pts',(0.704096847355287,0.0218532827285811,
-4.23817540402554));
#66365=CARTESIAN_POINT('Ctrl Pts',(0.578714001944864,0.47049844320186,-4.21699327269969));
#66366=CARTESIAN_POINT('Ctrl Pts',(0.0349786870852126,0.799534905690655,
-4.19051560854237));
#66367=CARTESIAN_POINT('Ctrl Pts',(-0.65499394863327,0.460886278487515,
-4.15874241155358));
#66368=CARTESIAN_POINT('Ctrl Pts',(-0.725677279864578,-0.172196127616421,
-4.13226474739626));
#66369=CARTESIAN_POINT('Ctrl Pts',(-0.447211755898116,-0.54335411393822,
-4.1110826160704));
#66370=CARTESIAN_POINT('Ctrl Pts',(-0.027231621354319,-0.745938926057937,
-4.08990048474455));
#66371=CARTESIAN_POINT('Ctrl Pts',(0.455363367272391,-0.591213310405756,
-4.06871835341868));
#66372=CARTESIAN_POINT('Ctrl Pts',(0.680528182180706,-0.181965075860278,
-4.04753622209283));
#66373=CARTESIAN_POINT('Ctrl Pts',(0.686307798878026,0.165346241353982,
-4.03164962359843));
#66374=CARTESIAN_POINT('Ctrl Pts',(0.522509375349723,0.472455171517164,
-4.01576302510404));
#66375=CARTESIAN_POINT('Ctrl Pts',(0.136512190381233,0.733241503857858,
-3.99458089377818));
#66376=CARTESIAN_POINT('Ctrl Pts',(-0.490920424353534,0.632041700301898,
-3.96810322962086));
#66377=CARTESIAN_POINT('Ctrl Pts',(-0.797586221486274,-0.072728630810176,
-3.93633003263207));
#66378=CARTESIAN_POINT('Ctrl Pts',(-0.441632977912428,-0.601015252466975,
-3.90985236847475));
#66379=CARTESIAN_POINT('Ctrl Pts',(0.0108809088601417,-0.703643129412517,
-3.88867023714889));
#66380=CARTESIAN_POINT('Ctrl Pts',(0.462129679432592,-0.586176255061214,
-3.86748810582303));
#66381=CARTESIAN_POINT('Ctrl Pts',(0.729797145596839,-0.15583677657501,
-3.84630597449717));
#66382=CARTESIAN_POINT('Ctrl Pts',(0.636487863470664,0.301849457891777,
-3.82512384317132));
#66383=CARTESIAN_POINT('Ctrl Pts',(0.416060211528914,0.570308403158517,
-3.80923724467692));
#66384=CARTESIAN_POINT('Ctrl Pts',(0.0924068473382293,0.698348703003505,
-3.79335064618252));
#66385=CARTESIAN_POINT('Ctrl Pts',(-0.370617326288914,0.647241437607997,
-3.77216851485667));
#66386=CARTESIAN_POINT('Ctrl Pts',(-0.783328765084108,0.163937853346245,
-3.74569085069934));
#66387=CARTESIAN_POINT('Ctrl Pts',(-0.560831837890227,-0.571752467465549,
-3.71391765371057));
#66388=CARTESIAN_POINT('Ctrl Pts',(0.0524600799429356,-0.743980484213214,
-3.68743998955323));
#66389=CARTESIAN_POINT('Ctrl Pts',(0.463798413511565,-0.529266548509558,
-3.66625785822738));
#66390=CARTESIAN_POINT('Ctrl Pts',(0.731693616604151,-0.147617390678711,
-3.64507572690151));
#66391=CARTESIAN_POINT('Ctrl Pts',(0.65712599706795,0.353658590496596,-3.62389359557566));
#66392=CARTESIAN_POINT('Ctrl Pts',(0.289722226326614,0.642098845309166,
-3.6027114642498));
#66393=CARTESIAN_POINT('Ctrl Pts',(-0.0520732543285767,0.704021413391895,
-3.58682486575541));
#66394=CARTESIAN_POINT('Ctrl Pts',(-0.381646074532144,0.592094764557056,
-3.57093826726101));
#66395=CARTESIAN_POINT('Ctrl Pts',(-0.7014744353342,0.253401455550246,-3.54975613593516));
#66396=CARTESIAN_POINT('Ctrl Pts',(-0.703171557501552,-0.382137847757598,
-3.52327847177783));
#66397=CARTESIAN_POINT('Ctrl Pts',(-0.0573355312236082,-0.798840329041782,
-3.49150527478905));
#66398=CARTESIAN_POINT('Ctrl Pts',(0.521602160227078,-0.533094932750431,
-3.46502761063172));
#66399=CARTESIAN_POINT('Ctrl Pts',(0.696124873969488,-0.103161075934814,
-3.44384547930587));
#66400=CARTESIAN_POINT('Ctrl Pts',(0.653250630478223,0.361151016044349,
-3.42266334798001));
#66401=CARTESIAN_POINT('Ctrl Pts',(0.271913654699282,0.69494743617245,-3.40148121665415));
#66402=CARTESIAN_POINT('Ctrl Pts',(-0.194840623075141,0.676954228271529,
-3.38029908532829));
#66403=CARTESIAN_POINT('Ctrl Pts',(-0.495439723982,0.50288890843937,-3.36441248683389));
#66404=CARTESIAN_POINT('Ctrl Pts',(-0.674181113544814,0.204229680901535,
-3.3485258883395));
#66405=CARTESIAN_POINT('Ctrl Pts',(-0.698697418738935,-0.260960913069297,
-3.32734375701365));
#66406=CARTESIAN_POINT('Ctrl Pts',(-0.28857304180409,-0.746461769625146,
-3.30086609285632));
#66407=CARTESIAN_POINT('Ctrl Pts',(0.473430607192205,-0.645985057580972,
-3.26909289586753));
#66408=CARTESIAN_POINT('Ctrl Pts',(0.742660672680755,-0.0686596397537776,
-3.24261523171021));
#66409=CARTESIAN_POINT('Ctrl Pts',(0.597361558428951,0.372009699145598,
-3.22143310038435));
#66410=CARTESIAN_POINT('Ctrl Pts',(0.264109646042611,0.698149366165507,
-3.2002509690585));
#66411=CARTESIAN_POINT('Ctrl Pts',(-0.242625816165684,0.705706516892486,
-3.17906883773263));
#66412=CARTESIAN_POINT('Ctrl Pts',(-0.586733693445035,0.38983774644249,
-3.15788670640678));
#66413=CARTESIAN_POINT('Ctrl Pts',(-0.703165961016561,0.0625732019186072,
-3.14200010791238));
#66414=CARTESIAN_POINT('Ctrl Pts',(-0.646063232064753,-0.280770790139778,
-3.12611350941799));
#66415=CARTESIAN_POINT('Ctrl Pts',(-0.363607076602154,-0.651205478284122,
-3.10493137809214));
#66416=CARTESIAN_POINT('Ctrl Pts',(0.263276112884758,-0.755754763367232,
-3.0784537139348));
#66417=CARTESIAN_POINT('Ctrl Pts',(0.779024453182575,-0.18588742772943,
-3.04668051694603));
#66418=CARTESIAN_POINT('Ctrl Pts',(0.610496128531625,0.428431439002367,
-3.0202028527887));
#66419=CARTESIAN_POINT('Ctrl Pts',(0.214482113777081,0.670245828496365,
-2.99902072146284));
#66420=CARTESIAN_POINT('Ctrl Pts',(-0.250646737033531,0.703095054615309,
-2.97783859013698));
#66421=CARTESIAN_POINT('Ctrl Pts',(-0.64176799247962,0.380818616250913,
-2.95665645881112));
#66422=CARTESIAN_POINT('Ctrl Pts',(-0.699565442495169,-0.0826927278637582,
-2.93547432748527));
#66423=CARTESIAN_POINT('Ctrl Pts',(-0.576453551727282,-0.407503468735792,
-2.91958772899087));
#66424=CARTESIAN_POINT('Ctrl Pts',(-0.310665810973606,-0.632231516387613,
-2.90370113049648));
#66425=CARTESIAN_POINT('Ctrl Pts',(0.144421469649071,-0.731724757136735,
-2.88251899917062));
#66426=CARTESIAN_POINT('Ctrl Pts',(0.689906312612689,-0.405596910472863,
-2.85604133501329));
#66427=CARTESIAN_POINT('Ctrl Pts',(0.714099960658798,0.362621677001496,
-2.82426813802451));
#66428=CARTESIAN_POINT('Ctrl Pts',(0.187968412483645,0.721752656237666,
-2.79779047386719));
#66429=CARTESIAN_POINT('Ctrl Pts',(-0.270408963645806,0.649700731204041,
-2.77660834254133));
#66430=CARTESIAN_POINT('Ctrl Pts',(-0.646190928271226,0.373635821128039,
-2.75542621121547));
#66431=CARTESIAN_POINT('Ctrl Pts',(-0.735673524021166,-0.125193612891662,
-2.73424407988961));
#66432=CARTESIAN_POINT('Ctrl Pts',(-0.479671017962049,-0.51589302195539,
-2.71306194856376));
#66433=CARTESIAN_POINT('Ctrl Pts',(-0.17556924533772,-0.683764004918535,
-2.69717535006935));
#66434=CARTESIAN_POINT('Ctrl Pts',(0.172489975910581,-0.682991321051767,
-2.68128875157497));
#66435=CARTESIAN_POINT('Ctrl Pts',(0.583760512301853,-0.464222301682604,
-2.6601066202491));
#66436=CARTESIAN_POINT('Ctrl Pts',(0.78840439834167,0.137470282764965,-2.63362895609179));
#66437=CARTESIAN_POINT('Ctrl Pts',(0.309536410753203,0.738661251767208,
-2.601855759103));
#66438=CARTESIAN_POINT('Ctrl Pts',(-0.323960533014889,0.671795053514425,
-2.57537809494567));
#66439=CARTESIAN_POINT('Ctrl Pts',(-0.626688571274547,0.320146032898944,
-2.55419596361981));
#66440=CARTESIAN_POINT('Ctrl Pts',(-0.734394845236606,-0.133531471571163,
-2.53301383229396));
#66441=CARTESIAN_POINT('Ctrl Pts',(-0.47967921519751,-0.571661460273545,
-2.51183170096809));
#66442=CARTESIAN_POINT('Ctrl Pts',(-0.0316362470218281,-0.703725119240024,
-2.49064956964224));
#66443=CARTESIAN_POINT('Ctrl Pts',(0.308819018868513,-0.634813821459323,
-2.47476297114784));
#66444=CARTESIAN_POINT('Ctrl Pts',(0.573606362075548,-0.408907908713105,
-2.45887637265346));
#66445=CARTESIAN_POINT('Ctrl Pts',(0.745452333195922,0.0240728069648603,
-2.43769424132759));
#66446=CARTESIAN_POINT('Ctrl Pts',(0.511922871354516,0.615154084561029,
-2.41121657717027));
#66447=CARTESIAN_POINT('Ctrl Pts',(-0.242248341456588,0.763379967975192,
-2.37944338018148));
#66448=CARTESIAN_POINT('Ctrl Pts',(-0.681807898729322,0.302319384274405,
-2.35296571602416));
#66449=CARTESIAN_POINT('Ctrl Pts',(-0.684903583824367,-0.161675998873061,
-2.3317835846983));
#66450=CARTESIAN_POINT('Ctrl Pts',(-0.473307084952599,-0.57718874377774,
-2.31060145337244));
#66451=CARTESIAN_POINT('Ctrl Pts',(0.0044593387890197,-0.746236617268379,
-2.28941932204658));
#66452=CARTESIAN_POINT('Ctrl Pts',(0.431445304074627,-0.5568526242795,-2.26823719072073));
#66453=CARTESIAN_POINT('Ctrl Pts',(0.646327285527458,-0.283934524694336,
-2.25235059222633));
#66454=CARTESIAN_POINT('Ctrl Pts',(0.701905026833796,0.0596596155461771,
-2.23646399373194));
#66455=CARTESIAN_POINT('Ctrl Pts',(0.552593332470904,0.500918446467205,
-2.21528186240608));
#66456=CARTESIAN_POINT('Ctrl Pts',(-0.00803857589287147,0.800259305016558,
-2.18880419824876));
#66457=CARTESIAN_POINT('Ctrl Pts',(-0.678815333020211,0.42502115018071,
-2.15703100125997));
#66458=CARTESIAN_POINT('Ctrl Pts',(-0.715374904833764,-0.210944936919148,
-2.13055333710265));
#66459=CARTESIAN_POINT('Ctrl Pts',(-0.417365872073619,-0.566601956028473,
-2.10937120577679));
#66460=CARTESIAN_POINT('Ctrl Pts',(0.0128942183109048,-0.74632444804134,
-2.08818907445093));
#66461=CARTESIAN_POINT('Ctrl Pts',(0.486476949341432,-0.565887932734067,
-2.06700694312507));
#66462=CARTESIAN_POINT('Ctrl Pts',(0.689323544065248,-0.145130793329111,
-2.04582481179921));
#66463=CARTESIAN_POINT('Ctrl Pts',(0.676430423898524,0.201989247127572,
-2.02993821330482));
#66464=CARTESIAN_POINT('Ctrl Pts',(0.496364768725477,0.499851930865303,
-2.01405161481042));
#66465=CARTESIAN_POINT('Ctrl Pts',(0.0969107931718748,0.739518072307371,
-1.99286948348457));
#66466=CARTESIAN_POINT('Ctrl Pts',(-0.524176728798627,0.604746501398676,
-1.96639181932724));
#66467=CARTESIAN_POINT('Ctrl Pts',(-0.792525284190483,-0.115485533133239,
-1.93461862233846));
#66468=CARTESIAN_POINT('Ctrl Pts',(-0.408696466689488,-0.62387997162377,
-1.90814095818113));
#66469=CARTESIAN_POINT('Ctrl Pts',(0.0486787143220458,-0.702041615945249,
-1.88695882685528));
#66470=CARTESIAN_POINT('Ctrl Pts',(0.492962794513711,-0.560494536846958,
-1.86577669552942));
#66471=CARTESIAN_POINT('Ctrl Pts',(0.737117187516088,-0.116392553554602,
-1.84459456420356));
#66472=CARTESIAN_POINT('Ctrl Pts',(0.619346845481977,0.335617908590315,
-1.8234124328777));
#66473=CARTESIAN_POINT('Ctrl Pts',(0.384810828458858,0.591843223017294,
-1.80752583438331));
#66474=CARTESIAN_POINT('Ctrl Pts',(0.0547443097277555,0.702305486931504,
-1.79163923588892));
#66475=CARTESIAN_POINT('Ctrl Pts',(-0.404864299349843,0.626389320003439,
-1.77045710456306));
#66476=CARTESIAN_POINT('Ctrl Pts',(-0.791006801773371,0.121605154151588,
-1.74397944040573));
#66477=CARTESIAN_POINT('Ctrl Pts',(-0.529295653645387,-0.601065175730866,
-1.71220624341695));
#66478=CARTESIAN_POINT('Ctrl Pts',(0.0923655176653327,-0.740086232829771,
-1.68572857925962));
#66479=CARTESIAN_POINT('Ctrl Pts',(0.491570810089264,-0.5035773887053,-1.66454644793377));
#66480=CARTESIAN_POINT('Ctrl Pts',(0.738569211247283,-0.10808312915354,
-1.64336431660791));
#66481=CARTESIAN_POINT('Ctrl Pts',(0.637170952451161,0.388461261913037,
-1.62218218528205));
#66482=CARTESIAN_POINT('Ctrl Pts',(0.254797411454479,0.656740568787333,
-1.60100005395619));
#66483=CARTESIAN_POINT('Ctrl Pts',(-0.0898318649340317,0.700205691474415,
-1.5851134554618));
#66484=CARTESIAN_POINT('Ctrl Pts',(-0.412913548481974,0.570729653953337,
-1.56922685696741));
#66485=CARTESIAN_POINT('Ctrl Pts',(-0.714078494834342,0.215338302021576,
-1.54804472564154));
#66486=CARTESIAN_POINT('Ctrl Pts',(-0.68161951116076,-0.419373837969105,
-1.52156706148423));
#66487=CARTESIAN_POINT('Ctrl Pts',(-0.0143232884913037,-0.800767180802928,
-1.48979386449544));
#66488=CARTESIAN_POINT('Ctrl Pts',(0.549496765312817,-0.504293888311659,
-1.46331620033811));
#66489=CARTESIAN_POINT('Ctrl Pts',(0.700662799746577,-0.0656025060371282,
-1.44213406901226));
#66490=CARTESIAN_POINT('Ctrl Pts',(0.632898545584985,0.395734599961226,
-1.4209519376864));
#66491=CARTESIAN_POINT('Ctrl Pts',(0.234174509286621,0.708555766228003,
-1.39976980636054));
#66492=CARTESIAN_POINT('Ctrl Pts',(-0.230938351402798,0.665505351914144,
-1.37858767503468));
#66493=CARTESIAN_POINT('Ctrl Pts',(-0.521748873394984,0.475537472174135,
-1.36270107654029));
#66494=CARTESIAN_POINT('Ctrl Pts',(-0.684182138924209,0.167704314788749,
-1.34681447804589));
#66495=CARTESIAN_POINT('Ctrl Pts',(-0.683663842477407,-0.298131567586256,
-1.32563234672004));
#66496=CARTESIAN_POINT('Ctrl Pts',(-0.248041461525952,-0.760890929984079,
-1.29915468256271));
#66497=CARTESIAN_POINT('Ctrl Pts',(0.507461495749466,-0.619609606749274,
-1.26738148557393));
#66498=CARTESIAN_POINT('Ctrl Pts',(0.74527725860231,-0.0286501079923499,
-1.2409038214166));
#66499=CARTESIAN_POINT('Ctrl Pts',(0.576506692556375,0.403574133443626,
-1.21972169009074));
#66500=CARTESIAN_POINT('Ctrl Pts',(0.226209707001196,0.711333684755956,
-1.19853955876488));
#66501=CARTESIAN_POINT('Ctrl Pts',(-0.280199631649522,0.691648133864366,
-1.17735742743902));
#66502=CARTESIAN_POINT('Ctrl Pts',(-0.606835592617558,0.35774356613014,
-1.15617529611317));
#66503=CARTESIAN_POINT('Ctrl Pts',(-0.70551253454806,0.0246948967655601,
-1.14028869761877));
#66504=CARTESIAN_POINT('Ctrl Pts',(-0.630041137511382,-0.315084276765811,
-1.12440209912438));
#66505=CARTESIAN_POINT('Ctrl Pts',(-0.328086109575231,-0.669804587776323,
-1.10321996779852));
#66506=CARTESIAN_POINT('Ctrl Pts',(0.303509663064016,-0.740514320182075,
-1.0767423036412));
#66507=CARTESIAN_POINT('Ctrl Pts',(0.787888271911223,-0.143754323166431,
-1.04496910665241));
#66508=CARTESIAN_POINT('Ctrl Pts',(0.586590198965058,0.460620189913425,
-1.01849144249509));
#66509=CARTESIAN_POINT('Ctrl Pts',(0.178153413511559,0.680803502488938,
-0.99730931116923));
#66510=CARTESIAN_POINT('Ctrl Pts',(-0.288068623095297,0.688609403797382,
-0.976127179843373));
#66511=CARTESIAN_POINT('Ctrl Pts',(-0.661305681260653,0.345779945321747,
-0.954945048517514));
#66512=CARTESIAN_POINT('Ctrl Pts',(-0.694110680048501,-0.120167630490676,
-0.933762917191655));
#66513=CARTESIAN_POINT('Ctrl Pts',(-0.553721475905218,-0.437893025123882,
-0.917876318697262));
#66514=CARTESIAN_POINT('Ctrl Pts',(-0.276240998940245,-0.648012999040435,
-0.901989720202866));
#66515=CARTESIAN_POINT('Ctrl Pts',(0.18353540309995,-0.722906243515896,
-0.880807588877012));
#66516=CARTESIAN_POINT('Ctrl Pts',(0.710706017243741,-0.367935498444747,
-0.854329924719684));
#66517=CARTESIAN_POINT('Ctrl Pts',(0.693580914570762,0.4004731568877,-0.8225567277309));
#66518=CARTESIAN_POINT('Ctrl Pts',(0.148910066612057,0.730811065154998,
-0.796079063573575));
#66519=CARTESIAN_POINT('Ctrl Pts',(-0.304932901189276,0.634230221210176,
-0.774896932247717));
#66520=CARTESIAN_POINT('Ctrl Pts',(-0.665336225024664,0.338369842529393,
-0.75371480092186));
#66521=CARTESIAN_POINT('Ctrl Pts',(-0.727882602416646,-0.164547536335721,
-0.732532669595999));
#66522=CARTESIAN_POINT('Ctrl Pts',(-0.451253979159214,-0.540924894803379,
-0.711350538270144));
#66523=CARTESIAN_POINT('Ctrl Pts',(-0.138570312837484,-0.69221098153884,
-0.695463939775748));
#66524=CARTESIAN_POINT('Ctrl Pts',(0.208944432324475,-0.672734836372497,
-0.679577341281356));
#66525=CARTESIAN_POINT('Ctrl Pts',(0.607864107453516,-0.432180412746452,
-0.658395209955497));
#66526=CARTESIAN_POINT('Ctrl Pts',(0.77987753494969,0.179640205882728,-0.631917545798173));
#66527=CARTESIAN_POINT('Ctrl Pts',(0.269393736650696,0.754228245212569,
-0.600144348809387));
#66528=CARTESIAN_POINT('Ctrl Pts',(-0.359594431187155,0.653414779307557,
-0.573666684652064));
#66529=CARTESIAN_POINT('Ctrl Pts',(-0.642987523708695,0.28600539159311,
-0.552484553326205));
#66530=CARTESIAN_POINT('Ctrl Pts',(-0.726157707116663,-0.172804615259813,
-0.531302422000348));
#66531=CARTESIAN_POINT('Ctrl Pts',(-0.448265169876774,-0.596613218990799,
-0.510120290674488));
#66532=CARTESIAN_POINT('Ctrl Pts',(0.00622737937602623,-0.704408304798551,
-0.488938159348631));
#66533=CARTESIAN_POINT('Ctrl Pts',(0.342487484376452,-0.61730076227034,
-0.473051560854236));
#66534=CARTESIAN_POINT('Ctrl Pts',(0.594751965918543,-0.377491481115471,
-0.457164962359842));
#66535=CARTESIAN_POINT('Ctrl Pts',(0.743081667418538,0.0640980403615866,
-0.435982831033984));
#66536=CARTESIAN_POINT('Ctrl Pts',(0.478124579859611,0.641776390658052,
-0.409505166876661));
#66537=CARTESIAN_POINT('Ctrl Pts',(-0.282921364094237,0.749257370810349,
-0.377731969887874));
#66538=CARTESIAN_POINT('Ctrl Pts',(-0.697070363894654,0.265244362057293,
-0.351254305730551));
#66539=CARTESIAN_POINT('Ctrl Pts',(-0.675223937332315,-0.198251437163076,
-0.330072174404692));
#66540=CARTESIAN_POINT('Ctrl Pts',(-0.441609192873322,-0.601783375902012,
-0.308890043078835));
#66541=CARTESIAN_POINT('Ctrl Pts',(0.0445634358699717,-0.744932214423158,
-0.287707911752975));
#66542=CARTESIAN_POINT('Ctrl Pts',(0.460736965378437,-0.532845482801779,
-0.266525780427117));
#66543=CARTESIAN_POINT('Ctrl Pts',(0.660672578510412,-0.248825721585754,
-0.250639181932725));
#66544=CARTESIAN_POINT('Ctrl Pts',(0.697646902447653,0.0973571564825142,
-0.234752583438329));
#66545=CARTESIAN_POINT('Ctrl Pts',(0.524957262296379,0.529753299715826,
-0.213570452112473));
#66546=CARTESIAN_POINT('Ctrl Pts',(-0.0512014684653643,0.798955362640304,
-0.187092787955149));
#66547=CARTESIAN_POINT('Ctrl Pts',(-0.700379789122524,0.387430595988897,
-0.155319590966363));
#66548=CARTESIAN_POINT('Ctrl Pts',(-0.703501109104381,-0.248248768190496,
-0.128841926809038));
#66549=CARTESIAN_POINT('Ctrl Pts',(-0.385645525478233,-0.58933640490133,
-0.107659795483182));
#66550=CARTESIAN_POINT('Ctrl Pts',(-0.0580733210265062,-0.703415543027182,
-0.0917731969887855));
#66551=CARTESIAN_POINT('Ctrl Pts',(0.286592368567594,-0.644628272737791,
-0.0758865984943943));
#66552=CARTESIAN_POINT('Ctrl Pts',(0.468570466391673,-0.501037465313089,
-0.065295532831463));
#66553=CARTESIAN_POINT('Ctrl Pts',(0.537060862935828,-0.411689834101626,
-0.0599999999999987));
#66554=CARTESIAN_POINT('Ctrl Pts',(-0.309090610374417,0.644553868208713,
-11.9529325805302));
#66555=CARTESIAN_POINT('Ctrl Pts',(-0.416321215482797,0.593132296143871,
-11.9476370476987));
#66556=CARTESIAN_POINT('Ctrl Pts',(-0.604253502485025,0.436152983457259,
-11.9370459820358));
#66557=CARTESIAN_POINT('Ctrl Pts',(-0.739811829461958,0.0925825907650836,
-11.9211593835414));
#66558=CARTESIAN_POINT('Ctrl Pts',(-0.692947007893374,-0.270822984187043,
-11.905272785047));
#66559=CARTESIAN_POINT('Ctrl Pts',(-0.409285919167933,-0.673437402061984,
-11.8840906537212));
#66560=CARTESIAN_POINT('Ctrl Pts',(0.248575292524515,-0.80813422424943,
-11.8576129895638));
#66561=CARTESIAN_POINT('Ctrl Pts',(0.814874281174704,-0.226283406359347,
-11.8258397925751));
#66562=CARTESIAN_POINT('Ctrl Pts',(0.661574797042729,0.427775327210025,
-11.7993621284177));
#66563=CARTESIAN_POINT('Ctrl Pts',(0.252019553201191,0.700124195300235,
-11.7781799970919));
#66564=CARTESIAN_POINT('Ctrl Pts',(-0.113896804202068,0.737010561893185,
-11.7622933985975));
#66565=CARTESIAN_POINT('Ctrl Pts',(-0.450904916615657,0.591935197672468,
-11.7464068001031));
#66566=CARTESIAN_POINT('Ctrl Pts',(-0.760463823480222,0.207699378513882,
-11.7252246687772));
#66567=CARTESIAN_POINT('Ctrl Pts',(-0.717957522306204,-0.32597923867788,
-11.7040425374514));
#66568=CARTESIAN_POINT('Ctrl Pts',(-0.351461896485877,-0.655051583268549,
-11.6828604061255));
#66569=CARTESIAN_POINT('Ctrl Pts',(0.122973627023043,-0.778202022613627,
-11.6616782747997));
#66570=CARTESIAN_POINT('Ctrl Pts',(0.71321863385788,-0.455059229729923,
-11.6352006106423));
#66571=CARTESIAN_POINT('Ctrl Pts',(0.767226239823105,0.355052608587047,
-11.6034274136535));
#66572=CARTESIAN_POINT('Ctrl Pts',(0.227493311469381,0.75431223879576,-11.5769497494962));
#66573=CARTESIAN_POINT('Ctrl Pts',(-0.261218076357254,0.696776585846632,
-11.5557676181703));
#66574=CARTESIAN_POINT('Ctrl Pts',(-0.563873923467153,0.488009727699941,
-11.539881019676));
#66575=CARTESIAN_POINT('Ctrl Pts',(-0.726886814028964,0.159273941491993,
-11.5239944211816));
#66576=CARTESIAN_POINT('Ctrl Pts',(-0.714056613740822,-0.333982155042871,
-11.5028122898557));
#66577=CARTESIAN_POINT('Ctrl Pts',(-0.336205356107924,-0.713229621096794,
-11.4816301585299));
#66578=CARTESIAN_POINT('Ctrl Pts',(0.156171374865428,-0.726794128759501,
-11.460448027204));
#66579=CARTESIAN_POINT('Ctrl Pts',(0.59749794928794,-0.513531071236394,
-11.4392658958781));
#66580=CARTESIAN_POINT('Ctrl Pts',(0.838193809590663,0.114861792295151,
-11.4127882317208));
#66581=CARTESIAN_POINT('Ctrl Pts',(0.35492781363207,0.767283632994828,-11.381015034732));
#66582=CARTESIAN_POINT('Ctrl Pts',(-0.314912149164092,0.722198192887193,
-11.3545373705747));
#66583=CARTESIAN_POINT('Ctrl Pts',(-0.650158212070062,0.361976566873907,
-11.3333552392488));
#66584=CARTESIAN_POINT('Ctrl Pts',(-0.745693705839447,0.00693137846112073,
-11.3174686407545));
#66585=CARTESIAN_POINT('Ctrl Pts',(-0.657132874094063,-0.3491548029949,
-11.30158204226));
#66586=CARTESIAN_POINT('Ctrl Pts',(-0.328043197231767,-0.71680441185038,
-11.2803999109342));
#66587=CARTESIAN_POINT('Ctrl Pts',(0.205458269395073,-0.761260418319186,
-11.2592177796083));
#66588=CARTESIAN_POINT('Ctrl Pts',(0.589524335340204,-0.452857892678056,
-11.2380356482825));
#66589=CARTESIAN_POINT('Ctrl Pts',(0.787843027379244,-0.00461692103046995,
-11.2168535169566));
#66590=CARTESIAN_POINT('Ctrl Pts',(0.564507567765378,0.630153396638974,
-11.1903758527993));
#66591=CARTESIAN_POINT('Ctrl Pts',(-0.226180200780229,0.814579918793154,
-11.1586026558105));
#66592=CARTESIAN_POINT('Ctrl Pts',(-0.70753989713274,0.34659368739482,-11.1321249916532));
#66593=CARTESIAN_POINT('Ctrl Pts',(-0.729871026448289,-0.144986278853025,
-11.1109428603273));
#66594=CARTESIAN_POINT('Ctrl Pts',(-0.572847938806445,-0.477443594241456,
-11.0950562618329));
#66595=CARTESIAN_POINT('Ctrl Pts',(-0.274834434169087,-0.691519142555255,
-11.0791696633386));
#66596=CARTESIAN_POINT('Ctrl Pts',(0.213993560575424,-0.758701298387166,
-11.0579875320127));
#66597=CARTESIAN_POINT('Ctrl Pts',(0.649402182312231,-0.447221791185339,
-11.0368054006868));
#66598=CARTESIAN_POINT('Ctrl Pts',(0.742488688495841,0.0364658799499072,
-11.015623269361));
#66599=CARTESIAN_POINT('Ctrl Pts',(0.603475495194033,0.506493117855511,
-10.9944411380351));
#66600=CARTESIAN_POINT('Ctrl Pts',(0.0223311557836704,0.845732473564332,
-10.9679634738778));
#66601=CARTESIAN_POINT('Ctrl Pts',(-0.699712755981378,0.474447032290606,
-10.936190276889));
#66602=CARTESIAN_POINT('Ctrl Pts',(-0.763648675099599,-0.193857141194035,
-10.9097126127317));
#66603=CARTESIAN_POINT('Ctrl Pts',(-0.462443774570201,-0.582990987637431,
-10.8885304814058));
#66604=CARTESIAN_POINT('Ctrl Pts',(-0.127545170575338,-0.734737624012674,
-10.8726438829114));
#66605=CARTESIAN_POINT('Ctrl Pts',(0.23818031069733,-0.704984276648341,
-10.856757284417));
#66606=CARTESIAN_POINT('Ctrl Pts',(0.654251050420993,-0.439745912050845,
-10.8355751530912));
#66607=CARTESIAN_POINT('Ctrl Pts',(0.784478489585921,0.0795237340656153,
-10.8143930217653));
#66608=CARTESIAN_POINT('Ctrl Pts',(0.54231178387317,0.508445810305424,-10.7932108904395));
#66609=CARTESIAN_POINT('Ctrl Pts',(0.132083933285029,0.776705726966545,
-10.7720287591136));
#66610=CARTESIAN_POINT('Ctrl Pts',(-0.530466364057635,0.659065652240602,
-10.7455510949563));
#66611=CARTESIAN_POINT('Ctrl Pts',(-0.84044907259622,-0.0913415770861792,
-10.7137778979675));
#66612=CARTESIAN_POINT('Ctrl Pts',(-0.456552117021781,-0.642105952796128,
-10.6873002338102));
#66613=CARTESIAN_POINT('Ctrl Pts',(0.0249302303405187,-0.743714474728285,
-10.6661181024843));
#66614=CARTESIAN_POINT('Ctrl Pts',(0.378420423442174,-0.642576944652335,
-10.6502315039899));
#66615=CARTESIAN_POINT('Ctrl Pts',(0.637912125065641,-0.383145940105722,
-10.6343449054955));
#66616=CARTESIAN_POINT('Ctrl Pts',(0.78333472385694,0.0883607070047231,
-10.6131627741697));
#66617=CARTESIAN_POINT('Ctrl Pts',(0.546442418456161,0.568446310758132,
-10.5919806428438));
#66618=CARTESIAN_POINT('Ctrl Pts',(0.0842014340339106,0.738599574499925,
-10.5707985115179));
#66619=CARTESIAN_POINT('Ctrl Pts',(-0.402129173320327,0.677502826340514,
-10.5496163801921));
#66620=CARTESIAN_POINT('Ctrl Pts',(-0.83096433791511,0.158935101450751,
-10.5231387160348));
#66621=CARTESIAN_POINT('Ctrl Pts',(-0.581452373499001,-0.613686454702083,
-10.491365519046));
#66622=CARTESIAN_POINT('Ctrl Pts',(0.0676890135440266,-0.784957379491861,
-10.4648878548887));
#66623=CARTESIAN_POINT('Ctrl Pts',(0.500446959800122,-0.550713697607039,
-10.4437057235628));
#66624=CARTESIAN_POINT('Ctrl Pts',(0.704402313506879,-0.244794868007973,
-10.4278191250684));
#66625=CARTESIAN_POINT('Ctrl Pts',(0.734241216025536,0.120923642909903,
-10.411932526574));
#66626=CARTESIAN_POINT('Ctrl Pts',(0.539850014877955,0.574441350860708,
-10.3907503952481));
#66627=CARTESIAN_POINT('Ctrl Pts',(0.048508296433538,0.787005381226751,
-10.3695682639223));
#66628=CARTESIAN_POINT('Ctrl Pts',(-0.413956664385384,0.617461814977869,
-10.3483861325964));
#66629=CARTESIAN_POINT('Ctrl Pts',(-0.745082259064963,0.256067137605208,
-10.3272040012706));
#66630=CARTESIAN_POINT('Ctrl Pts',(-0.736240410083894,-0.416787902798724,
-10.3007263371133));
#66631=CARTESIAN_POINT('Ctrl Pts',(-0.0459062458519896,-0.844150782694781,
-10.2689531401245));
#66632=CARTESIAN_POINT('Ctrl Pts',(0.559736006003475,-0.554468658948882,
-10.2424754759671));
#66633=CARTESIAN_POINT('Ctrl Pts',(0.737941923316341,-0.0957833707768819,
-10.2212933446413));
#66634=CARTESIAN_POINT('Ctrl Pts',(0.695357525294872,0.269416144083229,
-10.2054067461469));
#66635=CARTESIAN_POINT('Ctrl Pts',(0.481351698610594,0.567479720316027,
-10.1895201476525));
#66636=CARTESIAN_POINT('Ctrl Pts',(0.0396027232325981,0.787307137307268,
-10.1683380163266));
#66637=CARTESIAN_POINT('Ctrl Pts',(-0.4724972623396,0.631250237215267,-10.1471558850008));
#66638=CARTESIAN_POINT('Ctrl Pts',(-0.715229369954264,0.20264787514224,
-10.1259737536749));
#66639=CARTESIAN_POINT('Ctrl Pts',(-0.733660537244455,-0.287158785038608,
-10.1047916223491));
#66640=CARTESIAN_POINT('Ctrl Pts',(-0.291347020463876,-0.794278925206177,
-10.0783139581917));
#66641=CARTESIAN_POINT('Ctrl Pts',(0.511473735496293,-0.673121493662104,
-10.046540761203));
#66642=CARTESIAN_POINT('Ctrl Pts',(0.785562273165169,-0.0602644601142881,
-10.0200630970456));
#66643=CARTESIAN_POINT('Ctrl Pts',(0.624458154098192,0.404703286477242,
-9.99888096571979));
#66644=CARTESIAN_POINT('Ctrl Pts',(0.355587926208178,0.655487889599687,
-9.98299436722537));
#66645=CARTESIAN_POINT('Ctrl Pts',(-0.000477527797489372,0.744132019666176,
-9.96710776873098));
#66646=CARTESIAN_POINT('Ctrl Pts',(-0.479480350977519,0.625715188539386,
-9.94592563740513));
#66647=CARTESIAN_POINT('Ctrl Pts',(-0.768774444642223,0.175260886017933,
-9.92474350607927));
#66648=CARTESIAN_POINT('Ctrl Pts',(-0.676325850336198,-0.308549116206573,
-9.90356137475341));
#66649=CARTESIAN_POINT('Ctrl Pts',(-0.373296388542898,-0.693806715184786,
-9.88237924342755));
#66650=CARTESIAN_POINT('Ctrl Pts',(0.292116363348639,-0.793996302021506,
-9.85590157927023));
#66651=CARTESIAN_POINT('Ctrl Pts',(0.825587413847927,-0.181943258815281,
-9.82412838228143));
#66652=CARTESIAN_POINT('Ctrl Pts',(0.637760694546856,0.462602622846441,
-9.79765071812413));
#66653=CARTESIAN_POINT('Ctrl Pts',(0.213970617176942,0.712705627373687,
-9.77646858679825));
#66654=CARTESIAN_POINT('Ctrl Pts',(-0.153305821775376,0.729797555275886,
-9.76058198830387));
#66655=CARTESIAN_POINT('Ctrl Pts',(-0.482079633214187,0.566861462762583,
-9.74469538980946));
#66656=CARTESIAN_POINT('Ctrl Pts',(-0.770513763500401,0.166521603399833,
-9.72351325848364));
#66657=CARTESIAN_POINT('Ctrl Pts',(-0.699408380757533,-0.364085761639854,
-9.70233112715773));
#66658=CARTESIAN_POINT('Ctrl Pts',(-0.315749334014388,-0.672994480671505,
-9.68114899583192));
#66659=CARTESIAN_POINT('Ctrl Pts',(0.16461437899866,-0.770467428228838,
-9.65996686450602));
#66660=CARTESIAN_POINT('Ctrl Pts',(0.736643839361908,-0.416074454022362,
-9.63348920034873));
#66661=CARTESIAN_POINT('Ctrl Pts',(0.747036554356828,0.395770531731598,
-9.60171600335992));
#66662=CARTESIAN_POINT('Ctrl Pts',(0.186628415656226,0.765447401617473,
-9.5752383392026));
#66663=CARTESIAN_POINT('Ctrl Pts',(-0.298285275337462,0.68173208140886,
-9.55405620787676));
#66664=CARTESIAN_POINT('Ctrl Pts',(-0.589284505107621,0.457002099247858,
-9.53816960938235));
#66665=CARTESIAN_POINT('Ctrl Pts',(-0.734395810570078,0.119981182451158,
-9.52228301088797));
#66666=CARTESIAN_POINT('Ctrl Pts',(-0.69507667784042,-0.371872714869924,
-9.5011008795621));
#66667=CARTESIAN_POINT('Ctrl Pts',(-0.297390844736814,-0.730266533787131,
-9.47991874823625));
#66668=CARTESIAN_POINT('Ctrl Pts',(0.195003365029303,-0.717351309033507,
-9.45873661691039));
#66669=CARTESIAN_POINT('Ctrl Pts',(0.624231524365783,-0.480679680996236,
-9.43755448558453));
#66670=CARTESIAN_POINT('Ctrl Pts',(0.830809975211841,0.159740046476628,
-9.41107682142721));
#66671=CARTESIAN_POINT('Ctrl Pts',(0.313181388564641,0.785248588148464,
-9.37930362443842));
#66672=CARTESIAN_POINT('Ctrl Pts',(-0.353267765581714,0.704231336972586,
-9.35282596028109));
#66673=CARTESIAN_POINT('Ctrl Pts',(-0.668671212204437,0.326514235944241,
-9.33164382895525));
#66674=CARTESIAN_POINT('Ctrl Pts',(-0.744988654241857,-0.0331519490798406,
-9.31575723046083));
#66675=CARTESIAN_POINT('Ctrl Pts',(-0.637419851546266,-0.383964351965119,
-9.29987063196646));
#66676=CARTESIAN_POINT('Ctrl Pts',(-0.289048357513512,-0.733397539647596,
-9.27868850064058));
#66677=CARTESIAN_POINT('Ctrl Pts',(0.246071239309372,-0.749119129436365,
-9.25750636931473));
#66678=CARTESIAN_POINT('Ctrl Pts',(0.613008881978574,-0.42052267900818,
-9.23632423798887));
#66679=CARTESIAN_POINT('Ctrl Pts',(0.786952691293118,0.0377281513089534,
-9.21514210666303));
#66680=CARTESIAN_POINT('Ctrl Pts',(0.529827627109992,0.659579246877018,
-9.18866444250567));
#66681=CARTESIAN_POINT('Ctrl Pts',(-0.269628597927286,0.801247993140825,
-9.15689124551692));
#66682=CARTESIAN_POINT('Ctrl Pts',(-0.72514330893185,0.30806991363108,-9.13041358135957));
#66683=CARTESIAN_POINT('Ctrl Pts',(-0.721024838858224,-0.18399977732235,
-9.10923145003374));
#66684=CARTESIAN_POINT('Ctrl Pts',(-0.546362515984092,-0.507538321513182,
-9.09334485153932));
#66685=CARTESIAN_POINT('Ctrl Pts',(-0.237275303441589,-0.705289388196051,
-9.07745825304495));
#66686=CARTESIAN_POINT('Ctrl Pts',(0.254456670686461,-0.746105024031849,
-9.05627612171907));
#66687=CARTESIAN_POINT('Ctrl Pts',(0.672497322274279,-0.411676907825386,
-9.03509399039321));
#66688=CARTESIAN_POINT('Ctrl Pts',(0.73945611533713,0.0763142610221662,
-9.01391185906737));
#66689=CARTESIAN_POINT('Ctrl Pts',(0.575384704040563,0.538191781887113,
-8.99272972774149));
#66690=CARTESIAN_POINT('Ctrl Pts',(-0.023150471951528,0.845710442768847,
-8.96625206358419));
#66691=CARTESIAN_POINT('Ctrl Pts',(-0.724198270894036,0.436159135828339,
-8.93447886659538));
#66692=CARTESIAN_POINT('Ctrl Pts',(-0.75212737562495,-0.234615219047742,
-8.90800120243808));
#66693=CARTESIAN_POINT('Ctrl Pts',(-0.43044580886719,-0.607000116914215,
-8.88681907111221));
#66694=CARTESIAN_POINT('Ctrl Pts',(-0.0878763299167745,-0.740530146123197,
-8.87093247261782));
#66695=CARTESIAN_POINT('Ctrl Pts',(0.275721737088013,-0.691165837134929,
-8.85504587412342));
#66696=CARTESIAN_POINT('Ctrl Pts',(0.676937432624418,-0.403951255047272,
-8.83386374279756));
#66697=CARTESIAN_POINT('Ctrl Pts',(0.779071326801438,0.121566412543086,
-8.81268161147172));
#66698=CARTESIAN_POINT('Ctrl Pts',(0.514204438424602,0.536854736822985,
-8.79149948014584));
#66699=CARTESIAN_POINT('Ctrl Pts',(0.090153183279391,0.782681515866618,
-8.77031734882));
#66700=CARTESIAN_POINT('Ctrl Pts',(-0.565117781341099,0.629606218657323,
-8.74383968466265));
#66701=CARTESIAN_POINT('Ctrl Pts',(-0.834325944652335,-0.136375017552418,
-8.71206648767389));
#66702=CARTESIAN_POINT('Ctrl Pts',(-0.421385847917164,-0.665713044297937,
-8.68558882351655));
#66703=CARTESIAN_POINT('Ctrl Pts',(0.0648611539509664,-0.741300051944791,
-8.6644066921907));
#66704=CARTESIAN_POINT('Ctrl Pts',(0.412405452710403,-0.621312231693223,
-8.6485200936963));
#66705=CARTESIAN_POINT('Ctrl Pts',(0.657580455193039,-0.348311119078007,
-8.63263349520191));
#66706=CARTESIAN_POINT('Ctrl Pts',(0.777454318089235,0.130329150334099,
-8.61145136387606));
#66707=CARTESIAN_POINT('Ctrl Pts',(0.515104698860376,0.596990514258567,
-8.59026923255019));
#66708=CARTESIAN_POINT('Ctrl Pts',(0.0443876860470674,0.742057239215564,
-8.56908710122434));
#66709=CARTESIAN_POINT('Ctrl Pts',(-0.437956847320566,0.654913545149056,
-8.54790496989848));
#66710=CARTESIAN_POINT('Ctrl Pts',(-0.838304694233625,0.114049712782297,
-8.52142730574116));
#66711=CARTESIAN_POINT('Ctrl Pts',(-0.547632874814056,-0.644046707743566,
-8.48965410875236));
#66712=CARTESIAN_POINT('Ctrl Pts',(0.109774528782839,-0.780185518324841,
-8.46317644459505));
#66713=CARTESIAN_POINT('Ctrl Pts',(0.529318960625381,-0.523024066585532,
-8.44199431326918));
#66714=CARTESIAN_POINT('Ctrl Pts',(0.716539627251363,-0.206586808038074,
-8.4261077147748));
#66715=CARTESIAN_POINT('Ctrl Pts',(0.726681830826818,0.160206764749315,
-8.41022111628039));
#66716=CARTESIAN_POINT('Ctrl Pts',(0.508199650129457,0.602622618021181,
-8.38903898495455));
#66717=CARTESIAN_POINT('Ctrl Pts',(0.00614481505570648,0.788474962285219,
-8.36785685362867));
#66718=CARTESIAN_POINT('Ctrl Pts',(-0.446540665096658,0.594323689044844,
-8.34667472230284));
#66719=CARTESIAN_POINT('Ctrl Pts',(-0.757766557247427,0.215656663361126,
-8.32549259097696));
#66720=CARTESIAN_POINT('Ctrl Pts',(-0.712778497149809,-0.455750931277951,
-8.29901492681964));
#66721=CARTESIAN_POINT('Ctrl Pts',(-0.000475551173634113,-0.845397954328917,
-8.26724172983087));
#66722=CARTESIAN_POINT('Ctrl Pts',(0.588724123331353,-0.523587429930306,
-8.24076406567352));
#66723=CARTESIAN_POINT('Ctrl Pts',(0.742022947463043,-0.0559882286151282,
-8.21958193434769));
#66724=CARTESIAN_POINT('Ctrl Pts',(0.679874394168988,0.306395095963096,
-8.20369533585327));
#66725=CARTESIAN_POINT('Ctrl Pts',(0.450159980531817,0.592527368695197,
-8.18780873735889));
#66726=CARTESIAN_POINT('Ctrl Pts',(-0.00276410569037474,0.78829770002337,
-8.16662660603303));
#66727=CARTESIAN_POINT('Ctrl Pts',(-0.505737655653165,0.604946236088125,
-8.14544447470717));
#66728=CARTESIAN_POINT('Ctrl Pts',(-0.725086074171385,0.163918876239337,
-8.12426234338131));
#66729=CARTESIAN_POINT('Ctrl Pts',(-0.717168574417189,-0.326170488553287,
-8.10308021205545));
#66730=CARTESIAN_POINT('Ctrl Pts',(-0.248241755000774,-0.808788061505605,
-8.07660254789813));
#66731=CARTESIAN_POINT('Ctrl Pts',(0.546907953339569,-0.644662406152521,
-8.04482935090935));
#66732=CARTESIAN_POINT('Ctrl Pts',(0.787665711547366,-0.017961542970373,
-8.01835168675202));
#66733=CARTESIAN_POINT('Ctrl Pts',(0.601807191524753,0.437676639237566,
-7.99716955542616));
#66734=CARTESIAN_POINT('Ctrl Pts',(0.319848411758804,0.673649864671741,
-7.98128295693177));
#66735=CARTESIAN_POINT('Ctrl Pts',(-0.0404662247302287,0.743031072958151,
-7.96539635843737));
#66736=CARTESIAN_POINT('Ctrl Pts',(-0.512413202074689,0.599043916989371,
-7.94421422711151));
#66737=CARTESIAN_POINT('Ctrl Pts',(-0.777082008295114,0.133693968774884,
-7.92303209578568));
#66738=CARTESIAN_POINT('Ctrl Pts',(-0.658767228492401,-0.344448764853758,
-7.90184996445978));
#66739=CARTESIAN_POINT('Ctrl Pts',(-0.335472045139475,-0.712864965238586,
-7.88066783313396));
#66740=CARTESIAN_POINT('Ctrl Pts',(0.334363325358902,-0.777150734423377,
-7.8541901689766));
#66741=CARTESIAN_POINT('Ctrl Pts',(0.834171990018743,-0.137313576898307,
-7.82241697198784));
#66742=CARTESIAN_POINT('Ctrl Pts',(0.6119790200543,0.496207183731426,-7.7959393078305));
#66743=CARTESIAN_POINT('Ctrl Pts',(0.175360881720452,0.723174458528111,
-7.77475717650466));
#66744=CARTESIAN_POINT('Ctrl Pts',(-0.19230335003752,0.720504384609304,
-7.75887057801025));
#66745=CARTESIAN_POINT('Ctrl Pts',(-0.511845950255046,0.540135551443124,
-7.74298397951587));
#66746=CARTESIAN_POINT('Ctrl Pts',(-0.7783491679022,0.124873844212295,-7.72180184819));
#66747=CARTESIAN_POINT('Ctrl Pts',(-0.678831884888873,-0.401145605685725,
-7.70061971686414));
#66748=CARTESIAN_POINT('Ctrl Pts',(-0.279126589163162,-0.68899024678654,
-7.67943758553829));
#66749=CARTESIAN_POINT('Ctrl Pts',(0.205781150524281,-0.760507771047459,
-7.65825545421242));
#66750=CARTESIAN_POINT('Ctrl Pts',(0.757939066824373,-0.375886243884045,
-7.63177779005511));
#66751=CARTESIAN_POINT('Ctrl Pts',(0.724688506752804,0.435344111609228,
-7.60000459306631));
#66752=CARTESIAN_POINT('Ctrl Pts',(0.145223866217483,0.774370659861374,
-7.573526928909));
#66753=CARTESIAN_POINT('Ctrl Pts',(-0.334490284337073,0.664717222576117,
-7.55234479758313));
#66754=CARTESIAN_POINT('Ctrl Pts',(-0.612992106461524,0.424673785502175,
-7.53645819908875));
#66755=CARTESIAN_POINT('Ctrl Pts',(-0.73978234060737,0.0803416408267936,
-7.52057160059435));
#66756=CARTESIAN_POINT('Ctrl Pts',(-0.674087973298083,-0.408688522468257,
-7.49938946926849));
#66757=CARTESIAN_POINT('Ctrl Pts',(-0.257716848716532,-0.745192962118112,
-7.47820733794264));
#66758=CARTESIAN_POINT('Ctrl Pts',(0.233271782775553,-0.705835312452951,
-7.45702520661677));
#66759=CARTESIAN_POINT('Ctrl Pts',(0.649161051353326,-0.446439112467214,
-7.43584307529092));
#66760=CARTESIAN_POINT('Ctrl Pts',(0.821025066809404,0.204156648264201,
-7.40936541113359));
#66761=CARTESIAN_POINT('Ctrl Pts',(0.270529859099672,0.800944144536901,
-7.37759221414481));
#66762=CARTESIAN_POINT('Ctrl Pts',(-0.390602425763559,0.684229227058386,
-7.35111454998748));
#66763=CARTESIAN_POINT('Ctrl Pts',(-0.685251727478478,0.29010826650229,
-7.32993241866163));
#66764=CARTESIAN_POINT('Ctrl Pts',(-0.742130558038833,-0.073139466103157,
-7.31404582016723));
#66765=CARTESIAN_POINT('Ctrl Pts',(-0.615864661958205,-0.417664229826262,
-7.29815922167284));
#66766=CARTESIAN_POINT('Ctrl Pts',(-0.249218157413321,-0.747871121355755,
-7.27697709034698));
#66767=CARTESIAN_POINT('Ctrl Pts',(0.285973054269614,-0.734812858579961,
-7.25579495902112));
#66768=CARTESIAN_POINT('Ctrl Pts',(0.634721810251999,-0.386972139223568,
-7.23461282769526));
#66769=CARTESIAN_POINT('Ctrl Pts',(0.783788032819058,0.079964187886226,
-7.2134306963694));
#66770=CARTESIAN_POINT('Ctrl Pts',(0.493616465001244,0.687098888690364,
-7.18695303221208));
#66771=CARTESIAN_POINT('Ctrl Pts',(-0.312297758445966,0.785600431136631,
-7.15517983522329));
#66772=CARTESIAN_POINT('Ctrl Pts',(-0.740651029737173,0.268655806418843,
-7.12870217106597));
#66773=CARTESIAN_POINT('Ctrl Pts',(-0.710094862802953,-0.222481509627331,
-7.10752003974011));
#66774=CARTESIAN_POINT('Ctrl Pts',(-0.518298085273821,-0.536166244254872,
-7.09163344124572));
#66775=CARTESIAN_POINT('Ctrl Pts',(-0.199030438307018,-0.717021321407235,
-7.07574684275133));
#66776=CARTESIAN_POINT('Ctrl Pts',(0.294184391603376,-0.731352478548719,
-7.05456471142545));
#66777=CARTESIAN_POINT('Ctrl Pts',(0.693648920090533,-0.374942262968557,
-7.03338258009962));
#66778=CARTESIAN_POINT('Ctrl Pts',(0.734286486642884,0.115942091056241,
-7.01220044877374));
#66779=CARTESIAN_POINT('Ctrl Pts',(0.545631029801399,0.568335051754265,
-6.9910183174479));
#66780=CARTESIAN_POINT('Ctrl Pts',(-0.068565193966149,0.843244277499859,
-6.96454065329056));
#66781=CARTESIAN_POINT('Ctrl Pts',(-0.746590826006241,0.396610723324246,
-6.93276745630179));
#66782=CARTESIAN_POINT('Ctrl Pts',(-0.738432400203635,-0.274695250236871,
-6.90628979214445));
#66783=CARTESIAN_POINT('Ctrl Pts',(-0.397203838848781,-0.629254993392277,
-6.88510766081861));
#66784=CARTESIAN_POINT('Ctrl Pts',(-0.0479535234128937,-0.744182508709381,
-6.86922106232419));
#66785=CARTESIAN_POINT('Ctrl Pts',(0.312466317455657,-0.675349902777122,
-6.85333446382982));
#66786=CARTESIAN_POINT('Ctrl Pts',(0.697667440599412,-0.366989163968669,
-6.83215233250394));
#66787=CARTESIAN_POINT('Ctrl Pts',(0.771412619053169,0.16325775958901,-6.81097020117811));
#66788=CARTESIAN_POINT('Ctrl Pts',(0.484611023123308,0.56371213328692,-6.78978806985223));
#66789=CARTESIAN_POINT('Ctrl Pts',(0.047961887234688,0.786395326221602,
-6.76860593852638));
#66790=CARTESIAN_POINT('Ctrl Pts',(-0.598135987318,0.598327199810221,-6.74212827436906));
#66791=CARTESIAN_POINT('Ctrl Pts',(-0.825791583868712,-0.18101432918127,
-6.71035507738028));
#66792=CARTESIAN_POINT('Ctrl Pts',(-0.385001758097536,-0.687396200451901,
-6.68387741322294));
#66793=CARTESIAN_POINT('Ctrl Pts',(0.104604626396011,-0.736743244603411,
-6.6626952818971));
#66794=CARTESIAN_POINT('Ctrl Pts',(0.445198615026306,-0.598251903344638,
-6.64680868340269));
#66795=CARTESIAN_POINT('Ctrl Pts',(0.675348353348783,-0.312469666119661,
-6.63092208490831));
#66796=CARTESIAN_POINT('Ctrl Pts',(0.769327040856058,0.171920937806506,
-6.60973995358243));
#66797=CARTESIAN_POINT('Ctrl Pts',(0.482278307083611,0.623809392679397,
-6.5885578222566));
#66798=CARTESIAN_POINT('Ctrl Pts',(0.0044456566373652,0.743370331522448,
-6.56737569093072));
#66799=CARTESIAN_POINT('Ctrl Pts',(-0.472518811304924,0.630431538476766,
-6.54619355960487));
#66800=CARTESIAN_POINT('Ctrl Pts',(-0.843222315817966,0.0688347185687733,
-6.51971589544755));
#66801=CARTESIAN_POINT('Ctrl Pts',(-0.512230702407081,-0.672545646102564,
-6.48794269845875));
#66802=CARTESIAN_POINT('Ctrl Pts',(0.151542800970993,-0.77315888513845,
-6.46146503430144));
#66803=CARTESIAN_POINT('Ctrl Pts',(0.556661197052577,-0.493822886353796,
-6.44028290297557));
#66804=CARTESIAN_POINT('Ctrl Pts',(0.726606143350278,-0.16778168339867,
-6.42439630448119));
#66805=CARTESIAN_POINT('Ctrl Pts',(0.717022255325511,0.199026843686629,
-6.40850970598679));
#66806=CARTESIAN_POINT('Ctrl Pts',(0.475080690338507,0.629062373469418,
-6.38732757466093));
#66807=CARTESIAN_POINT('Ctrl Pts',(-0.036236656606484,0.78766564904173,
-6.36614544333508));
#66808=CARTESIAN_POINT('Ctrl Pts',(-0.477833876060214,0.56946814731603,
-6.34496331200921));
#66809=CARTESIAN_POINT('Ctrl Pts',(-0.768261515109739,0.174622461779635,
-6.32378118068336));
#66810=CARTESIAN_POINT('Ctrl Pts',(-0.687255280232435,-0.493395818705134,
-6.29730351652604));
#66811=CARTESIAN_POINT('Ctrl Pts',(0.0449541415847475,-0.844203664783362,
-6.26553031953724));
#66812=CARTESIAN_POINT('Ctrl Pts',(0.616014830444453,-0.491190016005719,
-6.23905265537993));
#66813=CARTESIAN_POINT('Ctrl Pts',(0.743953925476331,-0.0160354294836368,
-6.21787052405406));
#66814=CARTESIAN_POINT('Ctrl Pts',(0.662438556258499,0.342497609724965,
-6.20198392555968));
#66815=CARTESIAN_POINT('Ctrl Pts',(0.417644625691115,0.61584571232203,-6.18609732706527));
#66816=CARTESIAN_POINT('Ctrl Pts',(-0.0450712489042535,0.787048564929024,
-6.16491519573942));
#66817=CARTESIAN_POINT('Ctrl Pts',(-0.537615573110493,0.576820073921749,
-6.14373306441357));
#66818=CARTESIAN_POINT('Ctrl Pts',(-0.732731387322439,0.124802468022666,
-6.1225509330877));
#66819=CARTESIAN_POINT('Ctrl Pts',(-0.698874509772504,-0.364441229918025,
-6.10136880176184));
#66820=CARTESIAN_POINT('Ctrl Pts',(-0.203848075213461,-0.820532664836046,
-6.07489113760452));
#66821=CARTESIAN_POINT('Ctrl Pts',(0.579781559557804,-0.615081213840891,
-6.04311794061573));
#66822=CARTESIAN_POINT('Ctrl Pts',(0.830826746056493,0.153711188366667,
-6.01134474362695));
#66823=CARTESIAN_POINT('Ctrl Pts',(0.321082505138741,0.781540937050481,
-5.97957154663815));
#66824=CARTESIAN_POINT('Ctrl Pts',(-0.482882123813584,0.693755296141619,
-5.94779834964938));
#66825=CARTESIAN_POINT('Ctrl Pts',(-0.844907628832503,-0.0309675729080316,
-5.91602515266057));
#66826=CARTESIAN_POINT('Ctrl Pts',(-0.500217074565313,-0.609118928278575,
-5.88954748850327));
#66827=CARTESIAN_POINT('Ctrl Pts',(-0.0283586531132722,-0.742742706989181,
-5.86836535717739));
#66828=CARTESIAN_POINT('Ctrl Pts',(0.4540974835594,-0.644629643714152,-5.84718322585155));
#66829=CARTESIAN_POINT('Ctrl Pts',(0.761010378138235,-0.205767017280531,
-5.82600109452568));
#66830=CARTESIAN_POINT('Ctrl Pts',(0.688497809353763,0.282247659457379,
-5.80481896319983));
#66831=CARTESIAN_POINT('Ctrl Pts',(0.47125751192046,0.577966963540043,-5.78893236470543));
#66832=CARTESIAN_POINT('Ctrl Pts',(0.137111726801814,0.731385638773274,
-5.77304576621104));
#66833=CARTESIAN_POINT('Ctrl Pts',(-0.354190246329251,0.703769260877763,
-5.75186363488517));
#66834=CARTESIAN_POINT('Ctrl Pts',(-0.816970922862985,0.217391843627321,
-5.72538597072787));
#66835=CARTESIAN_POINT('Ctrl Pts',(-0.624035667222098,-0.571260658681954,
-5.69361277373906));
#66836=CARTESIAN_POINT('Ctrl Pts',(0.0131013734634179,-0.787748128382458,
-5.66713510958175));
#66837=CARTESIAN_POINT('Ctrl Pts',(0.459181237710636,-0.584612499740476,
-5.64595297825589));
#66838=CARTESIAN_POINT('Ctrl Pts',(0.763428896494617,-0.19724753473581,
-5.62477084693002));
#66839=CARTESIAN_POINT('Ctrl Pts',(0.713229822891815,0.335744473945888,
-5.60358871560418));
#66840=CARTESIAN_POINT('Ctrl Pts',(0.342056978743302,0.660855220477942,
-5.58240658427831));
#66841=CARTESIAN_POINT('Ctrl Pts',(-0.0149623003848158,0.745575824719156,
-5.56651998578392));
#66842=CARTESIAN_POINT('Ctrl Pts',(-0.368957988145881,0.646221892521559,
-5.55063338728953));
#66843=CARTESIAN_POINT('Ctrl Pts',(-0.725547995671562,0.307115594152496,
-5.52945125596367));
#66844=CARTESIAN_POINT('Ctrl Pts',(-0.763416454169478,-0.363171111300542,
-5.50297359180634));
#66845=CARTESIAN_POINT('Ctrl Pts',(-0.105827519704371,-0.839382289810237,
-5.47120039481756));
#66846=CARTESIAN_POINT('Ctrl Pts',(0.519936517239823,-0.591932403052683,
-5.44472273066023));
#66847=CARTESIAN_POINT('Ctrl Pts',(0.7284339930835,-0.148334525216346,-5.42354059933438));
#66848=CARTESIAN_POINT('Ctrl Pts',(0.709567204017975,0.343867571690883,
-5.40235846800852));
#66849=CARTESIAN_POINT('Ctrl Pts',(0.326272201059984,0.717612259834014,
-5.38117633668267));
#66850=CARTESIAN_POINT('Ctrl Pts',(-0.167093531027814,0.725129259170048,
-5.3599942053568));
#66851=CARTESIAN_POINT('Ctrl Pts',(-0.494054449540532,0.558585130097485,
-5.34410760686241));
#66852=CARTESIAN_POINT('Ctrl Pts',(-0.699549695773513,0.253698560254875,
-5.32822100836801));
#66853=CARTESIAN_POINT('Ctrl Pts',(-0.751818044764839,-0.235604579114837,
-5.30703887704216));
#66854=CARTESIAN_POINT('Ctrl Pts',(-0.346769310602394,-0.771005170269097,
-5.28056121288483));
#66855=CARTESIAN_POINT('Ctrl Pts',(0.462715394887025,-0.708277177870474,
-5.24878801589604));
#66856=CARTESIAN_POINT('Ctrl Pts',(0.779479714111498,-0.114583275476619,
-5.22231035173873));
#66857=CARTESIAN_POINT('Ctrl Pts',(0.651230414035533,0.358494296722582,
-5.20112822041286));
#66858=CARTESIAN_POINT('Ctrl Pts',(0.318222100876526,0.721432754603103,
-5.17994608908701));
#66859=CARTESIAN_POINT('Ctrl Pts',(-0.21586635990173,0.758170573687571,
-5.15876395776115));
#66860=CARTESIAN_POINT('Ctrl Pts',(-0.596771337661512,0.444518459989074,
-5.13758182643529));
#66861=CARTESIAN_POINT('Ctrl Pts',(-0.738165201609358,0.105921111256041,
-5.12169522794089));
#66862=CARTESIAN_POINT('Ctrl Pts',(-0.697422731366996,-0.259488477736339,
-5.1058086294465));
#66863=CARTESIAN_POINT('Ctrl Pts',(-0.420509614143643,-0.666266879400412,
-5.08462649812064));
#66864=CARTESIAN_POINT('Ctrl Pts',(0.234807681137167,-0.812135013536203,
-5.05814883396333));
#66865=CARTESIAN_POINT('Ctrl Pts',(0.811182371766064,-0.240302428401924,
-5.02637563697453));
#66866=CARTESIAN_POINT('Ctrl Pts',(0.668288040632482,0.417263761285658,
-4.99989797281721));
#66867=CARTESIAN_POINT('Ctrl Pts',(0.264289689312711,0.694816647086003,
-4.97871584149136));
#66868=CARTESIAN_POINT('Ctrl Pts',(-0.22447527882807,0.755871268204979,
-4.95753371016549));
#66869=CARTESIAN_POINT('Ctrl Pts',(-0.655334914948076,0.438129037376436,
-4.93635157883964));
#66870=CARTESIAN_POINT('Ctrl Pts',(-0.742613735136722,-0.0475134834709792,
-4.91516944751378));
#66871=CARTESIAN_POINT('Ctrl Pts',(-0.631191025624889,-0.397120933529679,
-4.89928284901938));
#66872=CARTESIAN_POINT('Ctrl Pts',(-0.363588706173925,-0.649258029636888,
-4.88339625052499));
#66873=CARTESIAN_POINT('Ctrl Pts',(0.110800912613465,-0.780040414297433,
-4.86221411919913));
#66874=CARTESIAN_POINT('Ctrl Pts',(0.704705826931277,-0.466998527643861,
-4.83573645504181));
#66875=CARTESIAN_POINT('Ctrl Pts',(0.773836113405174,0.341964569728843,
-4.80396325805302));
#66876=CARTESIAN_POINT('Ctrl Pts',(0.239246300374524,0.750652489166442,
-4.7774855938957));
#66877=CARTESIAN_POINT('Ctrl Pts',(-0.248352065935438,0.700671438186571,
-4.75630346256984));
#66878=CARTESIAN_POINT('Ctrl Pts',(-0.660408092917064,0.430803523328669,
-4.73512133124398));
#66879=CARTESIAN_POINT('Ctrl Pts',(-0.783114147707591,-0.0902947163604663,
-4.71393919991813));
#66880=CARTESIAN_POINT('Ctrl Pts',(-0.535255400367477,-0.516947141497766,
-4.69275706859226));
#66881=CARTESIAN_POINT('Ctrl Pts',(-0.224010804574387,-0.711284968286846,
-4.67687047009788));
#66882=CARTESIAN_POINT('Ctrl Pts',(0.143174785820403,-0.730228537521291,
-4.66098387160347));
#66883=CARTESIAN_POINT('Ctrl Pts',(0.589412490217385,-0.522812400913593,
-4.63980174027763));
#66884=CARTESIAN_POINT('Ctrl Pts',(0.839432937889302,0.100251035500731,
-4.61332407612029));
#66885=CARTESIAN_POINT('Ctrl Pts',(0.368439186224119,0.761586937528716,
-4.58155087913152));
#66886=CARTESIAN_POINT('Ctrl Pts',(-0.303585374651586,0.72701710573571,
-4.55507321497418));
#66887=CARTESIAN_POINT('Ctrl Pts',(-0.642873017066318,0.373274023838906,
-4.53389108364834));
#66888=CARTESIAN_POINT('Ctrl Pts',(-0.782238688097199,-0.0991622899429063,
-4.51270895232246));
#66889=CARTESIAN_POINT('Ctrl Pts',(-0.538429908120204,-0.575772644525661,
-4.49152682099662));
#66890=CARTESIAN_POINT('Ctrl Pts',(-0.0733197659837324,-0.740511244101904,
-4.47034468967075));
#66891=CARTESIAN_POINT('Ctrl Pts',(0.2897130696067,-0.687148807738141,-4.45445809117637));
#66892=CARTESIAN_POINT('Ctrl Pts',(0.581841719943463,-0.46388894062958,
-4.43857149268196));
#66893=CARTESIAN_POINT('Ctrl Pts',(0.787688661554364,-0.0169252069998933,
-4.41738936135611));
#66894=CARTESIAN_POINT('Ctrl Pts',(0.57491032546554,0.619819364819736,-4.39091169719878));
#66895=CARTESIAN_POINT('Ctrl Pts',(-0.212194185160404,0.818984569539605,
-4.35913850021));
#66896=CARTESIAN_POINT('Ctrl Pts',(-0.702026269447928,0.357599033471425,
-4.33266083605267));
#66897=CARTESIAN_POINT('Ctrl Pts',(-0.731631753435033,-0.13165937228476,
-4.31147870472682));
#66898=CARTESIAN_POINT('Ctrl Pts',(-0.532022195600957,-0.581964696773512,
-4.29029657340095));
#66899=CARTESIAN_POINT('Ctrl Pts',(-0.0376585147239648,-0.787402527562103,
-4.2691144420751));
#66900=CARTESIAN_POINT('Ctrl Pts',(0.423488095788453,-0.61187459781456,
-4.24793231074924));
#66901=CARTESIAN_POINT('Ctrl Pts',(0.665644086634238,-0.336192053156755,
-4.23204571225485));
#66902=CARTESIAN_POINT('Ctrl Pts',(0.743774045196498,0.0230847568156815,
-4.21615911376045));
#66903=CARTESIAN_POINT('Ctrl Pts',(0.611325637737408,0.497011926233411,
-4.1949769824346));
#66904=CARTESIAN_POINT('Ctrl Pts',(0.0369498026964951,0.844590219818537,
-4.16849931827727));
#66905=CARTESIAN_POINT('Ctrl Pts',(-0.691904104647108,0.486858097737258,
-4.13672612128848));
#66906=CARTESIAN_POINT('Ctrl Pts',(-0.766570576163524,-0.181899707242741,
-4.11024845713116));
#66907=CARTESIAN_POINT('Ctrl Pts',(-0.472412989765752,-0.573973152721816,
-4.08906632580531));
#66908=CARTESIAN_POINT('Ctrl Pts',(-0.0287661750624402,-0.787974004694965,
-4.06788419447945));
#66909=CARTESIAN_POINT('Ctrl Pts',(0.481023959960447,-0.624529306026845,
-4.04670206315358));
#66910=CARTESIAN_POINT('Ctrl Pts',(0.718877240868205,-0.192219154318652,
-4.02551993182774));
#66911=CARTESIAN_POINT('Ctrl Pts',(0.724982549969908,0.174663816848276,
-4.00963333333333));
#66912=CARTESIAN_POINT('Ctrl Pts',(0.551953773428615,0.499078919914592,
-3.99374673483894));
#66913=CARTESIAN_POINT('Ctrl Pts',(0.144204912207516,0.774561058579967,
-3.97256460351308));
#66914=CARTESIAN_POINT('Ctrl Pts',(-0.518584724903316,0.667658453424645,
-3.94608693935576));
#66915=CARTESIAN_POINT('Ctrl Pts',(-0.842531723549237,-0.0768270276205641,
-3.91431374236698));
#66916=CARTESIAN_POINT('Ctrl Pts',(-0.466519837019428,-0.634883606184656,
-3.88783607820964));
#66917=CARTESIAN_POINT('Ctrl Pts',(0.0114940687900335,-0.743294759383846,
-3.86665394688379));
#66918=CARTESIAN_POINT('Ctrl Pts',(0.4881715666929,-0.619208403023853,-3.84547181555793));
#66919=CARTESIAN_POINT('Ctrl Pts',(0.770922604173408,-0.164618475624371,
-3.82428968423208));
#66920=CARTESIAN_POINT('Ctrl Pts',(0.672355166352795,0.318859249519227,
-3.80310755290621));
#66921=CARTESIAN_POINT('Ctrl Pts',(0.439505996563567,0.60244636745652,-3.78722095441182));
#66922=CARTESIAN_POINT('Ctrl Pts',(0.0976141491142113,0.737701981966911,
-3.77133435591743));
#66923=CARTESIAN_POINT('Ctrl Pts',(-0.39150231822405,0.683714724865923,
-3.75015222459157));
#66924=CARTESIAN_POINT('Ctrl Pts',(-0.827470832334805,0.173176063494873,
-3.72367456043424));
#66925=CARTESIAN_POINT('Ctrl Pts',(-0.592435779693381,-0.603971807536539,
-3.69190136344546));
#66926=CARTESIAN_POINT('Ctrl Pts',(0.0554163053237293,-0.785905200923715,
-3.66542369928814));
#66927=CARTESIAN_POINT('Ctrl Pts',(0.489934337114234,-0.559091726160631,
-3.64424156796228));
#66928=CARTESIAN_POINT('Ctrl Pts',(0.772925944932573,-0.155935911684361,
-3.62305943663642));
#66929=CARTESIAN_POINT('Ctrl Pts',(0.694156298070137,0.373587925382995,
-3.60187730531056));
#66930=CARTESIAN_POINT('Ctrl Pts',(0.306048625366906,0.678282337700377,
-3.5806951739847));
#66931=CARTESIAN_POINT('Ctrl Pts',(-0.0550076813495416,0.743694360385653,
-3.56480857549031));
#66932=CARTESIAN_POINT('Ctrl Pts',(-0.403152557427834,0.625460431797726,
-3.54892197699592));
#66933=CARTESIAN_POINT('Ctrl Pts',(-0.741003855265364,0.267681110008094,
-3.52773984567005));
#66934=CARTESIAN_POINT('Ctrl Pts',(-0.742796613497877,-0.403672043010809,
-3.50126218151274));
#66935=CARTESIAN_POINT('Ctrl Pts',(-0.0605664975661023,-0.843856502453133,
-3.46948898452395));
#66936=CARTESIAN_POINT('Ctrl Pts',(0.550995435006661,-0.563135847142134,
-3.44301132036662));
#66937=CARTESIAN_POINT('Ctrl Pts',(0.735352835932997,-0.10897439896662,
-3.42182918904077));
#66938=CARTESIAN_POINT('Ctrl Pts',(0.690062547194971,0.381502563374796,
-3.4006470577149));
#66939=CARTESIAN_POINT('Ctrl Pts',(0.287236506823574,0.734109047274443,
-3.37946492638905));
#66940=CARTESIAN_POINT('Ctrl Pts',(-0.205820263132216,0.715101887851966,
-3.35828279506319));
#66941=CARTESIAN_POINT('Ctrl Pts',(-0.523358695669893,0.531227655853493,
-3.3423961965688));
#66942=CARTESIAN_POINT('Ctrl Pts',(-0.712172502830834,0.215738412242388,
-3.3265095980744));
#66943=CARTESIAN_POINT('Ctrl Pts',(-0.738070348497915,-0.275666557350466,
-3.30532746674855));
#66944=CARTESIAN_POINT('Ctrl Pts',(-0.304834682108662,-0.788526311492612,
-3.27884980259122));
#66945=CARTESIAN_POINT('Ctrl Pts',(0.500109323247009,-0.682387545432416,
-3.24707660560244));
#66946=CARTESIAN_POINT('Ctrl Pts',(0.784511015498687,-0.0725287411713208,
-3.22059894144511));
#66947=CARTESIAN_POINT('Ctrl Pts',(0.631024019531475,0.392973153942071,
-3.19941681011926));
#66948=CARTESIAN_POINT('Ctrl Pts',(0.278992727421459,0.737491412118594,
-3.17823467879339));
#66949=CARTESIAN_POINT('Ctrl Pts',(-0.256298242829113,0.745474422676672,
-3.15705254746754));
#66950=CARTESIAN_POINT('Ctrl Pts',(-0.619797254121925,0.411805845645958,
-3.13587041614168));
#66951=CARTESIAN_POINT('Ctrl Pts',(-0.742790701640324,0.0660993209764941,
-3.11998381764728));
#66952=CARTESIAN_POINT('Ctrl Pts',(-0.682470125197199,-0.296592758708842,
-3.1040972191529));
#66953=CARTESIAN_POINT('Ctrl Pts',(-0.384097027620931,-0.687902146781113,
-3.08291508782703));
#66954=CARTESIAN_POINT('Ctrl Pts',(0.278112223083316,-0.798342983124478,
-3.05643742366971));
#66955=CARTESIAN_POINT('Ctrl Pts',(0.82292396426287,-0.196362538183184,
-3.02466422668092));
#66956=CARTESIAN_POINT('Ctrl Pts',(0.644898747665643,0.452574366258134,
-2.9981865625236));
#66957=CARTESIAN_POINT('Ctrl Pts',(0.226568589229536,0.708015456977724,
-2.97700443119774));
#66958=CARTESIAN_POINT('Ctrl Pts',(-0.264771157858471,0.742715799528351,
-2.95582229987188));
#66959=CARTESIAN_POINT('Ctrl Pts',(-0.677932840683997,0.402278470297038,
-2.93464016854602));
#66960=CARTESIAN_POINT('Ctrl Pts',(-0.738987287045408,-0.0873526205132272,
-2.91345803722017));
#66961=CARTESIAN_POINT('Ctrl Pts',(-0.608937806846517,-0.43046706502338,
-2.89757143872577));
#66962=CARTESIAN_POINT('Ctrl Pts',(-0.328172420882141,-0.667858966008211,
-2.88168484023138));
#66963=CARTESIAN_POINT('Ctrl Pts',(0.152559894420231,-0.772958840293439,
-2.86050270890552));
#66964=CARTESIAN_POINT('Ctrl Pts',(0.728783846804567,-0.428453068572477,
-2.8340250447482));
#66965=CARTESIAN_POINT('Ctrl Pts',(0.754340852979042,0.383056098876796,
-2.80225184775941));
#66966=CARTESIAN_POINT('Ctrl Pts',(0.198560790390178,0.76242479252337,-2.77577418360209));
#66967=CARTESIAN_POINT('Ctrl Pts',(-0.285647023564601,0.686312604338228,
-2.75459205227623));
#66968=CARTESIAN_POINT('Ctrl Pts',(-0.682605017328055,0.394690910994047,
-2.73340992095037));
#66969=CARTESIAN_POINT('Ctrl Pts',(-0.777130127709657,-0.132248511327643,
-2.71222778962451));
#66970=CARTESIAN_POINT('Ctrl Pts',(-0.506701393044462,-0.544964575924034,
-2.69104565829866));
#66971=CARTESIAN_POINT('Ctrl Pts',(-0.185462906569463,-0.722295408377821,
-2.67515905980426));
#66972=CARTESIAN_POINT('Ctrl Pts',(0.182210114447717,-0.721479182304072,
-2.65927246130987));
#66973=CARTESIAN_POINT('Ctrl Pts',(0.616656528560847,-0.490382112190671,
-2.63809032998401));
#66974=CARTESIAN_POINT('Ctrl Pts',(0.832832487189643,0.145216994921211,
-2.61161266582669));
#66975=CARTESIAN_POINT('Ctrl Pts',(0.326979376809108,0.780286219602388,
-2.5798394688379));
#66976=CARTESIAN_POINT('Ctrl Pts',(-0.342216325821634,0.709651983775012,
-2.55336180468057));
#66977=CARTESIAN_POINT('Ctrl Pts',(-0.662003665385102,0.338186871361864,
-2.53217967335472));
#66978=CARTESIAN_POINT('Ctrl Pts',(-0.775779392941181,-0.14105622421774,
-2.51099754202885));
#66979=CARTESIAN_POINT('Ctrl Pts',(-0.506710052209743,-0.603875671915998,
-2.489815410703));
#66980=CARTESIAN_POINT('Ctrl Pts',(-0.0334190097720498,-0.74338136949423,
-2.46863327937714));
#66981=CARTESIAN_POINT('Ctrl Pts',(0.32622155852598,-0.670586788886994,
-2.45274668088275));
#66982=CARTESIAN_POINT('Ctrl Pts',(0.605930172637336,-0.431950647867195,
-2.43686008238835));
#66983=CARTESIAN_POINT('Ctrl Pts',(0.787459991398773,0.0254293554683121,
-2.4156779510625));
#66984=CARTESIAN_POINT('Ctrl Pts',(0.540770699778186,0.649819188385389,
-2.38920028690517));
#66985=CARTESIAN_POINT('Ctrl Pts',(-0.255899496701508,0.806397882529322,
-2.35742708991639));
#66986=CARTESIAN_POINT('Ctrl Pts',(-0.720229071880726,0.319355657148115,
-2.33094942575906));
#66987=CARTESIAN_POINT('Ctrl Pts',(-0.723499204724565,-0.170786749215974,
-2.3097672944332));
#66988=CARTESIAN_POINT('Ctrl Pts',(-0.49997884029397,-0.609714428368757,
-2.28858516310735));
#66989=CARTESIAN_POINT('Ctrl Pts',(0.00471063101971821,-0.788288471371872,
-2.26740303178148));
#66990=CARTESIAN_POINT('Ctrl Pts',(0.455758068365152,-0.588232329819882,
-2.24622090045563));
#66991=CARTESIAN_POINT('Ctrl Pts',(0.682749058575273,-0.299934775728751,
-2.23033430196123));
#66992=CARTESIAN_POINT('Ctrl Pts',(0.741458711415728,0.0630215484650262,
-2.21444770346684));
#66993=CARTESIAN_POINT('Ctrl Pts',(0.583733018808828,0.529146154597792,
-2.19326557214099));
#66994=CARTESIAN_POINT('Ctrl Pts',(-0.00849156494869494,0.845355440425599,
-2.16678790798366));
#66995=CARTESIAN_POINT('Ctrl Pts',(-0.717067869396526,0.448971901168643,
-2.13501471099488));
#66996=CARTESIAN_POINT('Ctrl Pts',(-0.755687642685574,-0.222832085721485,
-2.10853704683755));
#66997=CARTESIAN_POINT('Ctrl Pts',(-0.440885233565745,-0.598531054974189,
-2.08735491551169));
#66998=CARTESIAN_POINT('Ctrl Pts',(0.0136208320613828,-0.788381251576107,
-2.06617278418583));
#66999=CARTESIAN_POINT('Ctrl Pts',(0.513890851614579,-0.597776795107706,
-2.04499065285998));
#67000=CARTESIAN_POINT('Ctrl Pts',(0.728168238139964,-0.153309189840012,
-2.02380852153411));
#67001=CARTESIAN_POINT('Ctrl Pts',(0.714548566105297,0.213371725759888,
-2.00792192303973));
#67002=CARTESIAN_POINT('Ctrl Pts',(0.524335868445759,0.528019538811239,
-1.99203532454533));
#67003=CARTESIAN_POINT('Ctrl Pts',(0.102371900870404,0.781191323611233,
-1.97085319321948));
#67004=CARTESIAN_POINT('Ctrl Pts',(-0.553715085418805,0.638825118097339,
-1.94437552906215));
#67005=CARTESIAN_POINT('Ctrl Pts',(-0.837185592801576,-0.121993362792136,
-1.91260233207336));
#67006=CARTESIAN_POINT('Ctrl Pts',(-0.431727290682992,-0.659036795796866,
-1.88612466791603));
#67007=CARTESIAN_POINT('Ctrl Pts',(0.051421852550958,-0.741602997583657,
-1.86494253659018));
#67008=CARTESIAN_POINT('Ctrl Pts',(0.520742186510374,-0.592079471094158,
-1.84376040526432));
#67009=CARTESIAN_POINT('Ctrl Pts',(0.778655144391046,-0.122951495540993,
-1.82257827393846));
#67010=CARTESIAN_POINT('Ctrl Pts',(0.654248219366565,0.354530616704593,
-1.8013961426126));
#67011=CARTESIAN_POINT('Ctrl Pts',(0.406495651263466,0.625194715413342,
-1.78550954411821));
#67012=CARTESIAN_POINT('Ctrl Pts',(0.0578292558056736,0.741881738202362,
-1.76962294562382));
#67013=CARTESIAN_POINT('Ctrl Pts',(-0.427679173417961,0.661687550735103,
-1.74844081429796));
#67014=CARTESIAN_POINT('Ctrl Pts',(-0.835581541009314,0.12845783610561,
-1.72196315014064));
#67015=CARTESIAN_POINT('Ctrl Pts',(-0.559122471426269,-0.63493634271952,
-1.69018995315185));
#67016=CARTESIAN_POINT('Ctrl Pts',(0.0975704904356342,-0.781791501060753,
-1.66371228899453));
#67017=CARTESIAN_POINT('Ctrl Pts',(0.519271761113482,-0.53195493329317,
-1.64253015766867));
#67018=CARTESIAN_POINT('Ctrl Pts',(0.780188992423923,-0.114173819255057,
-1.62134802634281));
#67019=CARTESIAN_POINT('Ctrl Pts',(0.673076748697835,0.410351793592717,
-1.60016589501695));
#67020=CARTESIAN_POINT('Ctrl Pts',(0.269155730685218,0.69374915017214,-1.57898376369109));
#67021=CARTESIAN_POINT('Ctrl Pts',(-0.0948940615492358,0.73966361527357,
-1.5630971651967));
#67022=CARTESIAN_POINT('Ctrl Pts',(-0.436182013063224,0.602891356535583,
-1.54721056670231));
#67023=CARTESIAN_POINT('Ctrl Pts',(-0.754318177514541,0.227473025311658,
-1.52602843537645));
#67024=CARTESIAN_POINT('Ctrl Pts',(-0.720030068313977,-0.443006352162364,
-1.49955077121913));
#67025=CARTESIAN_POINT('Ctrl Pts',(-0.0151304330670991,-0.84589193597945,
-1.46777757423034));
#67026=CARTESIAN_POINT('Ctrl Pts',(0.580461954196043,-0.53271180901645,
-1.44129991007302));
#67027=CARTESIAN_POINT('Ctrl Pts',(0.740146482467141,-0.0692993321494254,
-1.42011777874716));
#67028=CARTESIAN_POINT('Ctrl Pts',(0.668563583570739,0.418034998087244,
-1.3989356474213));
#67029=CARTESIAN_POINT('Ctrl Pts',(0.247370688717346,0.748484232636805,
-1.37775351609544));
#67030=CARTESIAN_POINT('Ctrl Pts',(-0.24395216717569,0.703007845514929,
-1.35657138476958));
#67031=CARTESIAN_POINT('Ctrl Pts',(-0.551150415740897,0.502334914081758,
-1.34068478627519));
#67032=CARTESIAN_POINT('Ctrl Pts',(-0.722737105030778,0.177154772210434,
-1.32479818778079));
#67033=CARTESIAN_POINT('Ctrl Pts',(-0.722189601592419,-0.314931849016698,
-1.30361605645494));
#67034=CARTESIAN_POINT('Ctrl Pts',(-0.262019070115917,-0.803768582508686,
-1.27713839229761));
#67035=CARTESIAN_POINT('Ctrl Pts',(0.536057917164077,-0.654525787731523,
-1.24536519530883));
#67036=CARTESIAN_POINT('Ctrl Pts',(0.7872750510185,-0.0302645961231062,
-1.2188875311515));
#67037=CARTESIAN_POINT('Ctrl Pts',(0.608993942262501,0.426316304206648,
-1.19770539982565));
#67038=CARTESIAN_POINT('Ctrl Pts',(0.238957054659373,0.751418692162539,
-1.17652326849978));
#67039=CARTESIAN_POINT('Ctrl Pts',(-0.295989414350265,0.730623822999904,
-1.15534113717393));
#67040=CARTESIAN_POINT('Ctrl Pts',(-0.641031933583759,0.377903097170594,
-1.13415900584807));
#67041=CARTESIAN_POINT('Ctrl Pts',(-0.745269509057839,0.0260865012135712,
-1.11827240735367));
#67042=CARTESIAN_POINT('Ctrl Pts',(-0.665545155112125,-0.332839875633884,
-1.10238580885928));
#67043=CARTESIAN_POINT('Ctrl Pts',(-0.34657438647555,-0.707549351503058,
-1.08120367753342));
#67044=CARTESIAN_POINT('Ctrl Pts',(0.320613010413704,-0.782243711950361,
-1.0547260133761));
#67045=CARTESIAN_POINT('Ctrl Pts',(0.832287276052231,-0.151855152963071,
-1.02295281638731));
#67046=CARTESIAN_POINT('Ctrl Pts',(0.619645673454765,0.48657701456549,-0.996475152229989));
#67047=CARTESIAN_POINT('Ctrl Pts',(0.18819269753976,0.719168075999973,-0.975293020904133));
#67048=CARTESIAN_POINT('Ctrl Pts',(-0.304301838445365,0.727413854708367,
-0.954110889578274));
#67049=CARTESIAN_POINT('Ctrl Pts',(-0.698571515424613,0.36526530355274,
-0.932928758252416));
#67050=CARTESIAN_POINT('Ctrl Pts',(-0.733225138349833,-0.126939305249656,
-0.911746626926556));
#67051=CARTESIAN_POINT('Ctrl Pts',(-0.584924735273482,-0.462569130771008,
-0.895860028432164));
#67052=CARTESIAN_POINT('Ctrl Pts',(-0.291807705151121,-0.684529765254048,
-0.879973429937768));
#67053=CARTESIAN_POINT('Ctrl Pts',(0.193877972488015,-0.763643386640963,
-0.858791298611913));
#67054=CARTESIAN_POINT('Ctrl Pts',(0.750755654391034,-0.388669364275005,
-0.832313634454587));
#67055=CARTESIAN_POINT('Ctrl Pts',(0.732665519578818,0.423040581718017,
-0.800540437465801));
#67056=CARTESIAN_POINT('Ctrl Pts',(0.157301432367607,0.771993660029016,
-0.774062773308477));
#67057=CARTESIAN_POINT('Ctrl Pts',(-0.322116450716943,0.669970301652722,
-0.752880641982619));
#67058=CARTESIAN_POINT('Ctrl Pts',(-0.702829188003266,0.357437627360335,
-0.731698510656762));
#67059=CARTESIAN_POINT('Ctrl Pts',(-0.768900172839997,-0.173820103281627,
-0.710516379330902));
#67060=CARTESIAN_POINT('Ctrl Pts',(-0.47668300000339,-0.571407042463865,
-0.689334248005046));
#67061=CARTESIAN_POINT('Ctrl Pts',(-0.146379013782528,-0.731218388212433,
-0.673447649510651));
#67062=CARTESIAN_POINT('Ctrl Pts',(0.220718848884244,-0.710644725186344,
-0.657561051016257));
#67063=CARTESIAN_POINT('Ctrl Pts',(0.642118407188864,-0.45653460181011,
-0.6363789196904));
#67064=CARTESIAN_POINT('Ctrl Pts',(0.823825118811679,0.189763273491745,
-0.609901255533075));
#67065=CARTESIAN_POINT('Ctrl Pts',(0.28457458659541,0.796730442765568,-0.578128058544289));
#67066=CARTESIAN_POINT('Ctrl Pts',(-0.379858261997401,0.690235946123353,
-0.551650394386966));
#67067=CARTESIAN_POINT('Ctrl Pts',(-0.679221094819627,0.302122339919885,
-0.530468263061107));
#67068=CARTESIAN_POINT('Ctrl Pts',(-0.767078076405924,-0.182542484323307,
-0.50928613173525));
#67069=CARTESIAN_POINT('Ctrl Pts',(-0.473525765627643,-0.630233509741301,
-0.488104000409389));
#67070=CARTESIAN_POINT('Ctrl Pts',(0.00657830405987886,-0.744103053859658,
-0.466921869083533));
#67071=CARTESIAN_POINT('Ctrl Pts',(0.361787306164901,-0.652086835470523,
-0.451035270589137));
#67072=CARTESIAN_POINT('Ctrl Pts',(0.628267371514877,-0.398763844762359,
-0.435148672094745));
#67073=CARTESIAN_POINT('Ctrl Pts',(0.784955734091449,0.0677100869688686,
-0.413966540768886));
#67074=CARTESIAN_POINT('Ctrl Pts',(0.505067810210761,0.677941712115777,
-0.387488876611564));
#67075=CARTESIAN_POINT('Ctrl Pts',(-0.298864521600004,0.791479450126972,
-0.355715679622777));
#67076=CARTESIAN_POINT('Ctrl Pts',(-0.736351606015524,0.280191386843895,
-0.329238015465453));
#67077=CARTESIAN_POINT('Ctrl Pts',(-0.713274091724115,-0.209423283087674,
-0.308055884139594));
#67078=CARTESIAN_POINT('Ctrl Pts',(-0.466494711648086,-0.635695014837649,
-0.286873752813737));
#67079=CARTESIAN_POINT('Ctrl Pts',(0.0470746703232514,-0.786910562942938,
-0.265691621487877));
#67080=CARTESIAN_POINT('Ctrl Pts',(0.486700370550275,-0.562872340213963,
-0.244509490162019));
#67081=CARTESIAN_POINT('Ctrl Pts',(0.69790273612906,-0.262847524723207,
-0.228622891667627));
#67082=CARTESIAN_POINT('Ctrl Pts',(0.736960633613606,0.10284341760348,-0.212736293173231));
#67083=CARTESIAN_POINT('Ctrl Pts',(0.554539603465115,0.559605906724123,
-0.191554161847375));
#67084=CARTESIAN_POINT('Ctrl Pts',(-0.0540867686931964,0.843978018413933,
-0.165076497690051));
#67085=CARTESIAN_POINT('Ctrl Pts',(-0.739847523655629,0.409263047681452,
-0.133303300701265));
#67086=CARTESIAN_POINT('Ctrl Pts',(-0.743144735960948,-0.262238058905764,
-0.10682563654394));
#67087=CARTESIAN_POINT('Ctrl Pts',(-0.407377385049017,-0.622546633323945,
-0.0856435052180836));
#67088=CARTESIAN_POINT('Ctrl Pts',(-0.0613458632290381,-0.74305434807241,
-0.0697569067236874));
#67089=CARTESIAN_POINT('Ctrl Pts',(0.302742394164461,-0.680954303180219,
-0.0538703082292963));
#67090=CARTESIAN_POINT('Ctrl Pts',(0.494975304259394,-0.529271880382184,
-0.043279242566365));
#67091=CARTESIAN_POINT('Ctrl Pts',(0.567325265044049,-0.434889340047722,
-0.0379837097349007));
#67092=CARTESIAN_POINT('Ctrl Pts',(-0.325579286441984,0.678938089483158,
-11.9309162902651));
#67093=CARTESIAN_POINT('Ctrl Pts',(-0.438530190559174,0.624773394152179,
-11.9256207574336));
#67094=CARTESIAN_POINT('Ctrl Pts',(-0.636487869789445,0.459419899431822,
-11.9150296917707));
#67095=CARTESIAN_POINT('Ctrl Pts',(-0.779277659860866,0.0975214801954652,
-11.8991430932763));
#67096=CARTESIAN_POINT('Ctrl Pts',(-0.729912798382054,-0.285270244336759,
-11.8832564947819));
#67097=CARTESIAN_POINT('Ctrl Pts',(-0.431119590957509,-0.709362437639476,
-11.8620743634561));
#67098=CARTESIAN_POINT('Ctrl Pts',(0.261835732470835,-0.851244765286553,
-11.8355966992988));
#67099=CARTESIAN_POINT('Ctrl Pts',(0.85834437572654,-0.238354668512496,
-11.8038235023099));
#67100=CARTESIAN_POINT('Ctrl Pts',(0.69686701284205,0.45059533067605,-11.7773458381526));
#67101=CARTESIAN_POINT('Ctrl Pts',(0.265463729879274,0.737472858364993,
-11.7561637068268));
#67102=CARTESIAN_POINT('Ctrl Pts',(-0.119972716722838,0.776326956521568,
-11.7402771083324));
#67103=CARTESIAN_POINT('Ctrl Pts',(-0.474958785797699,0.623512435543155,
-11.724390509838));
#67104=CARTESIAN_POINT('Ctrl Pts',(-0.801031350365818,0.218779261424542,
-11.7032083785121));
#67105=CARTESIAN_POINT('Ctrl Pts',(-0.756257517900422,-0.34336885159689,
-11.6820262471863));
#67106=CARTESIAN_POINT('Ctrl Pts',(-0.370210901362501,-0.689995813217701,
-11.6608441158604));
#67107=CARTESIAN_POINT('Ctrl Pts',(0.129533749630415,-0.81971580735925,
-11.6396619845346));
#67108=CARTESIAN_POINT('Ctrl Pts',(0.751265829807233,-0.479334713936513,
-11.6131843203772));
#67109=CARTESIAN_POINT('Ctrl Pts',(0.808154513003672,0.373993162759316,
-11.5814111233884));
#67110=CARTESIAN_POINT('Ctrl Pts',(0.239629116940131,0.794551604670445,
-11.5549334592311));
#67111=CARTESIAN_POINT('Ctrl Pts',(-0.275152955319875,0.73394666811328,
-11.5337513279053));
#67112=CARTESIAN_POINT('Ctrl Pts',(-0.593954211107484,0.514042981534784,
-11.5178647294109));
#67113=CARTESIAN_POINT('Ctrl Pts',(-0.765663149550031,0.167770532262155,
-11.5019781309165));
#67114=CARTESIAN_POINT('Ctrl Pts',(-0.752148512370767,-0.351798689683568,
-11.4807959995906));
#67115=CARTESIAN_POINT('Ctrl Pts',(-0.354140489117332,-0.751277403168843,
-11.4596138682647));
#67116=CARTESIAN_POINT('Ctrl Pts',(0.164502456835433,-0.765565519913649,
-11.4384317369389));
#67117=CARTESIAN_POINT('Ctrl Pts',(0.62937193641715,-0.540925780748815,
-11.417249605613));
#67118=CARTESIAN_POINT('Ctrl Pts',(0.882907902300928,0.120989182847097,
-11.3907719414557));
#67119=CARTESIAN_POINT('Ctrl Pts',(0.373861710521524,0.808214967858265,
-11.3589987444669));
#67120=CARTESIAN_POINT('Ctrl Pts',(-0.331711379690762,0.760724410311425,
-11.3325210803096));
#67121=CARTESIAN_POINT('Ctrl Pts',(-0.684841401373326,0.381286484920216,
-11.3113389489838));
#67122=CARTESIAN_POINT('Ctrl Pts',(-0.785473309452427,0.00730113817008764,
-11.2954523504893));
#67123=CARTESIAN_POINT('Ctrl Pts',(-0.69218813210121,-0.367780734196896,
-11.279565751995));
#67124=CARTESIAN_POINT('Ctrl Pts',(-0.345542913605394,-0.755042893881491,
-11.2583836206691));
#67125=CARTESIAN_POINT('Ctrl Pts',(0.216418598618142,-0.801870440168425,
-11.2372014893433));
#67126=CARTESIAN_POINT('Ctrl Pts',(0.620972963907686,-0.477015944868456,
-11.2160193580174));
#67127=CARTESIAN_POINT('Ctrl Pts',(0.82987111893074,-0.00486321422972745,
-11.1948372266915));
#67128=CARTESIAN_POINT('Ctrl Pts',(0.594621657647541,0.663769413694489,
-11.1683595625342));
#67129=CARTESIAN_POINT('Ctrl Pts',(-0.238245957352548,0.858034310357582,
-11.1365863655454));
#67130=CARTESIAN_POINT('Ctrl Pts',(-0.745284156508827,0.365082993917505,
-11.1101087013881));
#67131=CARTESIAN_POINT('Ctrl Pts',(-0.768806557073455,-0.152720683283362,
-11.0889265700622));
#67132=CARTESIAN_POINT('Ctrl Pts',(-0.603406952189243,-0.502913189569635,
-11.0730399715678));
#67133=CARTESIAN_POINT('Ctrl Pts',(-0.289495688199805,-0.728408762470549,
-11.0571533730735));
#67134=CARTESIAN_POINT('Ctrl Pts',(0.225409211463697,-0.799174802017602,
-11.0359712417476));
#67135=CARTESIAN_POINT('Ctrl Pts',(0.684045040627252,-0.471079181211703,
-11.0147891104217));
#67136=CARTESIAN_POINT('Ctrl Pts',(0.782097317996387,0.038411180330575,
-10.9936069790959));
#67137=CARTESIAN_POINT('Ctrl Pts',(0.635668359101772,0.533512382338015,
-10.97242484777));
#67138=CARTESIAN_POINT('Ctrl Pts',(0.0235224284446957,0.890848722095813,
-10.9459471836127));
#67139=CARTESIAN_POINT('Ctrl Pts',(-0.737039470499595,0.499756773719366,
-10.9141739866239));
#67140=CARTESIAN_POINT('Ctrl Pts',(-0.804386100341556,-0.204198599320718,
-10.8876963224666));
#67141=CARTESIAN_POINT('Ctrl Pts',(-0.487113192994437,-0.614091089752501,
-10.8665141911407));
#67142=CARTESIAN_POINT('Ctrl Pts',(-0.134349165685502,-0.773932767023663,
-10.8506275926463));
#67143=CARTESIAN_POINT('Ctrl Pts',(0.250886222352188,-0.742592204486319,
-10.8347409941519));
#67144=CARTESIAN_POINT('Ctrl Pts',(0.689152575330391,-0.463204495561479,
-10.8135588628261));
#67145=CARTESIAN_POINT('Ctrl Pts',(0.826327097284044,0.0837659887530412,
-10.7923767315002));
#67146=CARTESIAN_POINT('Ctrl Pts',(0.571241822611821,0.535569242666811,
-10.7711946001744));
#67147=CARTESIAN_POINT('Ctrl Pts',(0.139130052178819,0.818139690671364,
-10.7500124688485));
#67148=CARTESIAN_POINT('Ctrl Pts',(-0.558764499776105,0.694224015782814,
-10.7235348046912));
#67149=CARTESIAN_POINT('Ctrl Pts',(-0.885283474044109,-0.0962142636885308,
-10.6917616077024));
#67150=CARTESIAN_POINT('Ctrl Pts',(-0.480907240447861,-0.676359588142325,
-10.6652839435451));
#67151=CARTESIAN_POINT('Ctrl Pts',(0.0262601526305759,-0.783388494737106,
-10.6441018122192));
#67152=CARTESIAN_POINT('Ctrl Pts',(0.398607551650078,-0.6768557054209,-10.6282152137248));
#67153=CARTESIAN_POINT('Ctrl Pts',(0.671942037449668,-0.403585154630335,
-10.6123286152304));
#67154=CARTESIAN_POINT('Ctrl Pts',(0.825122316493558,0.0930743768025403,
-10.5911464839046));
#67155=CARTESIAN_POINT('Ctrl Pts',(0.575592809069977,0.598770515911213,
-10.5699643525787));
#67156=CARTESIAN_POINT('Ctrl Pts',(0.0886932242196915,0.778000736226575,
-10.5487822212528));
#67157=CARTESIAN_POINT('Ctrl Pts',(-0.423581063004594,0.713644735099345,
-10.527600089927));
#67158=CARTESIAN_POINT('Ctrl Pts',(-0.875292768904854,0.167413616538596,
-10.5011224257697));
#67159=CARTESIAN_POINT('Ctrl Pts',(-0.612470397060775,-0.646424030089341,
-10.4693492287809));
#67160=CARTESIAN_POINT('Ctrl Pts',(0.0712999359732703,-0.826831533939921,
-10.4428715646235));
#67161=CARTESIAN_POINT('Ctrl Pts',(0.527143687336232,-0.580091942888548,
-10.4216894332977));
#67162=CARTESIAN_POINT('Ctrl Pts',(0.741979196074009,-0.2578536383041,-10.4058028348033));
#67163=CARTESIAN_POINT('Ctrl Pts',(0.773409877771076,0.12737440753987,-10.3899162363089));
#67164=CARTESIAN_POINT('Ctrl Pts',(0.568648728658316,0.605085366033717,
-10.368734104983));
#67165=CARTESIAN_POINT('Ctrl Pts',(0.0510960087729735,0.828988787900728,
-10.3475519736572));
#67166=CARTESIAN_POINT('Ctrl Pts',(-0.436039500666917,0.650400789859394,
-10.3263698423313));
#67167=CARTESIAN_POINT('Ctrl Pts',(-0.784829244580027,0.269727235782853,
-10.3051877110055));
#67168=CARTESIAN_POINT('Ctrl Pts',(-0.775515720372333,-0.439021773668505,
-10.2787100468482));
#67169=CARTESIAN_POINT('Ctrl Pts',(-0.0483551498041389,-0.889182654711702,
-10.2469368498594));
#67170=CARTESIAN_POINT('Ctrl Pts',(0.589595553257777,-0.584047215527897,
-10.220459185702));
#67171=CARTESIAN_POINT('Ctrl Pts',(0.777308002135367,-0.100893008275974,
-10.1992770543762));
#67172=CARTESIAN_POINT('Ctrl Pts',(0.732451906686202,0.28378835526681,-10.1833904558818));
#67173=CARTESIAN_POINT('Ctrl Pts',(0.507029774768671,0.597752361959393,
-10.1675038573874));
#67174=CARTESIAN_POINT('Ctrl Pts',(0.0417153609279727,0.829306641391184,
-10.1463217260615));
#67175=CARTESIAN_POINT('Ctrl Pts',(-0.497702991792484,0.664924766073919,
-10.1251395947357));
#67176=CARTESIAN_POINT('Ctrl Pts',(-0.753383830165404,0.213458281724755,
-10.1039574634098));
#67177=CARTESIAN_POINT('Ctrl Pts',(-0.772798222234306,-0.302477491034639,
-10.082775332084));
#67178=CARTESIAN_POINT('Ctrl Pts',(-0.306889151096186,-0.836650344671608,
-10.0562976679267));
#67179=CARTESIAN_POINT('Ctrl Pts',(0.538758694853179,-0.709029676863268,
-10.0245244709379));
#67180=CARTESIAN_POINT('Ctrl Pts',(0.827468696130943,-0.0634793140368794,
-9.99804680678052));
#67181=CARTESIAN_POINT('Ctrl Pts',(0.657770354064988,0.42629249420541,-9.97686467545469));
#67182=CARTESIAN_POINT('Ctrl Pts',(0.374557037310136,0.690455394645263,
-9.96097807696027));
#67183=CARTESIAN_POINT('Ctrl Pts',(-0.000503001884737476,0.783828313930485,
-9.94509147846589));
#67184=CARTESIAN_POINT('Ctrl Pts',(-0.505058598658514,0.659094445974152,
-9.92390934714003));
#67185=CARTESIAN_POINT('Ctrl Pts',(-0.809785307998288,0.184610312625709,
-9.90272721581418));
#67186=CARTESIAN_POINT('Ctrl Pts',(-0.71240497240588,-0.325008905851757,
-9.88154508448831));
#67187=CARTESIAN_POINT('Ctrl Pts',(-0.393210171172526,-0.730818367419422,
-9.86036295316246));
#67188=CARTESIAN_POINT('Ctrl Pts',(0.307699535168253,-0.836352644735999,
-9.83388528900513));
#67189=CARTESIAN_POINT('Ctrl Pts',(0.869629008692517,-0.191649161733625,
-9.80211209201635));
#67190=CARTESIAN_POINT('Ctrl Pts',(0.671782528753483,0.487280515154063,
-9.77563442785901));
#67191=CARTESIAN_POINT('Ctrl Pts',(0.225385044131932,0.750725456598015,
-9.75445229653317));
#67192=CARTESIAN_POINT('Ctrl Pts',(-0.161484038614348,0.768729166524916,
-9.73856569803877));
#67193=CARTESIAN_POINT('Ctrl Pts',(-0.507796541602976,0.597101122981744,
-9.72267909954437));
#67194=CARTESIAN_POINT('Ctrl Pts',(-0.81161741215718,0.175404826262443,
-9.70149696821852));
#67195=CARTESIAN_POINT('Ctrl Pts',(-0.736718858145562,-0.383508196301391,
-9.68031483689266));
#67196=CARTESIAN_POINT('Ctrl Pts',(-0.332593224809995,-0.708895888267146,
-9.6591327055668));
#67197=CARTESIAN_POINT('Ctrl Pts',(0.173395859510444,-0.811568605094942,
-9.63795057424095));
#67198=CARTESIAN_POINT('Ctrl Pts',(0.775940670895153,-0.438270265418998,
-9.61147291008361));
#67199=CARTESIAN_POINT('Ctrl Pts',(0.786887793255583,0.416883214795328,
-9.57969971309484));
#67200=CARTESIAN_POINT('Ctrl Pts',(0.196584251865598,0.806280781307404,
-9.5532220489375));
#67201=CARTESIAN_POINT('Ctrl Pts',(-0.314197532506346,0.718099603028419,
-9.53203991761166));
#67202=CARTESIAN_POINT('Ctrl Pts',(-0.620720339747097,0.481381227321487,
-9.51615331911726));
#67203=CARTESIAN_POINT('Ctrl Pts',(-0.773572719280374,0.126381670803847,
-9.50026672062285));
#67204=CARTESIAN_POINT('Ctrl Pts',(-0.732156077208528,-0.391710550533803,
-9.47908458929703));
#67205=CARTESIAN_POINT('Ctrl Pts',(-0.313255387818101,-0.769223163055156,
-9.45790245797111));
#67206=CARTESIAN_POINT('Ctrl Pts',(0.205405969347057,-0.755618965714978,
-9.43672032664531));
#67207=CARTESIAN_POINT('Ctrl Pts',(0.657531634595437,-0.506321907858398,
-9.41553819531941));
#67208=CARTESIAN_POINT('Ctrl Pts',(0.875130171604578,0.168261501975349,
-9.38906053116212));
#67209=CARTESIAN_POINT('Ctrl Pts',(0.329888290337415,0.827138277346046,
-9.35728733417332));
#67210=CARTESIAN_POINT('Ctrl Pts',(-0.372113105932665,0.741799098665116,
-9.33080967001599));
#67211=CARTESIAN_POINT('Ctrl Pts',(-0.704341991722376,0.343932388703371,
-9.30962753869014));
#67212=CARTESIAN_POINT('Ctrl Pts',(-0.784730646335707,-0.0349204652723357,
-9.29374094019574));
#67213=CARTESIAN_POINT('Ctrl Pts',(-0.671423503221182,-0.404447225299171,
-9.27785434170135));
#67214=CARTESIAN_POINT('Ctrl Pts',(-0.304467864204802,-0.772521194828622,
-9.25667221037549));
#67215=CARTESIAN_POINT('Ctrl Pts',(0.259198098613203,-0.789081464902673,
-9.23549007904963));
#67216=CARTESIAN_POINT('Ctrl Pts',(0.645710311728348,-0.442955784384013,
-9.21430794772378));
#67217=CARTESIAN_POINT('Ctrl Pts',(0.828933287182104,0.0397407885250041,
-9.19312581639791));
#67218=CARTESIAN_POINT('Ctrl Pts',(0.558091688915222,0.694765008519724,
-9.1666481522406));
#67219=CARTESIAN_POINT('Ctrl Pts',(-0.2840121426244,0.84399118288915,-9.13487495525182));
#67220=CARTESIAN_POINT('Ctrl Pts',(-0.763826635834081,0.324504139846667,
-9.10839729109447));
#67221=CARTESIAN_POINT('Ctrl Pts',(-0.759488462810364,-0.193815386800432,
-9.08721515976864));
#67222=CARTESIAN_POINT('Ctrl Pts',(-0.575508644139153,-0.534613343187773,
-9.07132856127422));
#67223=CARTESIAN_POINT('Ctrl Pts',(-0.249932936789059,-0.742913592443966,
-9.05544196277984));
#67224=CARTESIAN_POINT('Ctrl Pts',(0.268030857269164,-0.785906569729782,
-9.03425983145398));
#67225=CARTESIAN_POINT('Ctrl Pts',(0.708372208573284,-0.433638128741758,
-9.01307770012811));
#67226=CARTESIAN_POINT('Ctrl Pts',(0.778902969892766,0.0803853039044273,
-8.99189556880227));
#67227=CARTESIAN_POINT('Ctrl Pts',(0.606079043113628,0.566902035954701,
-8.9707134374764));
#67228=CARTESIAN_POINT('Ctrl Pts',(-0.0243854516630399,0.890825516050617,
-8.94423577331908));
#67229=CARTESIAN_POINT('Ctrl Pts',(-0.762831184016125,0.459426380005858,
-8.91246257633029));
#67230=CARTESIAN_POINT('Ctrl Pts',(-0.792250188295256,-0.247130948149693,
-8.88598491217298));
#67231=CARTESIAN_POINT('Ctrl Pts',(-0.453408271228742,-0.639381004475433,
-8.86480278084711));
#67232=CARTESIAN_POINT('Ctrl Pts',(-0.0925641602466446,-0.78003429567624,
-8.84891618235272));
#67233=CARTESIAN_POINT('Ctrl Pts',(0.29043032497467,-0.728036609701126,
-8.83302958385833));
#67234=CARTESIAN_POINT('Ctrl Pts',(0.713049180021141,-0.425500345081005,
-8.81184745253247));
#67235=CARTESIAN_POINT('Ctrl Pts',(0.820631485246796,0.128051466212941,
-8.7906653212066));
#67236=CARTESIAN_POINT('Ctrl Pts',(0.541635069226991,0.565493665194448,
-8.76948318988076));
#67237=CARTESIAN_POINT('Ctrl Pts',(0.0949624741010667,0.824434262621175,
-8.74830105855488));
#67238=CARTESIAN_POINT('Ctrl Pts',(-0.595264423535308,0.66319304608299,
-8.72182339439759));
#67239=CARTESIAN_POINT('Ctrl Pts',(-0.878833703135999,-0.143650047633126,
-8.69005019740877));
#67240=CARTESIAN_POINT('Ctrl Pts',(-0.44386499970157,-0.701226018076312,
-8.66357253325146));
#67241=CARTESIAN_POINT('Ctrl Pts',(0.0683212220377295,-0.780845272715357,
-8.6423904019256));
#67242=CARTESIAN_POINT('Ctrl Pts',(0.434405538413424,-0.654456610012488,
-8.6265038034312));
#67243=CARTESIAN_POINT('Ctrl Pts',(0.692659589757795,-0.366892043313242,
-8.61061720493682));
#67244=CARTESIAN_POINT('Ctrl Pts',(0.818928215962582,0.13728165898334,-8.58943507361095));
#67245=CARTESIAN_POINT('Ctrl Pts',(0.542583354747329,0.628837431876301,
-8.56825294228509));
#67246=CARTESIAN_POINT('Ctrl Pts',(0.0467555812598027,0.781642852722799,
-8.54707081095925));
#67247=CARTESIAN_POINT('Ctrl Pts',(-0.461319991798783,0.689850411348641,
-8.52588867963336));
#67248=CARTESIAN_POINT('Ctrl Pts',(-0.883024702170366,0.120133782328678,
-8.49941101547607));
#67249=CARTESIAN_POINT('Ctrl Pts',(-0.576846771236841,-0.678403874153413,
-8.46763781848726));
#67250=CARTESIAN_POINT('Ctrl Pts',(0.115630535354455,-0.821805114172988,
-8.44116015432995));
#67251=CARTESIAN_POINT('Ctrl Pts',(0.557555887226266,-0.550925187227795,
-8.41997802300409));
#67252=CARTESIAN_POINT('Ctrl Pts',(0.754763984144613,-0.217607340021979,
-8.4040914245097));
#67253=CARTESIAN_POINT('Ctrl Pts',(0.765447231361476,0.168753117692842,
-8.3882048260153));
#67254=CARTESIAN_POINT('Ctrl Pts',(0.535309950887092,0.634769984540963,
-8.36702269468945));
#67255=CARTESIAN_POINT('Ctrl Pts',(0.00647261493553671,0.830536764889757,
-8.34584056336357));
#67256=CARTESIAN_POINT('Ctrl Pts',(-0.470361719928608,0.626028342822735,
-8.32465843203774));
#67257=CARTESIAN_POINT('Ctrl Pts',(-0.798190196393674,0.227161033745103,
-8.30347630071186));
#67258=CARTESIAN_POINT('Ctrl Pts',(-0.750802213668294,-0.480063314835082,
-8.27699863655455));
#67259=CARTESIAN_POINT('Ctrl Pts',(-0.000500919816292827,-0.890496357674791,
-8.24522543956576));
#67260=CARTESIAN_POINT('Ctrl Pts',(0.620130063974467,-0.551518603622994,
-8.21874777540842));
#67261=CARTESIAN_POINT('Ctrl Pts',(0.781606731650396,-0.0589749636832082,
-8.19756564408259));
#67262=CARTESIAN_POINT('Ctrl Pts',(0.716142816035578,0.322739977743579,
-8.18167904558817));
#67263=CARTESIAN_POINT('Ctrl Pts',(0.474174110526119,0.624136196384063,
-8.16579244709379));
#67264=CARTESIAN_POINT('Ctrl Pts',(-0.00291155903197221,0.830350046436369,
-8.14461031576793));
#67265=CARTESIAN_POINT('Ctrl Pts',(-0.532716619424106,0.637217557798746,
-8.12342818444207));
#67266=CARTESIAN_POINT('Ctrl Pts',(-0.763766347841342,0.172663254622042,
-8.10224605311622));
#67267=CARTESIAN_POINT('Ctrl Pts',(-0.755426482980161,-0.343570303843829,
-8.08106392179035));
#67268=CARTESIAN_POINT('Ctrl Pts',(-0.261484402131578,-0.851933481993487,
-8.05458625763304));
#67269=CARTESIAN_POINT('Ctrl Pts',(0.57608317826944,-0.679052417466952,
-8.02281306064424));
#67270=CARTESIAN_POINT('Ctrl Pts',(0.829684344049591,-0.0189197152789447,
-7.99633539648693));
#67271=CARTESIAN_POINT('Ctrl Pts',(0.633911058491592,0.461024835800324,
-7.97515326516106));
#67272=CARTESIAN_POINT('Ctrl Pts',(0.336910971005782,0.70958623423037,-7.95926666666668));
#67273=CARTESIAN_POINT('Ctrl Pts',(-0.0426249265764459,0.782668636374523,
-7.94338006817227));
#67274=CARTESIAN_POINT('Ctrl Pts',(-0.539748277997935,0.631000374953247,
-7.92219793684641));
#67275=CARTESIAN_POINT('Ctrl Pts',(-0.818536045016483,0.14082597624878,
-7.90101580552057));
#67276=CARTESIAN_POINT('Ctrl Pts',(-0.69390967239051,-0.362823648835728,
-7.8798336741947));
#67277=CARTESIAN_POINT('Ctrl Pts',(-0.35336805911191,-0.750893294463733,
-7.85865154286885));
#67278=CARTESIAN_POINT('Ctrl Pts',(0.352200193822944,-0.818608437392834,
-7.83217387871152));
#67279=CARTESIAN_POINT('Ctrl Pts',(0.878671535674212,-0.144638675148288,
-7.80040068172274));
#67280=CARTESIAN_POINT('Ctrl Pts',(0.644625511028497,0.522677737155969,
-7.77392301756541));
#67281=CARTESIAN_POINT('Ctrl Pts',(0.184715642675801,0.761752755592991,
-7.75274088623955));
#67282=CARTESIAN_POINT('Ctrl Pts',(-0.202561919981265,0.758940244529698,
-7.73685428774516));
#67283=CARTESIAN_POINT('Ctrl Pts',(-0.539150765694184,0.568949497390918,
-7.72096768925077));
#67284=CARTESIAN_POINT('Ctrl Pts',(-0.819870802226295,0.131535335365389,
-7.6997855579249));
#67285=CARTESIAN_POINT('Ctrl Pts',(-0.71504469329701,-0.422545026198905,
-7.67860342659905));
#67286=CARTESIAN_POINT('Ctrl Pts',(-0.294016811499463,-0.725744960814242,
-7.65742129527319));
#67287=CARTESIAN_POINT('Ctrl Pts',(0.216758704089238,-0.801077642349773,
-7.63623916394733));
#67288=CARTESIAN_POINT('Ctrl Pts',(0.798371908626541,-0.395938184336486,
-7.60976149979001));
#67289=CARTESIAN_POINT('Ctrl Pts',(0.76334757188336,0.458567877693707,-7.57798830280121));
#67290=CARTESIAN_POINT('Ctrl Pts',(0.152970944928233,0.815680057617568,
-7.5515106386439));
#67291=CARTESIAN_POINT('Ctrl Pts',(-0.352333925525334,0.700177073479672,
-7.53032850731803));
#67292=CARTESIAN_POINT('Ctrl Pts',(-0.645692641308453,0.447328334842996,
-7.51444190882366));
#67293=CARTESIAN_POINT('Ctrl Pts',(-0.779246597900674,0.0846275273786758,
-7.49855531032925));
#67294=CARTESIAN_POINT('Ctrl Pts',(-0.710047714097925,-0.430490325672003,
-7.4773731790034));
#67295=CARTESIAN_POINT('Ctrl Pts',(-0.271464952000793,-0.784945853172596,
-7.45619104767753));
#67296=CARTESIAN_POINT('Ctrl Pts',(0.245715845237475,-0.74348863944973,
-7.43500891635168));
#67297=CARTESIAN_POINT('Ctrl Pts',(0.683791046352098,-0.470254749896074,
-7.41382678502581));
#67298=CARTESIAN_POINT('Ctrl Pts',(0.864823279746207,0.215047541508085,
-7.3873491208685));
#67299=CARTESIAN_POINT('Ctrl Pts',(0.284961482266343,0.843671125248044,
-7.35557592387971));
#67300=CARTESIAN_POINT('Ctrl Pts',(-0.411439412244053,0.720729960831034,
-7.32909825972239));
#67301=CARTESIAN_POINT('Ctrl Pts',(-0.721807007321595,0.305584314852858,
-7.30791612839652));
#67302=CARTESIAN_POINT('Ctrl Pts',(-0.781720082795018,-0.0770411471114446,
-7.29202952990214));
#67303=CARTESIAN_POINT('Ctrl Pts',(-0.64871843548489,-0.439944849034556,
-7.27614293140773));
#67304=CARTESIAN_POINT('Ctrl Pts',(-0.262512891480941,-0.787766880872249,
-7.25496080008189));
#67305=CARTESIAN_POINT('Ctrl Pts',(0.301228506546843,-0.774012015036721,
-7.23377866875602));
#67306=CARTESIAN_POINT('Ctrl Pts',(0.668581532841351,-0.407615465279578,
-7.21259653743016));
#67307=CARTESIAN_POINT('Ctrl Pts',(0.825599807570513,0.0842299389210877,
-7.19141440610431));
#67308=CARTESIAN_POINT('Ctrl Pts',(0.519948814544762,0.723752706767411,
-7.16493674194698));
#67309=CARTESIAN_POINT('Ctrl Pts',(-0.328957522291289,0.82750888966869,
-7.1331635449582));
#67310=CARTESIAN_POINT('Ctrl Pts',(-0.780161627919481,0.282987456805527,
-7.10668588080087));
#67311=CARTESIAN_POINT('Ctrl Pts',(-0.747975418785531,-0.234349956678595,
-7.08550374947501));
#67312=CARTESIAN_POINT('Ctrl Pts',(-0.545947094812301,-0.564768444461357,
-7.06961715098063));
#67313=CARTESIAN_POINT('Ctrl Pts',(-0.209647869942482,-0.755271374645289,
-7.05373055248622));
#67314=CARTESIAN_POINT('Ctrl Pts',(0.309877883978987,-0.770367038374293,
-7.03254842116037));
#67315=CARTESIAN_POINT('Ctrl Pts',(0.730652154624641,-0.394943846033858,
-7.01136628983451));
#67316=CARTESIAN_POINT('Ctrl Pts',(0.773457563384284,0.122127110975526,
-6.99018415850865));
#67317=CARTESIAN_POINT('Ctrl Pts',(0.574738136264083,0.59865332171031,-6.96900202718279));
#67318=CARTESIAN_POINT('Ctrl Pts',(-0.0722228569131348,0.888227791300737,
-6.94252436302547));
#67319=CARTESIAN_POINT('Ctrl Pts',(-0.786418287183742,0.417768227053888,
-6.91075116603668));
#67320=CARTESIAN_POINT('Ctrl Pts',(-0.777824643889002,-0.289349079393862,
-6.88427350187936));
#67321=CARTESIAN_POINT('Ctrl Pts',(-0.418392982781744,-0.662823084436399,
-6.8630913705535));
#67322=CARTESIAN_POINT('Ctrl Pts',(-0.0505116409593437,-0.783881496350488,
-6.84720477205911));
#67323=CARTESIAN_POINT('Ctrl Pts',(0.329135073210841,-0.711376962174498,
-6.83131817356472));
#67324=CARTESIAN_POINT('Ctrl Pts',(0.734885046197271,-0.386566482857896,
-6.81013604223886));
#67325=CARTESIAN_POINT('Ctrl Pts',(0.812564217849937,0.171966870196172,
-6.788953910913));
#67326=CARTESIAN_POINT('Ctrl Pts',(0.510462970451474,0.593783790105791,
-6.76777177958714));
#67327=CARTESIAN_POINT('Ctrl Pts',(0.0505204509556357,0.828346189042659,
-6.74658964826128));
#67328=CARTESIAN_POINT('Ctrl Pts',(-0.630044011076097,0.630245423945558,
-6.72011198410397));
#67329=CARTESIAN_POINT('Ctrl Pts',(-0.869844070319895,-0.190670677634717,
-6.68833878711516));
#67330=CARTESIAN_POINT('Ctrl Pts',(-0.405539972658642,-0.724065878853271,
-6.66186112295786));
#67331=CARTESIAN_POINT('Ctrl Pts',(0.110184840553053,-0.776045378985607,
-6.64067899163198));
#67332=CARTESIAN_POINT('Ctrl Pts',(0.46894807716623,-0.63016611073218,-6.6247923931376));
#67333=CARTESIAN_POINT('Ctrl Pts',(0.711375330090743,-0.329138600511838,
-6.6089057946432));
#67334=CARTESIAN_POINT('Ctrl Pts',(0.810367382881666,0.181092192311117,
-6.58772366331735));
#67335=CARTESIAN_POINT('Ctrl Pts',(0.508005813882541,0.65708698396994,-6.56654153199149));
#67336=CARTESIAN_POINT('Ctrl Pts',(0.00468281360600204,0.783025992947568,
-6.54535940066562));
#67337=CARTESIAN_POINT('Ctrl Pts',(-0.497725690303919,0.664062393222252,
-6.52417726933977));
#67338=CARTESIAN_POINT('Ctrl Pts',(-0.888204658056055,0.0725067595126697,
-6.49769960518244));
#67339=CARTESIAN_POINT('Ctrl Pts',(-0.539556042745298,-0.708423110273319,
-6.46592640819366));
#67340=CARTESIAN_POINT('Ctrl Pts',(0.159626968110726,-0.814403639841095,
-6.43944874403633));
#67341=CARTESIAN_POINT('Ctrl Pts',(0.586356716261186,-0.520166247602953,
-6.41826661271048));
#67342=CARTESIAN_POINT('Ctrl Pts',(0.765367506278367,-0.176732126196868,
-6.40238001421609));
#67343=CARTESIAN_POINT('Ctrl Pts',(0.755272358384135,0.209644083564372,
-6.38649341572169));
#67344=CARTESIAN_POINT('Ctrl Pts',(0.50042423474264,0.662620189055778,-6.36531128439583));
#67345=CARTESIAN_POINT('Ctrl Pts',(-0.0381697288917987,0.82968427820954,
-6.34412915306998));
#67346=CARTESIAN_POINT('Ctrl Pts',(-0.503324291271846,0.599846863125267,
-6.32294702174411));
#67347=CARTESIAN_POINT('Ctrl Pts',(-0.80924501584584,0.183937831155953,
-6.30176489041826));
#67348=CARTESIAN_POINT('Ctrl Pts',(-0.723917441136396,-0.519716397702539,
-6.27528722626094));
#67349=CARTESIAN_POINT('Ctrl Pts',(0.0473522548033906,-0.88923835783592,
-6.24351402927214));
#67350=CARTESIAN_POINT('Ctrl Pts',(0.648876614824445,-0.51739292476347,
-6.21703636511482));
#67351=CARTESIAN_POINT('Ctrl Pts',(0.783640719169264,-0.0168908517885347,
-6.19585423378896));
#67352=CARTESIAN_POINT('Ctrl Pts',(0.697776849956767,0.360768407837624,
-6.17996763529457));
#67353=CARTESIAN_POINT('Ctrl Pts',(0.439924199101702,0.648698474965856,
-6.16408103680018));
#67354=CARTESIAN_POINT('Ctrl Pts',(-0.0474756093028199,0.829034275270768,
-6.14289890547431));
#67355=CARTESIAN_POINT('Ctrl Pts',(-0.566295088878221,0.607590983903843,
-6.12171677414848));
#67356=CARTESIAN_POINT('Ctrl Pts',(-0.771819506095907,0.131460151558091,
-6.10053464282259));
#67357=CARTESIAN_POINT('Ctrl Pts',(-0.73615650740269,-0.383882627307947,
-6.07935251149675));
#67358=CARTESIAN_POINT('Ctrl Pts',(-0.214722507390818,-0.864304610211316,
-6.05287484733942));
#67359=CARTESIAN_POINT('Ctrl Pts',(0.610710452266349,-0.647893193725871,
-6.02110165035064));
#67360=CARTESIAN_POINT('Ctrl Pts',(0.87514783710282,0.161911029797875,-5.98932845336184));
#67361=CARTESIAN_POINT('Ctrl Pts',(0.338210898045152,0.823232838751861,
-5.95755525637307));
#67362=CARTESIAN_POINT('Ctrl Pts',(-0.508641841679914,0.730764205387854,
-5.92578205938427));
#67363=CARTESIAN_POINT('Ctrl Pts',(-0.889979875388079,-0.0326195618755111,
-5.89400886239549));
#67364=CARTESIAN_POINT('Ctrl Pts',(-0.526901538696912,-0.641612845459792,
-5.86753119823816));
#67365=CARTESIAN_POINT('Ctrl Pts',(-0.0298714672499406,-0.782364887301405,
-5.84634906691231));
#67366=CARTESIAN_POINT('Ctrl Pts',(0.47832166267773,-0.679017907291142,
-5.82516693558643));
#67367=CARTESIAN_POINT('Ctrl Pts',(0.801607061401948,-0.216743816896674,
-5.8039848042606));
#67368=CARTESIAN_POINT('Ctrl Pts',(0.725226253928277,0.297304377686334,
-5.78280267293472));
#67369=CARTESIAN_POINT('Ctrl Pts',(0.496397105934749,0.608799055229958,
-5.76691607444034));
#67370=CARTESIAN_POINT('Ctrl Pts',(0.144426057203333,0.770401967556523,
-5.75102947594594));
#67371=CARTESIAN_POINT('Ctrl Pts',(-0.373084797124373,0.741312372766026,
-5.72984734462008));
#67372=CARTESIAN_POINT('Ctrl Pts',(-0.860552864376412,0.228988778535637,
-5.70336968046277));
#67373=CARTESIAN_POINT('Ctrl Pts',(-0.657325329301909,-0.601734997387143,
-5.67159648347396));
#67374=CARTESIAN_POINT('Ctrl Pts',(0.0138002762959166,-0.829771157474066,
-5.64511881931665));
#67375=CARTESIAN_POINT('Ctrl Pts',(0.483676613599726,-0.615799102664358,
-5.62393668799079));
#67376=CARTESIAN_POINT('Ctrl Pts',(0.804154597478065,-0.20776985601056,
-5.60275455666493));
#67377=CARTESIAN_POINT('Ctrl Pts',(0.751277615728742,0.353655020842358,
-5.58157242533908));
#67378=CARTESIAN_POINT('Ctrl Pts',(0.360304271057673,0.69610904991264,-5.56039029401322));
#67379=CARTESIAN_POINT('Ctrl Pts',(-0.0157604757935807,0.785349139873212,
-5.54450369551882));
#67380=CARTESIAN_POINT('Ctrl Pts',(-0.388640335473441,0.680695095834419,
-5.52861709702443));
#67381=CARTESIAN_POINT('Ctrl Pts',(-0.764252910898822,0.323498911462347,
-5.50743496569857));
#67382=CARTESIAN_POINT('Ctrl Pts',(-0.804141491407507,-0.382544753237058,
-5.48095730154125));
#67383=CARTESIAN_POINT('Ctrl Pts',(-0.111472970044356,-0.884159782910866,
-5.44918410455246));
#67384=CARTESIAN_POINT('Ctrl Pts',(0.547672930190298,-0.623509491842228,
-5.42270644039513));
#67385=CARTESIAN_POINT('Ctrl Pts',(0.767292864059844,-0.156247544421139,
-5.40152430906929));
#67386=CARTESIAN_POINT('Ctrl Pts',(0.74741961163729,0.362211451477082,-5.38034217774341));
#67387=CARTESIAN_POINT('Ctrl Pts',(0.34367744228227,0.755893837136436,-5.35916004641757));
#67388=CARTESIAN_POINT('Ctrl Pts',(-0.176007263809187,0.76381183657692,
-5.3379779150917));
#67389=CARTESIAN_POINT('Ctrl Pts',(-0.520410163705834,0.588383282992382,
-5.32209131659731));
#67390=CARTESIAN_POINT('Ctrl Pts',(-0.736867711719661,0.267232304854123,
-5.30620471810292));
#67391=CARTESIAN_POINT('Ctrl Pts',(-0.791924355942771,-0.248173086389637,
-5.28502258677705));
#67392=CARTESIAN_POINT('Ctrl Pts',(-0.365267985880006,-0.812135033397483,
-5.25854492261974));
#67393=CARTESIAN_POINT('Ctrl Pts',(0.487399303105791,-0.74606076805389,
-5.22677172563095));
#67394=CARTESIAN_POINT('Ctrl Pts',(0.821061658291666,-0.120695808334838,
-5.20029406147362));
#67395=CARTESIAN_POINT('Ctrl Pts',(0.685970800776325,0.377618450392495,
-5.17911193014777));
#67396=CARTESIAN_POINT('Ctrl Pts',(0.335197903320081,0.759918139134054,
-5.1579297988219));
#67397=CARTESIAN_POINT('Ctrl Pts',(-0.227381916708832,0.798615765401183,
-5.13674766749606));
#67398=CARTESIAN_POINT('Ctrl Pts',(-0.628606563135292,0.468231638735957,
-5.11556553617019));
#67399=CARTESIAN_POINT('Ctrl Pts',(-0.777543191380457,0.111571554309256,
-5.0996789376758));
#67400=CARTESIAN_POINT('Ctrl Pts',(-0.734627282762826,-0.273331089931772,
-5.0837923391814));
#67401=CARTESIAN_POINT('Ctrl Pts',(-0.442942022564239,-0.701809397937808,
-5.06261020785555));
#67402=CARTESIAN_POINT('Ctrl Pts',(0.24733367727714,-0.855458979751414,
-5.03613254369822));
#67403=CARTESIAN_POINT('Ctrl Pts',(0.854455518574205,-0.253121546055969,
-5.00435934670944));
#67404=CARTESIAN_POINT('Ctrl Pts',(0.703938379568512,0.439523017191998,
-4.97788168255211));
#67405=CARTESIAN_POINT('Ctrl Pts',(0.278388425828125,0.731882174913778,
-4.95669955122626));
#67406=CARTESIAN_POINT('Ctrl Pts',(-0.236450085029051,0.796193801701192,
-4.93551741990039));
#67407=CARTESIAN_POINT('Ctrl Pts',(-0.690294259443345,0.461501367465407,
-4.91433528857454));
#67408=CARTESIAN_POINT('Ctrl Pts',(-0.782229035346391,-0.0500481267487367,
-4.89315315724868));
#67409=CARTESIAN_POINT('Ctrl Pts',(-0.664862395795767,-0.418305654814762,
-4.87726655875428));
#67410=CARTESIAN_POINT('Ctrl Pts',(-0.382984625029711,-0.683893198016694,
-4.8613799602599));
#67411=CARTESIAN_POINT('Ctrl Pts',(0.11671167241904,-0.821652269459763,
-4.84019782893403));
#67412=CARTESIAN_POINT('Ctrl Pts',(0.742298900655215,-0.491910922869968,
-4.81372016477672));
#67413=CARTESIAN_POINT('Ctrl Pts',(0.815116995369976,0.36020693241341,-4.78194696778791));
#67414=CARTESIAN_POINT('Ctrl Pts',(0.252009078067586,0.790696622885568,
-4.75546930363061));
#67415=CARTESIAN_POINT('Ctrl Pts',(-0.261600597687866,0.738049294343494,
-4.73428717230474));
#67416=CARTESIAN_POINT('Ctrl Pts',(-0.695638069988528,0.453785068242976,
-4.71310504097889));
#67417=CARTESIAN_POINT('Ctrl Pts',(-0.824889973540065,-0.0951115573731555,
-4.69192290965302));
#67418=CARTESIAN_POINT('Ctrl Pts',(-0.563809010906991,-0.544524083902708,
-4.67074077832718));
#67419=CARTESIAN_POINT('Ctrl Pts',(-0.235960833039409,-0.749229011360774,
-4.65485417983276));
#67420=CARTESIAN_POINT('Ctrl Pts',(0.150812554763246,-0.769183139849302,
-4.63896758133839));
#67421=CARTESIAN_POINT('Ctrl Pts',(0.620855152320868,-0.550702230087972,
-4.61778545001251));
#67422=CARTESIAN_POINT('Ctrl Pts',(0.884213132850611,0.105599004006847,
-4.5913077858552));
#67423=CARTESIAN_POINT('Ctrl Pts',(0.388093857664531,0.802214377796061,
-4.5595345888664));
#67424=CARTESIAN_POINT('Ctrl Pts',(-0.319780369690156,0.765800391767949,
-4.53305692470909));
#67425=CARTESIAN_POINT('Ctrl Pts',(-0.677167572045297,0.393186613406222,
-4.51187479338323));
#67426=CARTESIAN_POINT('Ctrl Pts',(-0.823967811864189,-0.104452178480815,
-4.49069266205737));
#67427=CARTESIAN_POINT('Ctrl Pts',(-0.567152865214582,-0.606487678581986,
-4.46951053073151));
#67428=CARTESIAN_POINT('Ctrl Pts',(-0.077231065227596,-0.780014385312101,
-4.44832839940566));
#67429=CARTESIAN_POINT('Ctrl Pts',(0.305168035875328,-0.723805288785105,
-4.43244180091126));
#67430=CARTESIAN_POINT('Ctrl Pts',(0.612880513490481,-0.488635452547494,
-4.41655520241687));
#67431=CARTESIAN_POINT('Ctrl Pts',(0.829708518342342,-0.0178280951699618,
-4.395373071091));
#67432=CARTESIAN_POINT('Ctrl Pts',(0.605579358449078,0.652884105008795,
-4.36889540693369));
#67433=CARTESIAN_POINT('Ctrl Pts',(-0.223513846984806,0.862673930581949,
-4.33712220994489));
#67434=CARTESIAN_POINT('Ctrl Pts',(-0.739476400119356,0.376675428635363,
-4.31064454578758));
#67435=CARTESIAN_POINT('Ctrl Pts',(-0.770661211393977,-0.138682842645893,
-4.28946241446172));
#67436=CARTESIAN_POINT('Ctrl Pts',(-0.560403328348306,-0.613010050614006,
-4.26828028313586));
#67437=CARTESIAN_POINT('Ctrl Pts',(-0.0396674371228205,-0.829407120312446,
-4.24709815181));
#67438=CARTESIAN_POINT('Ctrl Pts',(0.446079393600652,-0.644515518304158,
-4.22591602048414));
#67439=CARTESIAN_POINT('Ctrl Pts',(0.701153381813063,-0.354126476510017,
-4.21002942198975));
#67440=CARTESIAN_POINT('Ctrl Pts',(0.783451243037709,0.0243162309027824,
-4.19414282349535));
#67441=CARTESIAN_POINT('Ctrl Pts',(0.643937273529952,0.523525409264962,
-4.1729606921695));
#67442=CARTESIAN_POINT('Ctrl Pts',(0.0389209183077788,0.889645533946421,
-4.14648302801217));
#67443=CARTESIAN_POINT('Ctrl Pts',(-0.728814260660947,0.512829916987002,
-4.11470983102339));
#67444=CARTESIAN_POINT('Ctrl Pts',(-0.807463872462469,-0.191603286869062,
-4.08823216686606));
#67445=CARTESIAN_POINT('Ctrl Pts',(-0.497614223633389,-0.604592191505413,
-4.06705003554021));
#67446=CARTESIAN_POINT('Ctrl Pts',(-0.030300728770561,-0.830009083331993,
-4.04586790421435));
#67447=CARTESIAN_POINT('Ctrl Pts',(0.506684552648503,-0.657845301647932,
-4.02468577288849));
#67448=CARTESIAN_POINT('Ctrl Pts',(0.757226299555704,-0.202473232777027,
-4.00350364156263));
#67449=CARTESIAN_POINT('Ctrl Pts',(0.76365730106179,0.18398139234257,-3.98761704306824));
#67450=CARTESIAN_POINT('Ctrl Pts',(0.581398171507507,0.52570266831202,-3.97173044457384));
#67451=CARTESIAN_POINT('Ctrl Pts',(0.1518976340338,0.815880613302076,-3.95054831324798));
#67452=CARTESIAN_POINT('Ctrl Pts',(-0.546249025453097,0.703275206547391,
-3.92407064909066));
#67453=CARTESIAN_POINT('Ctrl Pts',(-0.8874772256122,-0.0809254244309511,
-3.89229745210188));
#67454=CARTESIAN_POINT('Ctrl Pts',(-0.491406696126427,-0.668751959902339,
-3.86581978794455));
#67455=CARTESIAN_POINT('Ctrl Pts',(0.0121072287199249,-0.782946389355173,
-3.8446376566187));
#67456=CARTESIAN_POINT('Ctrl Pts',(0.514213453953207,-0.652240550986492,
-3.82345552529283));
#67457=CARTESIAN_POINT('Ctrl Pts',(0.812048062749978,-0.173400174673731,
-3.80227339396698));
#67458=CARTESIAN_POINT('Ctrl Pts',(0.708222469234925,0.335869041146677,
-3.78109126264112));
#67459=CARTESIAN_POINT('Ctrl Pts',(0.462951781598219,0.634584331754523,
-3.76520466414672));
#67460=CARTESIAN_POINT('Ctrl Pts',(0.102821450890194,0.777055260930318,
-3.74931806565233));
#67461=CARTESIAN_POINT('Ctrl Pts',(-0.412387310159186,0.72018801212385,
-3.72813593432647));
#67462=CARTESIAN_POINT('Ctrl Pts',(-0.871612899585501,0.182414273643501,
-3.70165827016915));
#67463=CARTESIAN_POINT('Ctrl Pts',(-0.624039721496535,-0.636191147607529,
-3.66988507318036));
#67464=CARTESIAN_POINT('Ctrl Pts',(0.0583725307045223,-0.827829917634214,
-3.64340740902304));
#67465=CARTESIAN_POINT('Ctrl Pts',(0.516070260716903,-0.588916903811706,
-3.62222527769718));
#67466=CARTESIAN_POINT('Ctrl Pts',(0.814158273260994,-0.164254432690011,
-3.60104314637132));
#67467=CARTESIAN_POINT('Ctrl Pts',(0.731186599072323,0.393517260269395,
-3.57986101504547));
#67468=CARTESIAN_POINT('Ctrl Pts',(0.322375024407198,0.714465830091588,
-3.5586788837196));
#67469=CARTESIAN_POINT('Ctrl Pts',(-0.057942108370507,0.78336730737941,
-3.54279228522521));
#67470=CARTESIAN_POINT('Ctrl Pts',(-0.424659040323523,0.658826099038399,
-3.52690568673082));
#67471=CARTESIAN_POINT('Ctrl Pts',(-0.780533275196529,0.281960764465941,
-3.50572355540496));
#67472=CARTESIAN_POINT('Ctrl Pts',(-0.782421669494201,-0.425206238264019,
-3.47924589124764));
#67473=CARTESIAN_POINT('Ctrl Pts',(-0.0637974639085965,-0.888872675864485,
-3.44747269425885));
#67474=CARTESIAN_POINT('Ctrl Pts',(0.580388709786245,-0.593176761533836,
-3.42099503010153));
#67475=CARTESIAN_POINT('Ctrl Pts',(0.774580797896507,-0.114787721998427,
-3.39981289877567));
#67476=CARTESIAN_POINT('Ctrl Pts',(0.726874463911719,0.401854110705244,
-3.37863076744981));
#67477=CARTESIAN_POINT('Ctrl Pts',(0.302559358947867,0.773270658376436,
-3.35744863612395));
#67478=CARTESIAN_POINT('Ctrl Pts',(-0.21679990318929,0.753249547432401,
-3.3362665047981));
#67479=CARTESIAN_POINT('Ctrl Pts',(-0.551277667357786,0.559566403267617,
-3.3203799063037));
#67480=CARTESIAN_POINT('Ctrl Pts',(-0.750163892116854,0.227247143583241,
-3.30449330780931));
#67481=CARTESIAN_POINT('Ctrl Pts',(-0.777443278256896,-0.290372201631635,
-3.28331117648345));
#67482=CARTESIAN_POINT('Ctrl Pts',(-0.321096322413234,-0.830590853360081,
-3.25683351232612));
#67483=CARTESIAN_POINT('Ctrl Pts',(0.526788039301812,-0.718790033283858,
-3.22506031533735));
#67484=CARTESIAN_POINT('Ctrl Pts',(0.826361358316619,-0.0763978425888647,
-3.19858265118));
#67485=CARTESIAN_POINT('Ctrl Pts',(0.664686480633999,0.413936608738543,
-3.17740051985416));
#67486=CARTESIAN_POINT('Ctrl Pts',(0.293875808800309,0.77683345807168,-3.15621838852829));
#67487=CARTESIAN_POINT('Ctrl Pts',(-0.269970669492542,0.785242328460858,
-3.13503625720245));
#67488=CARTESIAN_POINT('Ctrl Pts',(-0.652860814798813,0.433773944849426,
-3.11385412587658));
#67489=CARTESIAN_POINT('Ctrl Pts',(-0.782415442264087,0.0696254400343804,
-3.09796752738219));
#67490=CARTESIAN_POINT('Ctrl Pts',(-0.718877018329645,-0.312414727277906,
-3.08208092888779));
#67491=CARTESIAN_POINT('Ctrl Pts',(-0.404586978639708,-0.724598815278104,
-3.06089879756194));
#67492=CARTESIAN_POINT('Ctrl Pts',(0.292948333281876,-0.840931202881724,
-3.03442113340461));
#67493=CARTESIAN_POINT('Ctrl Pts',(0.866823475343164,-0.206837648636938,
-3.00264793641582));
#67494=CARTESIAN_POINT('Ctrl Pts',(0.679301366799664,0.476717293513901,
-2.9761702722585));
#67495=CARTESIAN_POINT('Ctrl Pts',(0.238655064681991,0.745785085459083,
-2.95498814093265));
#67496=CARTESIAN_POINT('Ctrl Pts',(-0.27889557868341,0.782336544441392,
-2.93380600960678));
#67497=CARTESIAN_POINT('Ctrl Pts',(-0.714097688888377,0.423738324343162,
-2.91262387828093));
#67498=CARTESIAN_POINT('Ctrl Pts',(-0.778409131595645,-0.0920125131626953,
-2.89144174695507));
#67499=CARTESIAN_POINT('Ctrl Pts',(-0.641422061965753,-0.45343066131097,
-2.87555514846067));
#67500=CARTESIAN_POINT('Ctrl Pts',(-0.345679030790674,-0.703486415628807,
-2.85966854996628));
#67501=CARTESIAN_POINT('Ctrl Pts',(0.160698319191389,-0.814192923450146,
-2.83848641864043));
#67502=CARTESIAN_POINT('Ctrl Pts',(0.767661380996447,-0.451309226672089,
-2.8120087544831));
#67503=CARTESIAN_POINT('Ctrl Pts',(0.794581745299286,0.403490520752094,
-2.78023555749431));
#67504=CARTESIAN_POINT('Ctrl Pts',(0.209153168296713,0.803096928809075,
-2.75375789333699));
#67505=CARTESIAN_POINT('Ctrl Pts',(-0.300885083483398,0.722924477472416,
-2.73257576201113));
#67506=CARTESIAN_POINT('Ctrl Pts',(-0.719019106384883,0.415746000860054,
-2.71139363068527));
#67507=CARTESIAN_POINT('Ctrl Pts',(-0.818586731398151,-0.139303409763623,
-2.69021149935941));
#67508=CARTESIAN_POINT('Ctrl Pts',(-0.533731768126874,-0.574036129892679,
-2.66902936803356));
#67509=CARTESIAN_POINT('Ctrl Pts',(-0.195356567801208,-0.76082681183711,
-2.65314276953916));
#67510=CARTESIAN_POINT('Ctrl Pts',(0.191930252984854,-0.759967043556375,
-2.63725617104477));
#67511=CARTESIAN_POINT('Ctrl Pts',(0.649552544819839,-0.516541922698741,
-2.61607403971891));
#67512=CARTESIAN_POINT('Ctrl Pts',(0.877260576037617,0.152963707077457,
-2.58959637556159));
#67513=CARTESIAN_POINT('Ctrl Pts',(0.344422342865012,0.82191118743757,-2.5578231785728));
#67514=CARTESIAN_POINT('Ctrl Pts',(-0.360472118628379,0.747508914035598,
-2.53134551441547));
#67515=CARTESIAN_POINT('Ctrl Pts',(-0.69731875949566,0.356227709824785,
-2.51016338308962));
#67516=CARTESIAN_POINT('Ctrl Pts',(-0.817163940645753,-0.148580976864318,
-2.48898125176376));
#67517=CARTESIAN_POINT('Ctrl Pts',(-0.533740889221978,-0.636089883558451,
-2.4677991204379));
#67518=CARTESIAN_POINT('Ctrl Pts',(-0.0352017725222705,-0.783037619748434,
-2.44661698911204));
#67519=CARTESIAN_POINT('Ctrl Pts',(0.343624098183447,-0.706359756314665,
-2.43073039061765));
#67520=CARTESIAN_POINT('Ctrl Pts',(0.638253983199123,-0.454993387021286,
-2.41484379212325));
#67521=CARTESIAN_POINT('Ctrl Pts',(0.829467649601628,0.0267859039717638,
-2.3936616607974));
#67522=CARTESIAN_POINT('Ctrl Pts',(0.569618528201855,0.68448429220975,-2.36718399664007));
#67523=CARTESIAN_POINT('Ctrl Pts',(-0.269550651946428,0.849415797083451,
-2.33541079965129));
#67524=CARTESIAN_POINT('Ctrl Pts',(-0.758650245032131,0.336391930021827,
-2.30893313549396));
#67525=CARTESIAN_POINT('Ctrl Pts',(-0.762094825624762,-0.179897499558888,
-2.28775100416811));
#67526=CARTESIAN_POINT('Ctrl Pts',(-0.526650595635342,-0.642240112959774,
-2.26656887284225));
#67527=CARTESIAN_POINT('Ctrl Pts',(0.00496192325041732,-0.830340325475366,
-2.24538674151639));
#67528=CARTESIAN_POINT('Ctrl Pts',(0.480070832655676,-0.619612035360264,
-2.22420461019054));
#67529=CARTESIAN_POINT('Ctrl Pts',(0.719170831623089,-0.315935026763165,
-2.20831801169613));
#67530=CARTESIAN_POINT('Ctrl Pts',(0.781012395997661,0.066383481383875,
-2.19243141320175));
#67531=CARTESIAN_POINT('Ctrl Pts',(0.614872705146752,0.55737386272838,-2.17124928187588));
#67532=CARTESIAN_POINT('Ctrl Pts',(-0.00894455400451892,0.890451575834638,
-2.14477161771857));
#67533=CARTESIAN_POINT('Ctrl Pts',(-0.75532040577284,0.472922652156577,
-2.11299842072978));
#67534=CARTESIAN_POINT('Ctrl Pts',(-0.796000380537386,-0.234719234523823,
-2.08652075657245));
#67535=CARTESIAN_POINT('Ctrl Pts',(-0.46440459505787,-0.630460153919906,
-2.06533862524659));
#67536=CARTESIAN_POINT('Ctrl Pts',(0.01434744581186,-0.830438055110873,
-2.04415649392074));
#67537=CARTESIAN_POINT('Ctrl Pts',(0.541304753887728,-0.629665657481347,
-2.02297436259488));
#67538=CARTESIAN_POINT('Ctrl Pts',(0.767012932214679,-0.161487586350912,
-2.00179223126902));
#67539=CARTESIAN_POINT('Ctrl Pts',(0.75266670831207,0.224754204392204,-1.98590563277462));
#67540=CARTESIAN_POINT('Ctrl Pts',(0.55230696816604,0.556187146757173,-1.97001903428023));
#67541=CARTESIAN_POINT('Ctrl Pts',(0.107833008568935,0.822864574915098,
-1.94883690295438));
#67542=CARTESIAN_POINT('Ctrl Pts',(-0.583253442038985,0.672903734796001,
-1.92235923879705));
#67543=CARTESIAN_POINT('Ctrl Pts',(-0.881845901412668,-0.128501192451031,
-1.89058604180827));
#67544=CARTESIAN_POINT('Ctrl Pts',(-0.454758114676497,-0.694193619969962,
-1.86410837765094));
#67545=CARTESIAN_POINT('Ctrl Pts',(0.0541649907798706,-0.781164379222065,
-1.84292624632508));
#67546=CARTESIAN_POINT('Ctrl Pts',(0.548521578507037,-0.623664405341359,
-1.82174411499922));
#67547=CARTESIAN_POINT('Ctrl Pts',(0.820193101266005,-0.129510437527382,
-1.80056198367337));
#67548=CARTESIAN_POINT('Ctrl Pts',(0.689149593251153,0.373443324818871,
-1.77937985234751));
#67549=CARTESIAN_POINT('Ctrl Pts',(0.428180474068072,0.658546207809391,
-1.76349325385311));
#67550=CARTESIAN_POINT('Ctrl Pts',(0.0609142018835925,0.781457989473221,
-1.74760665535872));
#67551=CARTESIAN_POINT('Ctrl Pts',(-0.45049404748608,0.696985781466766,
-1.72642452403286));
#67552=CARTESIAN_POINT('Ctrl Pts',(-0.880156280245255,0.135310518059632,
-1.69994685987554));
#67553=CARTESIAN_POINT('Ctrl Pts',(-0.588949289207153,-0.668807509708173,
-1.66817366288675));
#67554=CARTESIAN_POINT('Ctrl Pts',(0.102775463205937,-0.823496769291736,
-1.64169599872943));
#67555=CARTESIAN_POINT('Ctrl Pts',(0.546972712137699,-0.56033247788104,
-1.62051386740357));
#67556=CARTESIAN_POINT('Ctrl Pts',(0.821808773600565,-0.120264509356574,
-1.59933173607771));
#67557=CARTESIAN_POINT('Ctrl Pts',(0.708982544944508,0.432242325272397,
-1.57814960475185));
#67558=CARTESIAN_POINT('Ctrl Pts',(0.283514049915959,0.730757731556947,
-1.556967473426));
#67559=CARTESIAN_POINT('Ctrl Pts',(-0.0999562581644404,0.779121539072725,
-1.5410808749316));
#67560=CARTESIAN_POINT('Ctrl Pts',(-0.459450477644474,0.63505305911783,
-1.52519427643721));
#67561=CARTESIAN_POINT('Ctrl Pts',(-0.79455786019474,0.239607748601739,
-1.50401214511135));
#67562=CARTESIAN_POINT('Ctrl Pts',(-0.758440625467195,-0.466638866355624,
-1.47753448095403));
#67563=CARTESIAN_POINT('Ctrl Pts',(-0.0159375776428949,-0.891016691155971,
-1.44576128396524));
#67564=CARTESIAN_POINT('Ctrl Pts',(0.611427143079269,-0.561129729721242,
-1.41928361980792));
#67565=CARTESIAN_POINT('Ctrl Pts',(0.779630165187704,-0.0729961582617228,
-1.39810148848206));
#67566=CARTESIAN_POINT('Ctrl Pts',(0.704228621556494,0.440335396213263,
-1.3769193571562));
#67567=CARTESIAN_POINT('Ctrl Pts',(0.260566868148073,0.788412699045606,
-1.35573722583034));
#67568=CARTESIAN_POINT('Ctrl Pts',(-0.256965982948583,0.740510339115715,
-1.33455509450448));
#67569=CARTESIAN_POINT('Ctrl Pts',(-0.580551958086807,0.529132355989381,
-1.31866849601009));
#67570=CARTESIAN_POINT('Ctrl Pts',(-0.761292071137348,0.186605229632119,
-1.3027818975157));
#67571=CARTESIAN_POINT('Ctrl Pts',(-0.76071536070743,-0.331732130447139,
-1.28159976618984));
#67572=CARTESIAN_POINT('Ctrl Pts',(-0.275996678705884,-0.846646235033293,
-1.25512210203252));
#67573=CARTESIAN_POINT('Ctrl Pts',(0.564654338578688,-0.689441968713772,
-1.22334890504373));
#67574=CARTESIAN_POINT('Ctrl Pts',(0.829272843434691,-0.0318790842538621,
-1.19687124088641));
#67575=CARTESIAN_POINT('Ctrl Pts',(0.641481191968628,0.44905847496967,-1.17568910956055));
#67576=CARTESIAN_POINT('Ctrl Pts',(0.251704402317549,0.791503699569123,
-1.15450697823469));
#67577=CARTESIAN_POINT('Ctrl Pts',(-0.311779197051007,0.769599512135441,
-1.13332484690883));
#67578=CARTESIAN_POINT('Ctrl Pts',(-0.675228274549961,0.398062628211048,
-1.11214271558297));
#67579=CARTESIAN_POINT('Ctrl Pts',(-0.785026483567616,0.0274781056615818,
-1.09625611708858));
#67580=CARTESIAN_POINT('Ctrl Pts',(-0.70104917271287,-0.350595474501956,
-1.08036951859419));
#67581=CARTESIAN_POINT('Ctrl Pts',(-0.365062663375868,-0.745294115229794,
-1.05918738726832));
#67582=CARTESIAN_POINT('Ctrl Pts',(0.337716357763391,-0.823973103718647,
-1.032709723111));
#67583=CARTESIAN_POINT('Ctrl Pts',(0.876686280193239,-0.15995598275971,
-1.00093652612222));
#67584=CARTESIAN_POINT('Ctrl Pts',(0.652701147944472,0.512533839217553,
-0.974458861964892));
#67585=CARTESIAN_POINT('Ctrl Pts',(0.198231981567963,0.75753264951101,-0.953276730639035));
#67586=CARTESIAN_POINT('Ctrl Pts',(-0.320535053795434,0.766218305619351,
-0.932094599313175));
#67587=CARTESIAN_POINT('Ctrl Pts',(-0.735837349588571,0.384750661783734,
-0.910912467987319));
#67588=CARTESIAN_POINT('Ctrl Pts',(-0.772339596651168,-0.133710980008637,
-0.889730336661458));
#67589=CARTESIAN_POINT('Ctrl Pts',(-0.616127994641744,-0.487245236418133,
-0.873843738167066));
#67590=CARTESIAN_POINT('Ctrl Pts',(-0.307374411361996,-0.721046531467661,
-0.85795713967267));
#67591=CARTESIAN_POINT('Ctrl Pts',(0.20422054187608,-0.80438052976603,-0.836775008346816));
#67592=CARTESIAN_POINT('Ctrl Pts',(0.790805291538328,-0.409403230105263,
-0.810297344189487));
#67593=CARTESIAN_POINT('Ctrl Pts',(0.771750124586875,0.445608006548333,
-0.778524147200705));
#67594=CARTESIAN_POINT('Ctrl Pts',(0.165692798123157,0.813176254903035,
-0.752046483043378));
#67595=CARTESIAN_POINT('Ctrl Pts',(-0.33930000024461,0.705710382095269,
-0.730864351717522));
#67596=CARTESIAN_POINT('Ctrl Pts',(-0.740322150981868,0.376505412191275,
-0.709682220391663));
#67597=CARTESIAN_POINT('Ctrl Pts',(-0.809917743263348,-0.183092670227531,
-0.688500089065804));
#67598=CARTESIAN_POINT('Ctrl Pts',(-0.502112020847565,-0.601889190124352,
-0.667317957739947));
#67599=CARTESIAN_POINT('Ctrl Pts',(-0.154187714727574,-0.770225794886024,
-0.651431359245553));
#67600=CARTESIAN_POINT('Ctrl Pts',(0.232493265444015,-0.748554614000191,
-0.635544760751159));
#67601=CARTESIAN_POINT('Ctrl Pts',(0.676372706924209,-0.480888790873769,
-0.614362629425302));
#67602=CARTESIAN_POINT('Ctrl Pts',(0.86777270267367,0.199886341100763,-0.587884965267977));
#67603=CARTESIAN_POINT('Ctrl Pts',(0.299755436540123,0.839232640318567,
-0.556111768279191));
#67604=CARTESIAN_POINT('Ctrl Pts',(-0.400122092807645,0.72705711293915,
-0.529634104121868));
#67605=CARTESIAN_POINT('Ctrl Pts',(-0.715454665930561,0.318239288246659,
-0.508451972796009));
#67606=CARTESIAN_POINT('Ctrl Pts',(-0.807998445695184,-0.192280353386799,
-0.487269841470152));
#67607=CARTESIAN_POINT('Ctrl Pts',(-0.498786361378514,-0.663853800491803,
-0.466087710144292));
#67608=CARTESIAN_POINT('Ctrl Pts',(0.00692922874373258,-0.783797802920765,
-0.444905578818435));
#67609=CARTESIAN_POINT('Ctrl Pts',(0.381087127953349,-0.686872908670706,
-0.429018980324039));
#67610=CARTESIAN_POINT('Ctrl Pts',(0.661782777111213,-0.420036208409248,
-0.413132381829648));
#67611=CARTESIAN_POINT('Ctrl Pts',(0.826829800764357,0.0713221335761503,
-0.391950250503787));
#67612=CARTESIAN_POINT('Ctrl Pts',(0.532011040561915,0.714107033573504,
-0.365472586346466));
#67613=CARTESIAN_POINT('Ctrl Pts',(-0.314807679105772,0.833701529443594,
-0.333699389357678));
#67614=CARTESIAN_POINT('Ctrl Pts',(-0.775632848136392,0.295138411630498,
-0.307221725200355));
#67615=CARTESIAN_POINT('Ctrl Pts',(-0.751324246115917,-0.220595129012272,
-0.286039593874496));
#67616=CARTESIAN_POINT('Ctrl Pts',(-0.491380230422849,-0.669606653773286,
-0.264857462548639));
#67617=CARTESIAN_POINT('Ctrl Pts',(0.0495859047765307,-0.828888911462718,
-0.243675331222779));
#67618=CARTESIAN_POINT('Ctrl Pts',(0.512663775722113,-0.592899197626148,
-0.222493199896921));
#67619=CARTESIAN_POINT('Ctrl Pts',(0.735132893747708,-0.27686932786066,
-0.206606601402529));
#67620=CARTESIAN_POINT('Ctrl Pts',(0.776274364779559,0.108329678724445,
-0.190720002908133));
#67621=CARTESIAN_POINT('Ctrl Pts',(0.584121944633851,0.58945851373242,-0.169537871582277));
#67622=CARTESIAN_POINT('Ctrl Pts',(-0.0569720689210273,0.889000674187564,
-0.143060207424953));
#67623=CARTESIAN_POINT('Ctrl Pts',(-0.779315258188735,0.431095499374008,
-0.111287010436167));
#67624=CARTESIAN_POINT('Ctrl Pts',(-0.782788362817514,-0.276227349621032,
-0.0848093462788417));
#67625=CARTESIAN_POINT('Ctrl Pts',(-0.429109244619801,-0.655756861746561,
-0.0636272149529857));
#67626=CARTESIAN_POINT('Ctrl Pts',(-0.0646184054315698,-0.782693153117636,
-0.0477406164585894));
#67627=CARTESIAN_POINT('Ctrl Pts',(0.318892419761328,-0.717280333622648,
-0.0318540179641984));
#67628=CARTESIAN_POINT('Ctrl Pts',(0.521380142127114,-0.557506295451278,
-0.021262952301267));
#67629=CARTESIAN_POINT('Ctrl Pts',(0.597589667152271,-0.458088845993819,
-0.0159674194698027));
#67630=CARTESIAN_POINT('Ctrl Pts',(-0.34206796250955,0.713322310757602,
-11.9089));
#67631=CARTESIAN_POINT('Ctrl Pts',(-0.46073916563555,0.656414492160488,
-11.9036044671685));
#67632=CARTESIAN_POINT('Ctrl Pts',(-0.668722237093865,0.482686815406386,
-11.8930134015056));
#67633=CARTESIAN_POINT('Ctrl Pts',(-0.818743490259774,0.102460369625847,
-11.8771268030112));
#67634=CARTESIAN_POINT('Ctrl Pts',(-0.766878588870734,-0.299717504486475,
-11.8612402045168));
#67635=CARTESIAN_POINT('Ctrl Pts',(-0.452953262747085,-0.745287473216968,
-11.840058073191));
#67636=CARTESIAN_POINT('Ctrl Pts',(0.275096172417156,-0.894355306323675,
-11.8135804090336));
#67637=CARTESIAN_POINT('Ctrl Pts',(0.901814470278374,-0.250425930665646,
-11.7818072120449));
#67638=CARTESIAN_POINT('Ctrl Pts',(0.732159228641372,0.473415334142076,
-11.7553295478875));
#67639=CARTESIAN_POINT('Ctrl Pts',(0.278907906557356,0.77482152142975,-11.7341474165617));
#67640=CARTESIAN_POINT('Ctrl Pts',(-0.126048629243606,0.815643351149952,
-11.7182608180673));
#67641=CARTESIAN_POINT('Ctrl Pts',(-0.499012654979741,0.655089673413841,
-11.7023742195729));
#67642=CARTESIAN_POINT('Ctrl Pts',(-0.841598877251412,0.229859144335204,
-11.681192088247));
#67643=CARTESIAN_POINT('Ctrl Pts',(-0.794557513494638,-0.360758464515903,
-11.6600099569212));
#67644=CARTESIAN_POINT('Ctrl Pts',(-0.388959906239125,-0.724940043166852,
-11.6388278255953));
#67645=CARTESIAN_POINT('Ctrl Pts',(0.136093872237789,-0.861229592104873,
-11.6176456942695));
#67646=CARTESIAN_POINT('Ctrl Pts',(0.789313025756584,-0.503610198143102,
-11.5911680301121));
#67647=CARTESIAN_POINT('Ctrl Pts',(0.849082786184241,0.392933716931585,
-11.5593948331234));
#67648=CARTESIAN_POINT('Ctrl Pts',(0.25176492241088,0.834790970545129,-11.532917168966));
#67649=CARTESIAN_POINT('Ctrl Pts',(-0.289087834282494,0.771116750379929,
-11.5117350376402));
#67650=CARTESIAN_POINT('Ctrl Pts',(-0.624034498747816,0.540076235369627,
-11.4958484391458));
#67651=CARTESIAN_POINT('Ctrl Pts',(-0.804439485071099,0.176267123032317,
-11.4799618406514));
#67652=CARTESIAN_POINT('Ctrl Pts',(-0.790240411000712,-0.369615224324265,
-11.4587797093255));
#67653=CARTESIAN_POINT('Ctrl Pts',(-0.372075622126741,-0.789325185240889,
-11.4375975779997));
#67654=CARTESIAN_POINT('Ctrl Pts',(0.172833538805439,-0.804336911067798,
-11.4164154466738));
#67655=CARTESIAN_POINT('Ctrl Pts',(0.661245923546358,-0.568320490261234,
-11.395233315348));
#67656=CARTESIAN_POINT('Ctrl Pts',(0.927621995011193,0.127116573399042,
-11.3687556511906));
#67657=CARTESIAN_POINT('Ctrl Pts',(0.392795607410976,0.849146302721704,
-11.3369824542019));
#67658=CARTESIAN_POINT('Ctrl Pts',(-0.348510610217431,0.799250627735656,
-11.3105047900445));
#67659=CARTESIAN_POINT('Ctrl Pts',(-0.71952459067659,0.400596402966526,
-11.2893226587187));
#67660=CARTESIAN_POINT('Ctrl Pts',(-0.825252913065406,0.00767089787905485,
-11.2734360602243));
#67661=CARTESIAN_POINT('Ctrl Pts',(-0.727243390108357,-0.386406665398893,
-11.2575494617299));
#67662=CARTESIAN_POINT('Ctrl Pts',(-0.363042629979021,-0.793281375912599,
-11.236367330404));
#67663=CARTESIAN_POINT('Ctrl Pts',(0.227378927841211,-0.842480462017667,
-11.2151851990782));
#67664=CARTESIAN_POINT('Ctrl Pts',(0.652421592475167,-0.501173997058855,
-11.1940030677523));
#67665=CARTESIAN_POINT('Ctrl Pts',(0.871899210482239,-0.00510950742898545,
-11.1728209364264));
#67666=CARTESIAN_POINT('Ctrl Pts',(0.624735747529702,0.697385430750005,
-11.1463432722691));
#67667=CARTESIAN_POINT('Ctrl Pts',(-0.250311713924867,0.901488701922009,
-11.1145700752803));
#67668=CARTESIAN_POINT('Ctrl Pts',(-0.783028415884914,0.38357230044019,
-11.088092411123));
#67669=CARTESIAN_POINT('Ctrl Pts',(-0.807742087698623,-0.160455087713699,
-11.0669102797971));
#67670=CARTESIAN_POINT('Ctrl Pts',(-0.633965965572041,-0.528382784897813,
-11.0510236813027));
#67671=CARTESIAN_POINT('Ctrl Pts',(-0.304156942230524,-0.765298382385843,
-11.0351370828084));
#67672=CARTESIAN_POINT('Ctrl Pts',(0.23682486235197,-0.839648305648038,
-11.0139549514825));
#67673=CARTESIAN_POINT('Ctrl Pts',(0.718687898942275,-0.494936571238069,
-10.9927728201567));
#67674=CARTESIAN_POINT('Ctrl Pts',(0.821705947496933,0.0403564807112435,
-10.9715906888308));
#67675=CARTESIAN_POINT('Ctrl Pts',(0.667861223009512,0.560531646820518,
-10.9504085575049));
#67676=CARTESIAN_POINT('Ctrl Pts',(0.0247137011057215,0.935964970627296,
-10.9239308933476));
#67677=CARTESIAN_POINT('Ctrl Pts',(-0.774366185017812,0.525066515148126,
-10.8921576963588));
#67678=CARTESIAN_POINT('Ctrl Pts',(-0.845123525583511,-0.214540057447401,
-10.8656800322015));
#67679=CARTESIAN_POINT('Ctrl Pts',(-0.511782611418673,-0.645191191867571,
-10.8444979008756));
#67680=CARTESIAN_POINT('Ctrl Pts',(-0.141153160795665,-0.81312791003465,
-10.8286113023812));
#67681=CARTESIAN_POINT('Ctrl Pts',(0.263592134007046,-0.780200132324299,
-10.8127247038868));
#67682=CARTESIAN_POINT('Ctrl Pts',(0.72405410023979,-0.486663079072112,
-10.791542572561));
#67683=CARTESIAN_POINT('Ctrl Pts',(0.868175704982164,0.0880082434404666,
-10.7703604412351));
#67684=CARTESIAN_POINT('Ctrl Pts',(0.600171861350475,0.562692675028197,
-10.7491783099093));
#67685=CARTESIAN_POINT('Ctrl Pts',(0.146176171072608,0.859573654376184,
-10.7279961785834));
#67686=CARTESIAN_POINT('Ctrl Pts',(-0.587062635494574,0.729382379325026,
-10.7015185144261));
#67687=CARTESIAN_POINT('Ctrl Pts',(-0.930117875491998,-0.101086950290881,
-10.6697453174373));
#67688=CARTESIAN_POINT('Ctrl Pts',(-0.505262363873941,-0.710613223488523,
-10.64326765328));
#67689=CARTESIAN_POINT('Ctrl Pts',(0.0275900749206337,-0.823062514745925,
-10.6220855219541));
#67690=CARTESIAN_POINT('Ctrl Pts',(0.41879467985798,-0.711134466189467,
-10.6061989234597));
#67691=CARTESIAN_POINT('Ctrl Pts',(0.705971949833696,-0.424024369154948,
-10.5903123249653));
#67692=CARTESIAN_POINT('Ctrl Pts',(0.866909909130173,0.0977880466003558,
-10.5691301936395));
#67693=CARTESIAN_POINT('Ctrl Pts',(0.604743199683794,0.629094721064296,
-10.5479480623136));
#67694=CARTESIAN_POINT('Ctrl Pts',(0.0931850144054718,0.817401897953224,
-10.5267659309878));
#67695=CARTESIAN_POINT('Ctrl Pts',(-0.445032952688861,0.749786643858178,
-10.5055837996619));
#67696=CARTESIAN_POINT('Ctrl Pts',(-0.919621199894597,0.175892131626442,
-10.4791061355046));
#67697=CARTESIAN_POINT('Ctrl Pts',(-0.64348842062255,-0.6791616054766,-10.4473329385158));
#67698=CARTESIAN_POINT('Ctrl Pts',(0.0749108584025137,-0.868705688387979,
-10.4208552743585));
#67699=CARTESIAN_POINT('Ctrl Pts',(0.553840414872343,-0.609470188170057,
-10.3996731430326));
#67700=CARTESIAN_POINT('Ctrl Pts',(0.779556078641138,-0.270912408600226,
-10.3837865445382));
#67701=CARTESIAN_POINT('Ctrl Pts',(0.812578539516615,0.133825172169838,
-10.3678999460438));
#67702=CARTESIAN_POINT('Ctrl Pts',(0.597447442438676,0.635729381206725,
-10.346717814718));
#67703=CARTESIAN_POINT('Ctrl Pts',(0.0536837211124086,0.870972194574707,
-10.3255356833921));
#67704=CARTESIAN_POINT('Ctrl Pts',(-0.458122336948451,0.683339764740917,
-10.3043535520663));
#67705=CARTESIAN_POINT('Ctrl Pts',(-0.824576230095092,0.2833873339605,-10.2831714207404));
#67706=CARTESIAN_POINT('Ctrl Pts',(-0.814791030660772,-0.461255644538286,
-10.2566937565831));
#67707=CARTESIAN_POINT('Ctrl Pts',(-0.0508040537562885,-0.934214526728624,
-10.2249205595943));
#67708=CARTESIAN_POINT('Ctrl Pts',(0.61945510051208,-0.613625772106911,
-10.1984428954369));
#67709=CARTESIAN_POINT('Ctrl Pts',(0.816674080954391,-0.106002645775066,
-10.1772607641111));
#67710=CARTESIAN_POINT('Ctrl Pts',(0.769546288077532,0.298160566450391,
-10.1613741656167));
#67711=CARTESIAN_POINT('Ctrl Pts',(0.532707850926748,0.62802500360276,-10.1454875671223));
#67712=CARTESIAN_POINT('Ctrl Pts',(0.0438279986233484,0.871306145475099,
-10.1243054357965));
#67713=CARTESIAN_POINT('Ctrl Pts',(-0.52290872124537,0.698599294932571,
-10.1031233044706));
#67714=CARTESIAN_POINT('Ctrl Pts',(-0.791538290376542,0.224268688307269,
-10.0819411731447));
#67715=CARTESIAN_POINT('Ctrl Pts',(-0.811935907224159,-0.31779619703067,
-10.0607590418189));
#67716=CARTESIAN_POINT('Ctrl Pts',(-0.322431281728496,-0.879021764137039,
-10.0342813776615));
#67717=CARTESIAN_POINT('Ctrl Pts',(0.566043654210065,-0.74493786006443,
-10.0025081806728));
#67718=CARTESIAN_POINT('Ctrl Pts',(0.869375119096715,-0.0666941679594714,
-9.97603051651542));
#67719=CARTESIAN_POINT('Ctrl Pts',(0.691082554031784,0.447881701933579,
-9.95484838518959));
#67720=CARTESIAN_POINT('Ctrl Pts',(0.393526148412095,0.72542289969084,-9.93896178669518));
#67721=CARTESIAN_POINT('Ctrl Pts',(-0.0005284759719869,0.823524608194793,
-9.92307518820079));
#67722=CARTESIAN_POINT('Ctrl Pts',(-0.530636846339506,0.692473703408921,
-9.90189305687493));
#67723=CARTESIAN_POINT('Ctrl Pts',(-0.850796171354358,0.193959739233485,
-9.88071092554907));
#67724=CARTESIAN_POINT('Ctrl Pts',(-0.74848409447556,-0.341468695496941,
-9.85952879422322));
#67725=CARTESIAN_POINT('Ctrl Pts',(-0.413123953802155,-0.767830019654057,
-9.83834666289735));
#67726=CARTESIAN_POINT('Ctrl Pts',(0.323282706987867,-0.878708987450492,
-9.81186899874004));
#67727=CARTESIAN_POINT('Ctrl Pts',(0.913670603537105,-0.201355064651968,
-9.78009580175124));
#67728=CARTESIAN_POINT('Ctrl Pts',(0.705804362960112,0.511958407461686,
-9.75361813759391));
#67729=CARTESIAN_POINT('Ctrl Pts',(0.23679947108692,0.788745285822342,-9.73243600626808));
#67730=CARTESIAN_POINT('Ctrl Pts',(-0.16966225545332,0.807660777773948,
-9.71654940777366));
#67731=CARTESIAN_POINT('Ctrl Pts',(-0.533513449991765,0.627340783200905,
-9.70066280927929));
#67732=CARTESIAN_POINT('Ctrl Pts',(-0.85272106081396,0.184288049125053,
-9.67948067795341));
#67733=CARTESIAN_POINT('Ctrl Pts',(-0.774029335533589,-0.40293063096293,
-9.65829854662756));
#67734=CARTESIAN_POINT('Ctrl Pts',(-0.349437115605602,-0.744797295862786,
-9.63711641530171));
#67735=CARTESIAN_POINT('Ctrl Pts',(0.18217734002223,-0.852669781961048,
-9.61593428397583));
#67736=CARTESIAN_POINT('Ctrl Pts',(0.815237502428397,-0.460466076815634,
-9.58945661981853));
#67737=CARTESIAN_POINT('Ctrl Pts',(0.82673903215434,0.437995897859057,-9.55768342282973));
#67738=CARTESIAN_POINT('Ctrl Pts',(0.206540088074968,0.847114160997335,
-9.5312057586724));
#67739=CARTESIAN_POINT('Ctrl Pts',(-0.33010978967523,0.754467124647978,
-9.51002362734656));
#67740=CARTESIAN_POINT('Ctrl Pts',(-0.652156174386574,0.505760355395116,
-9.49413702885215));
#67741=CARTESIAN_POINT('Ctrl Pts',(-0.812749627990668,0.132782159156536,
-9.47825043035777));
#67742=CARTESIAN_POINT('Ctrl Pts',(-0.769235476576637,-0.411548386197682,
-9.45706829903191));
#67743=CARTESIAN_POINT('Ctrl Pts',(-0.329119930899387,-0.808179792323179,
-9.43588616770604));
#67744=CARTESIAN_POINT('Ctrl Pts',(0.21580857366481,-0.793886622396449,
-9.4147040363802));
#67745=CARTESIAN_POINT('Ctrl Pts',(0.690831744825092,-0.531964134720561,
-9.39352190505433));
#67746=CARTESIAN_POINT('Ctrl Pts',(0.91945036799731,0.17678295747407,-9.36704424089702));
#67747=CARTESIAN_POINT('Ctrl Pts',(0.346595192110193,0.869027966543628,
-9.33527104390822));
#67748=CARTESIAN_POINT('Ctrl Pts',(-0.390958446283618,0.779366860357645,
-9.3087933797509));
#67749=CARTESIAN_POINT('Ctrl Pts',(-0.740012771240314,0.361350541462502,
-9.28761124842504));
#67750=CARTESIAN_POINT('Ctrl Pts',(-0.82447263842956,-0.0366889814648314,
-9.27172464993064));
#67751=CARTESIAN_POINT('Ctrl Pts',(-0.705427154896096,-0.424930098633222,
-9.25583805143626));
#67752=CARTESIAN_POINT('Ctrl Pts',(-0.319887370896094,-0.81164485000965,
-9.23465592011039));
#67753=CARTESIAN_POINT('Ctrl Pts',(0.272324957917033,-0.82904380036898,
-9.21347378878455));
#67754=CARTESIAN_POINT('Ctrl Pts',(0.678411741478122,-0.465388889759847,
-9.19229165745867));
#67755=CARTESIAN_POINT('Ctrl Pts',(0.870913883071089,0.0417534257410553,
-9.17110952613283));
#67756=CARTESIAN_POINT('Ctrl Pts',(0.586355750720453,0.72995077016243,-9.14463186197549));
#67757=CARTESIAN_POINT('Ctrl Pts',(-0.298395687321513,0.886734372637476,
-9.11285866498671));
#67758=CARTESIAN_POINT('Ctrl Pts',(-0.802509962736313,0.340938366062253,
-9.08638100082939));
#67759=CARTESIAN_POINT('Ctrl Pts',(-0.797952086762503,-0.203630996278515,
-9.06519886950353));
#67760=CARTESIAN_POINT('Ctrl Pts',(-0.604654772294215,-0.561688364862365,
-9.04931227100913));
#67761=CARTESIAN_POINT('Ctrl Pts',(-0.262590570136529,-0.780537796691881,
-9.03342567251473));
#67762=CARTESIAN_POINT('Ctrl Pts',(0.281605043851865,-0.825708115427715,
-9.0122435411889));
#67763=CARTESIAN_POINT('Ctrl Pts',(0.74424709487229,-0.45559934965813,-8.991061409863));
#67764=CARTESIAN_POINT('Ctrl Pts',(0.818349824448401,0.0844563467866882,
-8.96987927853718));
#67765=CARTESIAN_POINT('Ctrl Pts',(0.636773382186694,0.595612290022289,
-8.94869714721129));
#67766=CARTESIAN_POINT('Ctrl Pts',(-0.0256204313745529,0.935940589332386,
-8.92221948305399));
#67767=CARTESIAN_POINT('Ctrl Pts',(-0.801464097138213,0.482693624183378,
-8.89044628606519));
#67768=CARTESIAN_POINT('Ctrl Pts',(-0.832373000965563,-0.259646677251645,
-8.86396862190787));
#67769=CARTESIAN_POINT('Ctrl Pts',(-0.476370733590293,-0.671761892036649,
-8.84278649058203));
#67770=CARTESIAN_POINT('Ctrl Pts',(-0.0972519905765146,-0.819538445229283,
-8.82689989208761));
#67771=CARTESIAN_POINT('Ctrl Pts',(0.305138912861327,-0.764907382267323,
-8.81101329359324));
#67772=CARTESIAN_POINT('Ctrl Pts',(0.749160927417865,-0.447049435114738,
-8.78983116226736));
#67773=CARTESIAN_POINT('Ctrl Pts',(0.862191643692155,0.134536519882796,
-8.76864903094151));
#67774=CARTESIAN_POINT('Ctrl Pts',(0.56906570002938,0.59413259356591,-8.74746689961565));
#67775=CARTESIAN_POINT('Ctrl Pts',(0.0997717649227431,0.866187009375733,
-8.7262847682898));
#67776=CARTESIAN_POINT('Ctrl Pts',(-0.625411065729518,0.696779873508656,
-8.69980710413246));
#67777=CARTESIAN_POINT('Ctrl Pts',(-0.92334146161966,-0.150925077713834,
-8.66803390714369));
#67778=CARTESIAN_POINT('Ctrl Pts',(-0.466344151485975,-0.736738991854688,
-8.64155624298635));
#67779=CARTESIAN_POINT('Ctrl Pts',(0.0717812901244923,-0.820390493485922,
-8.62037411166051));
#67780=CARTESIAN_POINT('Ctrl Pts',(0.456405624116447,-0.687600988331753,
-8.6044875131661));
#67781=CARTESIAN_POINT('Ctrl Pts',(0.72773872432255,-0.385472967548476,
-8.58860091467172));
#67782=CARTESIAN_POINT('Ctrl Pts',(0.860402113835931,0.144234167632582,
-8.56741878334586));
#67783=CARTESIAN_POINT('Ctrl Pts',(0.57006201063428,0.660684349494034,-8.54623665201998));
#67784=CARTESIAN_POINT('Ctrl Pts',(0.0491234764725384,0.821228466230034,
-8.52505452069416));
#67785=CARTESIAN_POINT('Ctrl Pts',(-0.484683136277,0.724787277548224,-8.50387238936827));
#67786=CARTESIAN_POINT('Ctrl Pts',(-0.927744710107105,0.126217851875059,
-8.47739472521096));
#67787=CARTESIAN_POINT('Ctrl Pts',(-0.606060667659628,-0.712761040563262,
-8.44562152822217));
#67788=CARTESIAN_POINT('Ctrl Pts',(0.121486541926073,-0.863424710021134,
-8.41914386406484));
#67789=CARTESIAN_POINT('Ctrl Pts',(0.585792813827149,-0.578826307870058,
-8.397961732739));
#67790=CARTESIAN_POINT('Ctrl Pts',(0.792988341037864,-0.228627872005885,
-8.38207513424459));
#67791=CARTESIAN_POINT('Ctrl Pts',(0.804212631896132,0.177299470636368,
-8.36618853575021));
#67792=CARTESIAN_POINT('Ctrl Pts',(0.562420251644729,0.666917351060745,
-8.34500640442434));
#67793=CARTESIAN_POINT('Ctrl Pts',(0.00680041481536649,0.872598567494293,
-8.32382427309849));
#67794=CARTESIAN_POINT('Ctrl Pts',(-0.494182774760557,0.657732996600626,
-8.30264214177263));
#67795=CARTESIAN_POINT('Ctrl Pts',(-0.838613835539921,0.23866540412908,
-8.28146001044677));
#67796=CARTESIAN_POINT('Ctrl Pts',(-0.78882593018678,-0.504375698392214,
-8.25498234628944));
#67797=CARTESIAN_POINT('Ctrl Pts',(-0.000526288458951071,-0.935594761020664,
-8.22320914930067));
#67798=CARTESIAN_POINT('Ctrl Pts',(0.651536004617581,-0.579449777315683,
-8.19673148514333));
#67799=CARTESIAN_POINT('Ctrl Pts',(0.821190515837749,-0.0619616987512881,
-8.17554935381748));
#67800=CARTESIAN_POINT('Ctrl Pts',(0.752411237902168,0.339084859524061,
-8.15966275532308));
#67801=CARTESIAN_POINT('Ctrl Pts',(0.498188240520423,0.65574502407293,-8.1437761568287));
#67802=CARTESIAN_POINT('Ctrl Pts',(-0.00305901237357047,0.872402392849367,
-8.12259402550283));
#67803=CARTESIAN_POINT('Ctrl Pts',(-0.559695583195045,0.66948887950937,
-8.10141189417697));
#67804=CARTESIAN_POINT('Ctrl Pts',(-0.802446621511299,0.181407633004746,
-8.08022976285112));
#67805=CARTESIAN_POINT('Ctrl Pts',(-0.793684391543133,-0.36097011913437,
-8.05904763152525));
#67806=CARTESIAN_POINT('Ctrl Pts',(-0.274727049262383,-0.895078902481372,
-8.03256996736793));
#67807=CARTESIAN_POINT('Ctrl Pts',(0.605258403199313,-0.713442428781381,
-8.00079677037915));
#67808=CARTESIAN_POINT('Ctrl Pts',(0.871702976551815,-0.0198778875875173,
-7.97431910622182));
#67809=CARTESIAN_POINT('Ctrl Pts',(0.666014925458434,0.484373032363083,
-7.95313697489597));
#67810=CARTESIAN_POINT('Ctrl Pts',(0.353973530252757,0.745522603788999,
-7.93725037640157));
#67811=CARTESIAN_POINT('Ctrl Pts',(-0.0447836284226616,0.822306199790894,
-7.92136377790718));
#67812=CARTESIAN_POINT('Ctrl Pts',(-0.567083353921183,0.662956832917124,
-7.90018164658131));
#67813=CARTESIAN_POINT('Ctrl Pts',(-0.85999008173785,0.147957983722677,
-7.87899951525548));
#67814=CARTESIAN_POINT('Ctrl Pts',(-0.729052116288621,-0.381198532817697,
-7.85781738392959));
#67815=CARTESIAN_POINT('Ctrl Pts',(-0.371264073084344,-0.78892162368888,
-7.83663525260375));
#67816=CARTESIAN_POINT('Ctrl Pts',(0.370037062286983,-0.860066140362291,
-7.81015758844642));
#67817=CARTESIAN_POINT('Ctrl Pts',(0.923171081329685,-0.151963773398269,
-7.77838439145763));
#67818=CARTESIAN_POINT('Ctrl Pts',(0.677272002002691,0.549148290580514,
-7.75190672730032));
#67819=CARTESIAN_POINT('Ctrl Pts',(0.194070403631153,0.80033105265787,-7.73072459597444));
#67820=CARTESIAN_POINT('Ctrl Pts',(-0.212820489925012,0.797376104450092,
-7.71483799748006));
#67821=CARTESIAN_POINT('Ctrl Pts',(-0.56645558113332,0.597763443338712,
-7.69895139898567));
#67822=CARTESIAN_POINT('Ctrl Pts',(-0.861392436550393,0.138196826518483,
-7.6777692676598));
#67823=CARTESIAN_POINT('Ctrl Pts',(-0.751257501705145,-0.443944446712085,
-7.65658713633396));
#67824=CARTESIAN_POINT('Ctrl Pts',(-0.308907033835764,-0.762499674841944,
-7.63540500500809));
#67825=CARTESIAN_POINT('Ctrl Pts',(0.227736257654196,-0.841647513652085,
-7.61422287368224));
#67826=CARTESIAN_POINT('Ctrl Pts',(0.838804750428707,-0.415990124788927,
-7.58774520952491));
#67827=CARTESIAN_POINT('Ctrl Pts',(0.802006637013915,0.481791643778187,
-7.55597201253612));
#67828=CARTESIAN_POINT('Ctrl Pts',(0.160718023638984,0.856989455373761,
-7.5294943483788));
#67829=CARTESIAN_POINT('Ctrl Pts',(-0.370177566713595,0.735636924383227,
-7.50831221705294));
#67830=CARTESIAN_POINT('Ctrl Pts',(-0.678393176155383,0.469982884183816,
-7.49242561855855));
#67831=CARTESIAN_POINT('Ctrl Pts',(-0.818710855193977,0.0889134139305586,
-7.47653902006415));
#67832=CARTESIAN_POINT('Ctrl Pts',(-0.746007454897768,-0.45229212887575,
-7.4553568887383));
#67833=CARTESIAN_POINT('Ctrl Pts',(-0.285213055285053,-0.824698744227078,
-7.43417475741243));
#67834=CARTESIAN_POINT('Ctrl Pts',(0.258159907699396,-0.78114196644651,
-7.41299262608659));
#67835=CARTESIAN_POINT('Ctrl Pts',(0.71842104135087,-0.494070387324931,
-7.39181049476071));
#67836=CARTESIAN_POINT('Ctrl Pts',(0.90862149268301,0.225938434751966,-7.3653328306034));
#67837=CARTESIAN_POINT('Ctrl Pts',(0.299393105433013,0.886398105959188,
-7.33355963361461));
#67838=CARTESIAN_POINT('Ctrl Pts',(-0.432276398724546,0.75723069460368,
-7.30708196945729));
#67839=CARTESIAN_POINT('Ctrl Pts',(-0.758362287164713,0.321060363203428,
-7.28589983813143));
#67840=CARTESIAN_POINT('Ctrl Pts',(-0.821309607551199,-0.0809428281197334,
-7.27001323963704));
#67841=CARTESIAN_POINT('Ctrl Pts',(-0.681572209011577,-0.462225468242849,
-7.25412664114264));
#67842=CARTESIAN_POINT('Ctrl Pts',(-0.27580762554856,-0.827662640388744,
-7.23294450981678));
#67843=CARTESIAN_POINT('Ctrl Pts',(0.316483958824071,-0.81321117149348,
-7.21176237849093));
#67844=CARTESIAN_POINT('Ctrl Pts',(0.702441255430704,-0.428258791335588,
-7.19058024716506));
#67845=CARTESIAN_POINT('Ctrl Pts',(0.867411582321966,0.0884956899559494,
-7.16939811583921));
#67846=CARTESIAN_POINT('Ctrl Pts',(0.54628116408828,0.760406524844457,-7.14292045168187));
#67847=CARTESIAN_POINT('Ctrl Pts',(-0.345617286136612,0.869417348200748,
-7.11114725469311));
#67848=CARTESIAN_POINT('Ctrl Pts',(-0.819672226101789,0.297319107192211,
-7.08466959053576));
#67849=CARTESIAN_POINT('Ctrl Pts',(-0.785855974768107,-0.24621840372986,
-7.06348745920993));
#67850=CARTESIAN_POINT('Ctrl Pts',(-0.573596104350783,-0.593370644667842,
-7.04760086071551));
#67851=CARTESIAN_POINT('Ctrl Pts',(-0.220265301577946,-0.793521427883344,
-7.03171426222114));
#67852=CARTESIAN_POINT('Ctrl Pts',(0.325571376354598,-0.809381598199867,
-7.01053213089526));
#67853=CARTESIAN_POINT('Ctrl Pts',(0.767655389158747,-0.414945429099158,
-6.98934999956942));
#67854=CARTESIAN_POINT('Ctrl Pts',(0.812628640125686,0.128312130894811,
-6.96816786824355));
#67855=CARTESIAN_POINT('Ctrl Pts',(0.603845242726765,0.628971591666356,
-6.9469857369177));
#67856=CARTESIAN_POINT('Ctrl Pts',(-0.0758805198601191,0.933211305101612,
-6.92050807276037));
#67857=CARTESIAN_POINT('Ctrl Pts',(-0.826245748361245,0.438925730783531,
-6.88873487577159));
#67858=CARTESIAN_POINT('Ctrl Pts',(-0.817216887574368,-0.304002908550855,
-6.86225721161426));
#67859=CARTESIAN_POINT('Ctrl Pts',(-0.439582126714707,-0.696391175480518,
-6.8410750802884));
#67860=CARTESIAN_POINT('Ctrl Pts',(-0.0530697585057933,-0.823580483991598,
-6.82518848179402));
#67861=CARTESIAN_POINT('Ctrl Pts',(0.345803828966025,-0.747404021571874,
-6.80930188329962));
#67862=CARTESIAN_POINT('Ctrl Pts',(0.772102651795132,-0.406143801747123,
-6.78811975197376));
#67863=CARTESIAN_POINT('Ctrl Pts',(0.853715816646702,0.180675980803334,
-6.7669376206479));
#67864=CARTESIAN_POINT('Ctrl Pts',(0.536314917779641,0.623855446924663,
-6.74575548932204));
#67865=CARTESIAN_POINT('Ctrl Pts',(0.0530790146765816,0.870297051863717,
-6.72457335799618));
#67866=CARTESIAN_POINT('Ctrl Pts',(-0.661952034834192,0.662163648080895,
-6.69809569383887));
#67867=CARTESIAN_POINT('Ctrl Pts',(-0.91389655677108,-0.200327026088165,
-6.66632249685007));
#67868=CARTESIAN_POINT('Ctrl Pts',(-0.426078187219746,-0.760735557254639,
-6.63984483269276));
#67869=CARTESIAN_POINT('Ctrl Pts',(0.115765054710094,-0.815347513367804,
-6.61866270136689));
#67870=CARTESIAN_POINT('Ctrl Pts',(0.492697539306155,-0.662080318119721,
-6.6027761028725));
#67871=CARTESIAN_POINT('Ctrl Pts',(0.747402306832701,-0.345807534904014,
-6.5868895043781));
#67872=CARTESIAN_POINT('Ctrl Pts',(0.851407724907275,0.190263446815729,
-6.56570737305224));
#67873=CARTESIAN_POINT('Ctrl Pts',(0.533733320681469,0.690364575260483,
-6.54452524172639));
#67874=CARTESIAN_POINT('Ctrl Pts',(0.00491997057463909,0.822681654372687,
-6.52334311040053));
#67875=CARTESIAN_POINT('Ctrl Pts',(-0.522932569302915,0.697693247967738,
-6.50216097907467));
#67876=CARTESIAN_POINT('Ctrl Pts',(-0.933187000294144,0.0761788004565664,
-6.47568331491735));
#67877=CARTESIAN_POINT('Ctrl Pts',(-0.566881383083514,-0.744300574444075,
-6.44391011792856));
#67878=CARTESIAN_POINT('Ctrl Pts',(0.167711135250459,-0.85564839454374,
-6.41743245377124));
#67879=CARTESIAN_POINT('Ctrl Pts',(0.616052235469796,-0.546509608852112,
-6.39625032244538));
#67880=CARTESIAN_POINT('Ctrl Pts',(0.804128869206457,-0.185682568995067,
-6.38036372395099));
#67881=CARTESIAN_POINT('Ctrl Pts',(0.793522461442759,0.220261323442116,
-6.36447712545659));
#67882=CARTESIAN_POINT('Ctrl Pts',(0.525767779146774,0.696178004642138,
-6.34329499413073));
#67883=CARTESIAN_POINT('Ctrl Pts',(-0.0401028011771158,0.871702907377351,
-6.32211286280489));
#67884=CARTESIAN_POINT('Ctrl Pts',(-0.528814706483476,0.630225578934503,
-6.30093073147902));
#67885=CARTESIAN_POINT('Ctrl Pts',(-0.850228516581944,0.193253200532271,
-6.27974860015315));
#67886=CARTESIAN_POINT('Ctrl Pts',(-0.760579602040354,-0.546036976699944,
-6.25327093599584));
#67887=CARTESIAN_POINT('Ctrl Pts',(0.0497503680220317,-0.93427305088848,
-6.22149773900705));
#67888=CARTESIAN_POINT('Ctrl Pts',(0.681738399204437,-0.543595833521218,
-6.19502007484973));
#67889=CARTESIAN_POINT('Ctrl Pts',(0.823327512862196,-0.017746274093434,
-6.17383794352387));
#67890=CARTESIAN_POINT('Ctrl Pts',(0.733115143655037,0.379039205950285,
-6.15795134502948));
#67891=CARTESIAN_POINT('Ctrl Pts',(0.462203772512288,0.68155123760968,-6.14206474653508));
#67892=CARTESIAN_POINT('Ctrl Pts',(-0.0498799697013847,0.871019985612516,
-6.12088261520922));
#67893=CARTESIAN_POINT('Ctrl Pts',(-0.594974604645952,0.638361893885933,
-6.09970048388337));
#67894=CARTESIAN_POINT('Ctrl Pts',(-0.810907624869373,0.138117835093518,
-6.0785183525575));
#67895=CARTESIAN_POINT('Ctrl Pts',(-0.77343850503288,-0.403324024697871,
-6.05733622123165));
#67896=CARTESIAN_POINT('Ctrl Pts',(-0.225596939568173,-0.908076555586584,
-6.03085855707432));
#67897=CARTESIAN_POINT('Ctrl Pts',(0.641639344974892,-0.680705173610852,
-5.99908536008554));
#67898=CARTESIAN_POINT('Ctrl Pts',(0.919468928149147,0.170110871229085,
-5.96731216309674));
#67899=CARTESIAN_POINT('Ctrl Pts',(0.35533929095156,0.864924740453239,-5.93553896610797));
#67900=CARTESIAN_POINT('Ctrl Pts',(-0.534401559546241,0.767773114634092,
-5.90376576911917));
#67901=CARTESIAN_POINT('Ctrl Pts',(-0.935052121943657,-0.0342715508429932,
-5.87199257213039));
#67902=CARTESIAN_POINT('Ctrl Pts',(-0.55358600282851,-0.674106762641006,
-5.84551490797307));
#67903=CARTESIAN_POINT('Ctrl Pts',(-0.0313842813866094,-0.821987067613631,
-5.82433277664721));
#67904=CARTESIAN_POINT('Ctrl Pts',(0.502545841796061,-0.71340617086813,
-5.80315064532135));
#67905=CARTESIAN_POINT('Ctrl Pts',(0.842203744665662,-0.227720616512817,
-5.78196851399549));
#67906=CARTESIAN_POINT('Ctrl Pts',(0.76195469850279,0.312361095915287,-5.76078638266963));
#67907=CARTESIAN_POINT('Ctrl Pts',(0.521536699949039,0.639631146919876,
-5.74489978417524));
#67908=CARTESIAN_POINT('Ctrl Pts',(0.151740387604851,0.809418296339771,
-5.72901318568084));
#67909=CARTESIAN_POINT('Ctrl Pts',(-0.391979347919493,0.778855484654289,
-5.70783105435499));
#67910=CARTESIAN_POINT('Ctrl Pts',(-0.90413480588984,0.240585713443955,
-5.68135339019766));
#67911=CARTESIAN_POINT('Ctrl Pts',(-0.690614991381718,-0.632209336092332,
-5.64958019320888));
#67912=CARTESIAN_POINT('Ctrl Pts',(0.0144991791284147,-0.871794186565672,
-5.62310252905155));
#67913=CARTESIAN_POINT('Ctrl Pts',(0.508171989488816,-0.646985705588241,
-5.60192039772569));
#67914=CARTESIAN_POINT('Ctrl Pts',(0.844880298461512,-0.218292177285309,
-5.58073826639983));
#67915=CARTESIAN_POINT('Ctrl Pts',(0.789325408565671,0.371565567738826,
-5.55955613507398));
#67916=CARTESIAN_POINT('Ctrl Pts',(0.378551563372044,0.731362879347338,
-5.53837400374811));
#67917=CARTESIAN_POINT('Ctrl Pts',(-0.0165586512023453,0.825122455027266,
-5.52248740525373));
#67918=CARTESIAN_POINT('Ctrl Pts',(-0.408322682801,0.71516829914728,-5.50660080675932));
#67919=CARTESIAN_POINT('Ctrl Pts',(-0.802957826126081,0.339882228772198,
-5.48541867543348));
#67920=CARTESIAN_POINT('Ctrl Pts',(-0.844866528645535,-0.401918395173574,
-5.45894101127615));
#67921=CARTESIAN_POINT('Ctrl Pts',(-0.117118420384341,-0.928937276011495,
-5.42716781428736));
#67922=CARTESIAN_POINT('Ctrl Pts',(0.575409343140774,-0.655086580631771,
-5.40069015013004));
#67923=CARTESIAN_POINT('Ctrl Pts',(0.806151735036186,-0.164160563625932,
-5.37950801880418));
#67924=CARTESIAN_POINT('Ctrl Pts',(0.785272019256606,0.380555331263283,
-5.35832588747833));
#67925=CARTESIAN_POINT('Ctrl Pts',(0.361082683504556,0.794175414438857,
-5.33714375615246));
#67926=CARTESIAN_POINT('Ctrl Pts',(-0.184920996590559,0.802494413983792,
-5.31596162482661));
#67927=CARTESIAN_POINT('Ctrl Pts',(-0.546765877871137,0.618181435887277,
-5.30007502633221));
#67928=CARTESIAN_POINT('Ctrl Pts',(-0.774185727665808,0.280766049453372,
-5.28418842783782));
#67929=CARTESIAN_POINT('Ctrl Pts',(-0.832030667120703,-0.260741593664439,
-5.26300629651196));
#67930=CARTESIAN_POINT('Ctrl Pts',(-0.383766661157618,-0.853264896525865,
-5.23652863235464));
#67931=CARTESIAN_POINT('Ctrl Pts',(0.512083211324558,-0.783844358237307,
-5.20475543536584));
#67932=CARTESIAN_POINT('Ctrl Pts',(0.862643602471831,-0.126808341193055,
-5.17827777120853));
#67933=CARTESIAN_POINT('Ctrl Pts',(0.720711187517118,0.396742604062407,
-5.15709563988266));
#67934=CARTESIAN_POINT('Ctrl Pts',(0.352173705763636,0.798403523665007,
-5.13591350855682));
#67935=CARTESIAN_POINT('Ctrl Pts',(-0.238897473515934,0.839060957114792,
-5.11473137723095));
#67936=CARTESIAN_POINT('Ctrl Pts',(-0.660441788609072,0.491944817482841,
-5.0935492459051));
#67937=CARTESIAN_POINT('Ctrl Pts',(-0.816921181151555,0.117221997362471,
-5.0776626474107));
#67938=CARTESIAN_POINT('Ctrl Pts',(-0.771831834158657,-0.287173702127205,
-5.0617760489163));
#67939=CARTESIAN_POINT('Ctrl Pts',(-0.465374430984834,-0.737351916475205,
-5.04059391759045));
#67940=CARTESIAN_POINT('Ctrl Pts',(0.259859673417111,-0.898782945966624,
-5.01411625343313));
#67941=CARTESIAN_POINT('Ctrl Pts',(0.897728665382349,-0.265940663710014,
-4.98234305644434));
#67942=CARTESIAN_POINT('Ctrl Pts',(0.73958871850454,0.461782273098336,-4.95586539228701));
#67943=CARTESIAN_POINT('Ctrl Pts',(0.292487162343539,0.768947702741554,
-4.93468326096116));
#67944=CARTESIAN_POINT('Ctrl Pts',(-0.248424891230033,0.836516335197404,
-4.91350112963529));
#67945=CARTESIAN_POINT('Ctrl Pts',(-0.725253603938613,0.48487369755438,
-4.89231899830945));
#67946=CARTESIAN_POINT('Ctrl Pts',(-0.821844335556061,-0.0525827700264955,
-4.87113686698358));
#67947=CARTESIAN_POINT('Ctrl Pts',(-0.698533765966645,-0.439490376099843,
-4.85525026848919));
#67948=CARTESIAN_POINT('Ctrl Pts',(-0.402380543885497,-0.718528366396501,
-4.83936366999479));
#67949=CARTESIAN_POINT('Ctrl Pts',(0.122622432224616,-0.863264124622093,
-4.81818153866894));
#67950=CARTESIAN_POINT('Ctrl Pts',(0.779891974379151,-0.516823318096077,
-4.79170387451161));
#67951=CARTESIAN_POINT('Ctrl Pts',(0.856397877334779,0.378449295097978,
-4.75993067752283));
#67952=CARTESIAN_POINT('Ctrl Pts',(0.264771855760648,0.830740756604694,
-4.7334530133655));
#67953=CARTESIAN_POINT('Ctrl Pts',(-0.274849129440295,0.775427150500415,
-4.71227088203965));
#67954=CARTESIAN_POINT('Ctrl Pts',(-0.730868047059991,0.476766613157286,
-4.69108875071378));
#67955=CARTESIAN_POINT('Ctrl Pts',(-0.866665799372539,-0.0999283983858467,
-4.66990661938793));
#67956=CARTESIAN_POINT('Ctrl Pts',(-0.592362621446505,-0.572101026307649,
-4.64872448806207));
#67957=CARTESIAN_POINT('Ctrl Pts',(-0.247910861504431,-0.787173054434702,
-4.63283788956768));
#67958=CARTESIAN_POINT('Ctrl Pts',(0.158450323706088,-0.808137742177314,
-4.61695129107328));
#67959=CARTESIAN_POINT('Ctrl Pts',(0.652297814424352,-0.578592059262353,
-4.59576915974742));
#67960=CARTESIAN_POINT('Ctrl Pts',(0.92899332781192,0.110946972512963,-4.5692914955901));
#67961=CARTESIAN_POINT('Ctrl Pts',(0.407748529104943,0.842841818063406,
-4.53751829860131));
#67962=CARTESIAN_POINT('Ctrl Pts',(-0.335975364728725,0.804583677800187,
-4.51104063444399));
#67963=CARTESIAN_POINT('Ctrl Pts',(-0.711462127024278,0.413099202973537,
-4.48985850311813));
#67964=CARTESIAN_POINT('Ctrl Pts',(-0.865696935631178,-0.109742067018724,
-4.46867637179227));
#67965=CARTESIAN_POINT('Ctrl Pts',(-0.595875822308961,-0.637202712638309,
-4.44749424046642));
#67966=CARTESIAN_POINT('Ctrl Pts',(-0.0811423644714603,-0.819517526522297,
-4.42631210914056));
#67967=CARTESIAN_POINT('Ctrl Pts',(0.320623002143957,-0.760461769832068,
-4.41042551064616));
#67968=CARTESIAN_POINT('Ctrl Pts',(0.643919307037497,-0.513381964465409,
-4.39453891215177));
#67969=CARTESIAN_POINT('Ctrl Pts',(0.871728375130321,-0.0187309833400292,
-4.37335678082591));
#67970=CARTESIAN_POINT('Ctrl Pts',(0.636248391432616,0.685948845197852,
-4.34687911666859));
#67971=CARTESIAN_POINT('Ctrl Pts',(-0.234833508809209,0.906363291624296,
-4.3151059196798));
#67972=CARTESIAN_POINT('Ctrl Pts',(-0.776926530790784,0.395751823799299,
-4.28862825552248));
#67973=CARTESIAN_POINT('Ctrl Pts',(-0.809690669352921,-0.145706313007025,
-4.26744612419662));
#67974=CARTESIAN_POINT('Ctrl Pts',(-0.588784461095656,-0.644055404454502,
-4.24626399287076));
#67975=CARTESIAN_POINT('Ctrl Pts',(-0.0416763595216752,-0.871411713062787,
-4.22508186154491));
#67976=CARTESIAN_POINT('Ctrl Pts',(0.46867069141285,-0.677156438793757,
-4.20389973021904));
#67977=CARTESIAN_POINT('Ctrl Pts',(0.736662676991888,-0.372060899863277,
-4.18801313172465));
#67978=CARTESIAN_POINT('Ctrl Pts',(0.82312844087892,0.0255477049898826,
-4.17212653323026));
#67979=CARTESIAN_POINT('Ctrl Pts',(0.676548909322497,0.550038892296514,
-4.1509444019044));
#67980=CARTESIAN_POINT('Ctrl Pts',(0.0408920339190606,0.934700848074303,
-4.12446673774708));
#67981=CARTESIAN_POINT('Ctrl Pts',(-0.765724416674785,0.538801736236745,
-4.09269354075828));
#67982=CARTESIAN_POINT('Ctrl Pts',(-0.848357168761416,-0.201306866495383,
-4.06621587660097));
#67983=CARTESIAN_POINT('Ctrl Pts',(-0.522815457501024,-0.635211230289008,
-4.04503374527511));
#67984=CARTESIAN_POINT('Ctrl Pts',(-0.0318352824786834,-0.872044161969022,
-4.02385161394925));
#67985=CARTESIAN_POINT('Ctrl Pts',(0.532345145336561,-0.691161297269021,
-4.00266948262338));
#67986=CARTESIAN_POINT('Ctrl Pts',(0.795575358243202,-0.212727311235401,
-3.98148735129753));
#67987=CARTESIAN_POINT('Ctrl Pts',(0.802332052153671,0.193298967836865,
-3.96560075280314));
#67988=CARTESIAN_POINT('Ctrl Pts',(0.6108425695864,0.552326416709447,-3.94971415430875));
#67989=CARTESIAN_POINT('Ctrl Pts',(0.159590355860081,0.857200168024185,
-3.92853202298289));
#67990=CARTESIAN_POINT('Ctrl Pts',(-0.573913326002876,0.738891959670137,
-3.90205435882556));
#67991=CARTESIAN_POINT('Ctrl Pts',(-0.932422727675164,-0.0850238212413381,
-3.87028116183678));
#67992=CARTESIAN_POINT('Ctrl Pts',(-0.516293555233426,-0.702620313620022,
-3.84380349767945));
#67993=CARTESIAN_POINT('Ctrl Pts',(0.0127203886498161,-0.8225980193265,
-3.8226213663536));
#67994=CARTESIAN_POINT('Ctrl Pts',(0.540255341213515,-0.685272698949131,
-3.80143923502774));
#67995=CARTESIAN_POINT('Ctrl Pts',(0.853173521326546,-0.182181873723091,
-3.78025710370187));
#67996=CARTESIAN_POINT('Ctrl Pts',(0.744089772117057,0.352878832774126,
-3.75907497237603));
#67997=CARTESIAN_POINT('Ctrl Pts',(0.486397566632872,0.666722296052527,
-3.74318837388162));
#67998=CARTESIAN_POINT('Ctrl Pts',(0.108028752666176,0.816408539893724,
-3.72730177538723));
#67999=CARTESIAN_POINT('Ctrl Pts',(-0.433272302094322,0.756661299381776,
-3.70611964406138));
#68000=CARTESIAN_POINT('Ctrl Pts',(-0.915754966836196,0.19165248379213,
-3.67964197990405));
#68001=CARTESIAN_POINT('Ctrl Pts',(-0.655643663299691,-0.66841048767852,
-3.64786878291526));
#68002=CARTESIAN_POINT('Ctrl Pts',(0.0613287560853172,-0.869754634344714,
-3.62139111875794));
#68003=CARTESIAN_POINT('Ctrl Pts',(0.542206184319571,-0.61874208146278,
-3.60020898743208));
#68004=CARTESIAN_POINT('Ctrl Pts',(0.855390601589418,-0.172572953695659,
-3.57902685610623));
#68005=CARTESIAN_POINT('Ctrl Pts',(0.768216900074508,0.413446595155793,
-3.55784472478036));
#68006=CARTESIAN_POINT('Ctrl Pts',(0.338701423447491,0.7506493224828,-3.53666259345451));
#68007=CARTESIAN_POINT('Ctrl Pts',(-0.060876535391473,0.823040254373167,
-3.52077599496011));
#68008=CARTESIAN_POINT('Ctrl Pts',(-0.446165523219212,0.692191766279071,
-3.50488939646573));
#68009=CARTESIAN_POINT('Ctrl Pts',(-0.820062695127696,0.296240418923788,
-3.48370726513986));
#68010=CARTESIAN_POINT('Ctrl Pts',(-0.822046725490525,-0.446740433517228,
-3.45722960098254));
#68011=CARTESIAN_POINT('Ctrl Pts',(-0.0670284302510913,-0.933888849275838,
-3.42545640399375));
#68012=CARTESIAN_POINT('Ctrl Pts',(0.609781984565828,-0.623217675925539,
-3.39897873983643));
#68013=CARTESIAN_POINT('Ctrl Pts',(0.813808759860016,-0.120601045030234,
-3.37779660851058));
#68014=CARTESIAN_POINT('Ctrl Pts',(0.763686380628467,0.422205658035691,
-3.35661447718471));
#68015=CARTESIAN_POINT('Ctrl Pts',(0.317882211072159,0.812432269478428,
-3.33543234585885));
#68016=CARTESIAN_POINT('Ctrl Pts',(-0.227779543246364,0.791397207012838,
-3.314250214533));
#68017=CARTESIAN_POINT('Ctrl Pts',(-0.57919663904568,0.587905150681739,
-3.2983636160386));
#68018=CARTESIAN_POINT('Ctrl Pts',(-0.788155281402872,0.238755874924095,
-3.28247701754421));
#68019=CARTESIAN_POINT('Ctrl Pts',(-0.816816208015877,-0.305077845912804,
-3.26129488621835));
#68020=CARTESIAN_POINT('Ctrl Pts',(-0.337357962717805,-0.872655395227547,
-3.23481722206102));
#68021=CARTESIAN_POINT('Ctrl Pts',(0.553466755356614,-0.755192521135302,
-3.20304402507224));
#68022=CARTESIAN_POINT('Ctrl Pts',(0.868211701134554,-0.0802669440064075,
-3.17656636091491));
#68023=CARTESIAN_POINT('Ctrl Pts',(0.698348941736522,0.434900063535014,
-3.15538422958906));
#68024=CARTESIAN_POINT('Ctrl Pts',(0.308758890179159,0.816175504024769,
-3.1342020982632));
#68025=CARTESIAN_POINT('Ctrl Pts',(-0.283643096155971,0.825010234245042,
-3.11301996693734));
#68026=CARTESIAN_POINT('Ctrl Pts',(-0.685924375475703,0.455742044052894,
-3.09183783561148));
#68027=CARTESIAN_POINT('Ctrl Pts',(-0.822040182887849,0.0731515590922672,
-3.07595123711709));
#68028=CARTESIAN_POINT('Ctrl Pts',(-0.755283911462092,-0.328236695846971,
-3.06006463862269));
#68029=CARTESIAN_POINT('Ctrl Pts',(-0.425076929658484,-0.761295483775094,
-3.03888250729684));
#68030=CARTESIAN_POINT('Ctrl Pts',(0.307784443480434,-0.88351942263897,
-3.01240484313951));
#68031=CARTESIAN_POINT('Ctrl Pts',(0.910722986423459,-0.217312759090691,
-2.98063164615073));
#68032=CARTESIAN_POINT('Ctrl Pts',(0.713703985933684,0.500860220769669,
-2.9541539819934));
#68033=CARTESIAN_POINT('Ctrl Pts',(0.250741540134446,0.783554713940442,
-2.93297185066755));
#68034=CARTESIAN_POINT('Ctrl Pts',(-0.293019999508349,0.821957289354433,
-2.91178971934168));
#68035=CARTESIAN_POINT('Ctrl Pts',(-0.750262537092754,0.445198178389288,
-2.89060758801583));
#68036=CARTESIAN_POINT('Ctrl Pts',(-0.817830976145884,-0.0966724058121645,
-2.86942545668997));
#68037=CARTESIAN_POINT('Ctrl Pts',(-0.673906317084987,-0.476394257598558,
-2.85353885819558));
#68038=CARTESIAN_POINT('Ctrl Pts',(-0.363185640699209,-0.739113865249405,
-2.83765225970118));
#68039=CARTESIAN_POINT('Ctrl Pts',(0.168836743962548,-0.855427006606851,
-2.81647012837533));
#68040=CARTESIAN_POINT('Ctrl Pts',(0.806538915188326,-0.474165384771702,
-2.789992464218));
#68041=CARTESIAN_POINT('Ctrl Pts',(0.834822637619531,0.423924942627393,
-2.75821926722922));
#68042=CARTESIAN_POINT('Ctrl Pts',(0.219745546203246,0.84376906509478,-2.73174160307189));
#68043=CARTESIAN_POINT('Ctrl Pts',(-0.316123143402194,0.759536350606603,
-2.71055947174603));
#68044=CARTESIAN_POINT('Ctrl Pts',(-0.75543319544171,0.436801090726061,
-2.68937734042018));
#68045=CARTESIAN_POINT('Ctrl Pts',(-0.860043335086644,-0.146358308199602,
-2.66819520909432));
#68046=CARTESIAN_POINT('Ctrl Pts',(-0.560762143209286,-0.603107683861325,
-2.64701307776846));
#68047=CARTESIAN_POINT('Ctrl Pts',(-0.205250229032953,-0.799358215296395,
-2.63112647927406));
#68048=CARTESIAN_POINT('Ctrl Pts',(0.201650391521991,-0.798454904808682,
-2.61523988077967));
#68049=CARTESIAN_POINT('Ctrl Pts',(0.682448561078831,-0.542701733206808,
-2.59405774945381));
#68050=CARTESIAN_POINT('Ctrl Pts',(0.921688664885592,0.160710419233701,
-2.56758008529649));
#68051=CARTESIAN_POINT('Ctrl Pts',(0.361865308920915,0.863536155272751,
-2.53580688830771));
#68052=CARTESIAN_POINT('Ctrl Pts',(-0.378727911435124,0.785365844296184,
-2.50932922415038));
#68053=CARTESIAN_POINT('Ctrl Pts',(-0.732633853606216,0.374268548287705,
-2.48814709282452));
#68054=CARTESIAN_POINT('Ctrl Pts',(-0.858548488350327,-0.156105729510895,
-2.46696496149866));
#68055=CARTESIAN_POINT('Ctrl Pts',(-0.560771726234211,-0.668304095200904,
-2.44578283017281));
#68056=CARTESIAN_POINT('Ctrl Pts',(-0.0369845352724926,-0.822693870002639,
-2.42460069884694));
#68057=CARTESIAN_POINT('Ctrl Pts',(0.361026637840914,-0.742132723742336,
-2.40871410035255));
#68058=CARTESIAN_POINT('Ctrl Pts',(0.67057779376091,-0.478036126175377,
-2.39282750185816));
#68059=CARTESIAN_POINT('Ctrl Pts',(0.87147530780448,0.0281424524752154,
-2.3716453705323));
#68060=CARTESIAN_POINT('Ctrl Pts',(0.598466356625525,0.71914939603411,-2.34516770637498));
#68061=CARTESIAN_POINT('Ctrl Pts',(-0.283201807191348,0.892433711637579,
-2.31339450938619));
#68062=CARTESIAN_POINT('Ctrl Pts',(-0.797071418183535,0.353428202895539,
-2.28691684522887));
#68063=CARTESIAN_POINT('Ctrl Pts',(-0.80069044652496,-0.189008249901802,
-2.26573471390301));
#68064=CARTESIAN_POINT('Ctrl Pts',(-0.553322350976712,-0.674765797550789,
-2.24455258257715));
#68065=CARTESIAN_POINT('Ctrl Pts',(0.00521321548111552,-0.872392179578859,
-2.22337045125129));
#68066=CARTESIAN_POINT('Ctrl Pts',(0.504383596946202,-0.650991740900647,
-2.20218831992543));
#68067=CARTESIAN_POINT('Ctrl Pts',(0.755592604670905,-0.331935277797579,
-2.18630172143104));
#68068=CARTESIAN_POINT('Ctrl Pts',(0.820566080579593,0.0697454143027238,
-2.17041512293665));
#68069=CARTESIAN_POINT('Ctrl Pts',(0.646012391484676,0.585601570858967,
-2.14923299161079));
#68070=CARTESIAN_POINT('Ctrl Pts',(-0.00939754306034187,0.935547711243679,
-2.12275532745346));
#68071=CARTESIAN_POINT('Ctrl Pts',(-0.793572942149156,0.496873403144509,
-2.09098213046468));
#68072=CARTESIAN_POINT('Ctrl Pts',(-0.836313118389196,-0.246606383326159,
-2.06450446630735));
#68073=CARTESIAN_POINT('Ctrl Pts',(-0.487923956549996,-0.662389252865625,
-2.0433223349815));
#68074=CARTESIAN_POINT('Ctrl Pts',(0.0150740595623384,-0.872494858645637,
-2.02214020365564));
#68075=CARTESIAN_POINT('Ctrl Pts',(0.568718656160876,-0.661554519854988,
-2.00095807232978));
#68076=CARTESIAN_POINT('Ctrl Pts',(0.805857626289395,-0.169665982861812,
-1.97977594100392));
#68077=CARTESIAN_POINT('Ctrl Pts',(0.790784850518842,0.23613668302452,-1.96388934250953));
#68078=CARTESIAN_POINT('Ctrl Pts',(0.580278067886322,0.584354754703108,
-1.94800274401513));
#68079=CARTESIAN_POINT('Ctrl Pts',(0.113294116267464,0.864537826218961,
-1.92682061268928));
#68080=CARTESIAN_POINT('Ctrl Pts',(-0.612791798659163,0.706982351494664,
-1.90034294853195));
#68081=CARTESIAN_POINT('Ctrl Pts',(-0.926506210023761,-0.135009022109928,
-1.86856975154316));
#68082=CARTESIAN_POINT('Ctrl Pts',(-0.47778893867,-0.729350444143057,-1.84209208738584));
#68083=CARTESIAN_POINT('Ctrl Pts',(0.0569081290087825,-0.820725760860472,
-1.82090995605998));
#68084=CARTESIAN_POINT('Ctrl Pts',(0.576300970503701,-0.655249339588559,
-1.79972782473412));
#68085=CARTESIAN_POINT('Ctrl Pts',(0.861731058140963,-0.136069379513772,
-1.77854569340827));
#68086=CARTESIAN_POINT('Ctrl Pts',(0.724050967135742,0.39235603293315,-1.75736356208241));
#68087=CARTESIAN_POINT('Ctrl Pts',(0.449865296872678,0.691897700205439,
-1.74147696358801));
#68088=CARTESIAN_POINT('Ctrl Pts',(0.0639991479615115,0.82103424074408,
-1.72559036509362));
#68089=CARTESIAN_POINT('Ctrl Pts',(-0.473308921554199,0.732284012198431,
-1.70440823376776));
#68090=CARTESIAN_POINT('Ctrl Pts',(-0.924731019481197,0.142163200013653,
-1.67793056961044));
#68091=CARTESIAN_POINT('Ctrl Pts',(-0.618776106988036,-0.702678676696827,
-1.64615737262165));
#68092=CARTESIAN_POINT('Ctrl Pts',(0.10798043597624,-0.865202037522717,
-1.61967970846433));
#68093=CARTESIAN_POINT('Ctrl Pts',(0.574673663161916,-0.58871002246891,
-1.59849757713847));
#68094=CARTESIAN_POINT('Ctrl Pts',(0.863428554777207,-0.12635519945809,
-1.57731544581262));
#68095=CARTESIAN_POINT('Ctrl Pts',(0.744888341191182,0.454132856952076,
-1.55613331448676));
#68096=CARTESIAN_POINT('Ctrl Pts',(0.297872369146698,0.767766312941754,
-1.5349511831609));
#68097=CARTESIAN_POINT('Ctrl Pts',(-0.105018454779645,0.818579462871879,
-1.5190645846665));
#68098=CARTESIAN_POINT('Ctrl Pts',(-0.482718942225724,0.667214761700076,
-1.50317798617211));
#68099=CARTESIAN_POINT('Ctrl Pts',(-0.83479754287494,0.251742471891821,
-1.48199585484625));
#68100=CARTESIAN_POINT('Ctrl Pts',(-0.796851182620412,-0.490271380548884,
-1.45551819068893));
#68101=CARTESIAN_POINT('Ctrl Pts',(-0.0167447222186907,-0.936141446332493,
-1.42374499370014));
#68102=CARTESIAN_POINT('Ctrl Pts',(0.642392331962497,-0.589547650426033,
-1.39726732954282));
#68103=CARTESIAN_POINT('Ctrl Pts',(0.819113847908267,-0.0766929843740207,
-1.37608519821696));
#68104=CARTESIAN_POINT('Ctrl Pts',(0.739893659542249,0.462635794339282,
-1.3549030668911));
#68105=CARTESIAN_POINT('Ctrl Pts',(0.273763047578798,0.828341165454406,
-1.33372093556524));
#68106=CARTESIAN_POINT('Ctrl Pts',(-0.269979798721475,0.778012832716501,
-1.31253880423939));
#68107=CARTESIAN_POINT('Ctrl Pts',(-0.60995350043272,0.555929797897005,
-1.29665220574499));
#68108=CARTESIAN_POINT('Ctrl Pts',(-0.799847037243918,0.196055687053803,
-1.2807656072506));
#68109=CARTESIAN_POINT('Ctrl Pts',(-0.79924111982244,-0.348532411877579,
-1.25958347592474));
#68110=CARTESIAN_POINT('Ctrl Pts',(-0.289974287295851,-0.889523887557901,
-1.23310581176742));
#68111=CARTESIAN_POINT('Ctrl Pts',(0.593250759993301,-0.724358149696021,
-1.20133261477863));
#68112=CARTESIAN_POINT('Ctrl Pts',(0.87127063585088,-0.0334935723846185,
-1.17485495062131));
#68113=CARTESIAN_POINT('Ctrl Pts',(0.673968441674755,0.471800645732692,
-1.15367281929545));
#68114=CARTESIAN_POINT('Ctrl Pts',(0.264451749975724,0.831588706975706,
-1.13249068796959));
#68115=CARTESIAN_POINT('Ctrl Pts',(-0.327568979751748,0.808575201270978,
-1.11130855664373));
#68116=CARTESIAN_POINT('Ctrl Pts',(-0.709424615516163,0.418222159251501,
-1.09012642531788));
#68117=CARTESIAN_POINT('Ctrl Pts',(-0.824783458077394,0.0288697101095931,
-1.07423982682348));
#68118=CARTESIAN_POINT('Ctrl Pts',(-0.736553190313614,-0.368351073370029,
-1.05835322832909));
#68119=CARTESIAN_POINT('Ctrl Pts',(-0.383550940276186,-0.783038878956529,
-1.03717109700323));
#68120=CARTESIAN_POINT('Ctrl Pts',(0.354819705113078,-0.865702495486934,
-1.0106934328459));
#68121=CARTESIAN_POINT('Ctrl Pts',(0.921085284334245,-0.168056812556349,
-0.978920235857119));
#68122=CARTESIAN_POINT('Ctrl Pts',(0.68575662243418,0.538490663869619,-0.952442571699793));
#68123=CARTESIAN_POINT('Ctrl Pts',(0.208271265596164,0.795897223022045,
-0.931260440373937));
#68124=CARTESIAN_POINT('Ctrl Pts',(-0.336768269145502,0.805022756530337,
-0.910078309048077));
#68125=CARTESIAN_POINT('Ctrl Pts',(-0.773103183752531,0.404236020014726,
-0.888896177722221));
#68126=CARTESIAN_POINT('Ctrl Pts',(-0.811454054952501,-0.140482654767616,
-0.86771404639636));
#68127=CARTESIAN_POINT('Ctrl Pts',(-0.647331254010008,-0.511921342065259,
-0.851827447901969));
#68128=CARTESIAN_POINT('Ctrl Pts',(-0.32294111757287,-0.757563297681273,
-0.835940849407571));
#68129=CARTESIAN_POINT('Ctrl Pts',(0.214563111264144,-0.845117672891099,
-0.814758718081718));
#68130=CARTESIAN_POINT('Ctrl Pts',(0.830854928685622,-0.430137095935519,
-0.78828105392439));
#68131=CARTESIAN_POINT('Ctrl Pts',(0.810834729594931,0.468175431378649,
-0.756507856935606));
#68132=CARTESIAN_POINT('Ctrl Pts',(0.174084163878708,0.854358849777055,
-0.730030192778281));
#68133=CARTESIAN_POINT('Ctrl Pts',(-0.356483549772279,0.741450462537814,
-0.708848061452423));
#68134=CARTESIAN_POINT('Ctrl Pts',(-0.777815113960467,0.395573197022217,
-0.687665930126566));
#68135=CARTESIAN_POINT('Ctrl Pts',(-0.850935313686701,-0.192365237173437,
-0.666483798800706));
#68136=CARTESIAN_POINT('Ctrl Pts',(-0.527541041691738,-0.632371337784837,
-0.64530166747485));
#68137=CARTESIAN_POINT('Ctrl Pts',(-0.16199641567262,-0.809233201559615,
-0.629415068980455));
#68138=CARTESIAN_POINT('Ctrl Pts',(0.244267682003785,-0.786464502814039,
-0.613528470486061));
#68139=CARTESIAN_POINT('Ctrl Pts',(0.710627006659556,-0.505242979937425,
-0.592346339160204));
#68140=CARTESIAN_POINT('Ctrl Pts',(0.911720286535661,0.210009408709779,
-0.565868675002879));
#68141=CARTESIAN_POINT('Ctrl Pts',(0.314936286484835,0.881734837871569,
-0.534095478014093));
#68142=CARTESIAN_POINT('Ctrl Pts',(-0.42038592361789,0.763878279754945,
-0.50761781385677));
#68143=CARTESIAN_POINT('Ctrl Pts',(-0.751688237041493,0.334356236573434,
-0.486435682530911));
#68144=CARTESIAN_POINT('Ctrl Pts',(-0.848918814984445,-0.202018222450293,
-0.465253551205055));
#68145=CARTESIAN_POINT('Ctrl Pts',(-0.524046957129384,-0.697474091242304,
-0.444071419879193));
#68146=CARTESIAN_POINT('Ctrl Pts',(0.00728015342758569,-0.823492551981872,
-0.422889288553338));
#68147=CARTESIAN_POINT('Ctrl Pts',(0.400386949741799,-0.72165898187089,
-0.407002690058941));
#68148=CARTESIAN_POINT('Ctrl Pts',(0.695298182707548,-0.441308572056135,
-0.39111609156455));
#68149=CARTESIAN_POINT('Ctrl Pts',(0.868703867437267,0.0749341801834311,
-0.369933960238689));
#68150=CARTESIAN_POINT('Ctrl Pts',(0.558954270913066,0.750272355031231,
-0.343456296081368));
#68151=CARTESIAN_POINT('Ctrl Pts',(-0.33075083661154,0.875923608760214,
-0.31168309909258));
#68152=CARTESIAN_POINT('Ctrl Pts',(-0.814914090257261,0.310085436417102,
-0.285205434935257));
#68153=CARTESIAN_POINT('Ctrl Pts',(-0.789374400507719,-0.23176697493687,
-0.264023303609398));
#68154=CARTESIAN_POINT('Ctrl Pts',(-0.516265749197611,-0.703518292708922,
-0.242841172283541));
#68155=CARTESIAN_POINT('Ctrl Pts',(0.0520971392298091,-0.870867259982498,
-0.221659040957681));
#68156=CARTESIAN_POINT('Ctrl Pts',(0.538627180893952,-0.622926055038332,
-0.200476909631823));
#68157=CARTESIAN_POINT('Ctrl Pts',(0.772363051366356,-0.290891130998112,
-0.184590311137431));
#68158=CARTESIAN_POINT('Ctrl Pts',(0.815588095945512,0.11381593984541,-0.168703712643035));
#68159=CARTESIAN_POINT('Ctrl Pts',(0.613704285802587,0.619311120740718,
-0.147521581317179));
#68160=CARTESIAN_POINT('Ctrl Pts',(-0.0598573691488588,0.934023329961192,
-0.121043917159855));
#68161=CARTESIAN_POINT('Ctrl Pts',(-0.81878299272184,0.452927951066564,
-0.089270720171069));
#68162=CARTESIAN_POINT('Ctrl Pts',(-0.82243198967408,-0.290216640336301,
-0.0627930560137438));
#68163=CARTESIAN_POINT('Ctrl Pts',(-0.450841104190585,-0.688967090169176,
-0.0416109246878877));
#68164=CARTESIAN_POINT('Ctrl Pts',(-0.0678909476341013,-0.822331958162865,
-0.0257243261934915));
#68165=CARTESIAN_POINT('Ctrl Pts',(0.335042445358195,-0.753606364065075,
-0.00983772769910037));
#68166=CARTESIAN_POINT('Ctrl Pts',(0.547784979994835,-0.585740710520373,
0.000753337963830978));
#68167=CARTESIAN_POINT('Ctrl Pts',(0.627854069260493,-0.481288351939915,
0.00604887079529526));
#68168=CARTESIAN_POINT('Ctrl Pts',(-0.789664670674245,0.000390155355157968,
-0.0731331508236992));
#68169=CARTESIAN_POINT('Ctrl Pts',(-0.789545021916376,-0.108669478777935,
-0.0687554338824675));
#68170=CARTESIAN_POINT('Ctrl Pts',(-0.76801952939625,-0.217821296353336,
-0.0643777169412358));
#68171=CARTESIAN_POINT('Ctrl Pts',(-0.725153241366725,-0.317623382068616,
-0.0600000000000044));
#68172=CARTESIAN_POINT('',(-0.392888236737431,-0.550964357679653,-11.9089));
#68173=CARTESIAN_POINT('Ctrl Pts',(-0.393304595585779,-0.5512599337297,
-11.9089));
#68174=CARTESIAN_POINT('Ctrl Pts',(-0.408693527352117,-0.542220167284383,
-11.9089));
#68175=CARTESIAN_POINT('Ctrl Pts',(-0.423683838010449,-0.532561211544802,
-11.9089));
#68176=CARTESIAN_POINT('Ctrl Pts',(-0.438233215603795,-0.522291678473845,
-11.9089));
#68177=CARTESIAN_POINT('Ctrl Pts',(-0.461867821271025,-0.505609427775394,
-11.9089));
#68178=CARTESIAN_POINT('Ctrl Pts',(-0.48433990880594,-0.487317637060884,
-11.9089));
#68179=CARTESIAN_POINT('Ctrl Pts',(-0.50557477026688,-0.467604008788871,
-11.9089));
#68180=CARTESIAN_POINT('Ctrl Pts',(-0.513462092846287,-0.460281722006926,
-11.9089));
#68181=CARTESIAN_POINT('Ctrl Pts',(-0.521178574541802,-0.45276297817765,
-11.9089));
#68182=CARTESIAN_POINT('Ctrl Pts',(-0.528719788537152,-0.445056426895789,
-11.9089));
#68183=CARTESIAN_POINT('Ctrl Pts',(-0.534715058150292,-0.438929714041502,
-11.9089));
#68184=CARTESIAN_POINT('Ctrl Pts',(-0.54059879777543,-0.432684821204094,
-11.9089));
#68185=CARTESIAN_POINT('Ctrl Pts',(-0.546360102250889,-0.426336159151428,
-11.9089));
#68186=CARTESIAN_POINT('Ctrl Pts',(-0.569122064476836,-0.401253644168294,
-11.9089));
#68187=CARTESIAN_POINT('Ctrl Pts',(-0.59001352525143,-0.374516741518621,
-11.9089));
#68188=CARTESIAN_POINT('Ctrl Pts',(-0.608914082959629,-0.346409536900853,
-11.9089));
#68189=CARTESIAN_POINT('Ctrl Pts',(-0.620816625689087,-0.328709148947567,
-11.9089));
#68190=CARTESIAN_POINT('Ctrl Pts',(-0.631929073242191,-0.310464307003422,
-11.9089));
#68191=CARTESIAN_POINT('Ctrl Pts',(-0.642213965653337,-0.291738016113175,
-11.9089));
#68192=CARTESIAN_POINT('Ctrl Pts',(-0.645959537905604,-0.284918238837686,
-11.9089));
#68193=CARTESIAN_POINT('Ctrl Pts',(-0.649590737078314,-0.278042814352498,
-11.9089));
#68194=CARTESIAN_POINT('Ctrl Pts',(-0.653105696058218,-0.271116451571719,
-11.9089));
#68195=CARTESIAN_POINT('Ctrl Pts',(-0.655265359288032,-0.266860751548043,
-11.9089));
#68196=CARTESIAN_POINT('Ctrl Pts',(-0.657381222064642,-0.262585667889145,
-11.9089));
#68197=CARTESIAN_POINT('Ctrl Pts',(-0.659452991369261,-0.258291988249454,
-11.9089));
#68198=CARTESIAN_POINT('Ctrl Pts',(-0.674373045108698,-0.227370625131801,
-11.9089));
#68199=CARTESIAN_POINT('Ctrl Pts',(-0.687009656395958,-0.195487698886124,
-11.9089));
#68200=CARTESIAN_POINT('Ctrl Pts',(-0.697343938616677,-0.16289685564625,
-11.9089));
#68201=CARTESIAN_POINT('Ctrl Pts',(-0.707706518654146,-0.130216770629341,
-11.9089));
#68202=CARTESIAN_POINT('Ctrl Pts',(-0.715754605809521,-0.096823788691555,
-11.9089));
#68203=CARTESIAN_POINT('Ctrl Pts',(-0.721423679591164,-0.0629478567023877,
-11.9089));
#68204=CARTESIAN_POINT('Ctrl Pts',(-0.723047928495838,-0.0532420480381235,
-11.9089));
#68205=CARTESIAN_POINT('Ctrl Pts',(-0.724476578999849,-0.0434964909242276,
-11.9089));
#68206=CARTESIAN_POINT('Ctrl Pts',(-0.725707343184254,-0.033716403000824,
-11.9089));
#68207=CARTESIAN_POINT('Ctrl Pts',(-0.7265959059525,-0.026655568676088,
-11.9089));
#68208=CARTESIAN_POINT('Ctrl Pts',(-0.727381016204586,-0.0195781656773132,
-11.9089));
#68209=CARTESIAN_POINT('Ctrl Pts',(-0.728061009551409,-0.012498405674025,
-11.9089));
#68210=CARTESIAN_POINT('Ctrl Pts',(-0.731399290066069,0.0222581474273844,
-11.9089));
#68211=CARTESIAN_POINT('Ctrl Pts',(-0.732218291976249,0.05714868313061,
-11.9089));
#68212=CARTESIAN_POINT('Ctrl Pts',(-0.730480688047011,0.0919286611337855,
-11.9089));
#68213=CARTESIAN_POINT('Ctrl Pts',(-0.728924956179102,0.123068277725504,
-11.9089));
#68214=CARTESIAN_POINT('Ctrl Pts',(-0.725319517222503,0.15412018856309,
-11.9089));
#68215=CARTESIAN_POINT('Ctrl Pts',(-0.719751379176906,0.184897223577564,
-11.9089));
#68216=CARTESIAN_POINT('Ctrl Pts',(-0.716657727201263,0.201996913706878,
-11.9089));
#68217=CARTESIAN_POINT('Ctrl Pts',(-0.712957590969093,0.219011827659849,
-11.9089));
#68218=CARTESIAN_POINT('Ctrl Pts',(-0.708661430842914,0.235909638790339,
-11.9089));
#68219=CARTESIAN_POINT('Ctrl Pts',(-0.706772031377583,0.24334109254847,
-11.9089));
#68220=CARTESIAN_POINT('Ctrl Pts',(-0.704766683530507,0.250752063241591,
-11.9089));
#68221=CARTESIAN_POINT('Ctrl Pts',(-0.702648111992644,0.258132763274611,
-11.9089));
#68222=CARTESIAN_POINT('Ctrl Pts',(-0.692735592491751,0.292666094672686,
-11.9089));
#68223=CARTESIAN_POINT('Ctrl Pts',(-0.680390309661971,0.326397320788224,
-11.9089));
#68224=CARTESIAN_POINT('Ctrl Pts',(-0.665760390044392,0.359055268523425,
-11.9089));
#68225=CARTESIAN_POINT('Ctrl Pts',(-0.65223697684172,0.38924319389273,-11.9089));
#68226=CARTESIAN_POINT('Ctrl Pts',(-0.636760651354079,0.418514986268856,
-11.9089));
#68227=CARTESIAN_POINT('Ctrl Pts',(-0.619409069747327,0.446652163200523,
-11.9089));
#68228=CARTESIAN_POINT('Ctrl Pts',(-0.610436195617874,0.461202499457351,
-11.9089));
#68229=CARTESIAN_POINT('Ctrl Pts',(-0.600961251859437,0.475449264180526,
-11.9089));
#68230=CARTESIAN_POINT('Ctrl Pts',(-0.591004529339638,0.489375201004093,
-11.9089));
#68231=CARTESIAN_POINT('Ctrl Pts',(-0.585705005712024,0.496787362092886,
-11.9089));
#68232=CARTESIAN_POINT('Ctrl Pts',(-0.580268955949018,0.504108610136061,
-11.9089));
#68233=CARTESIAN_POINT('Ctrl Pts',(-0.574699182670622,0.511336161684331,
-11.9089));
#68234=CARTESIAN_POINT('Ctrl Pts',(-0.570153054722175,0.51723539176967,
-11.9089));
#68235=CARTESIAN_POINT('Ctrl Pts',(-0.565517950353427,0.523071829695112,
-11.9089));
#68236=CARTESIAN_POINT('Ctrl Pts',(-0.560804459523544,0.528833397455703,
-11.9089));
#68237=CARTESIAN_POINT('Ctrl Pts',(-0.537795487450174,0.556958571872463,
-11.9089));
#68238=CARTESIAN_POINT('Ctrl Pts',(-0.512871815585796,0.583368342494326,
-11.9089));
#68239=CARTESIAN_POINT('Ctrl Pts',(-0.486264283896923,0.607923354592398,
-11.9089));
#68240=CARTESIAN_POINT('Ctrl Pts',(-0.459447509931059,0.632671467903429,
-11.9089));
#68241=CARTESIAN_POINT('Ctrl Pts',(-0.430919545923936,0.655536450034859,
-11.9089));
#68242=CARTESIAN_POINT('Ctrl Pts',(-0.40087273304815,0.676347523766625,
-11.9089));
#68243=CARTESIAN_POINT('Ctrl Pts',(-0.381865830138765,0.689512116613626,
-11.9089));
#68244=CARTESIAN_POINT('Ctrl Pts',(-0.362250311091213,0.701854228634629,
-11.9089));
#68245=CARTESIAN_POINT('Ctrl Pts',(-0.342067962509662,0.713322310757549,
-11.9089));
#68246=CARTESIAN_POINT('Ctrl Pts',(-0.39330459558578,-0.5512599337297,-11.9089));
#68247=CARTESIAN_POINT('Ctrl Pts',(-0.223877593268971,-0.670321260978493,
-11.8991430932763));
#68248=CARTESIAN_POINT('Ctrl Pts',(0.249389096047715,-0.750562929726869,
-11.8787951208897));
#68249=CARTESIAN_POINT('Ctrl Pts',(0.77140418662287,-0.214212144206197,
-11.8478560828401));
#68250=CARTESIAN_POINT('Ctrl Pts',(0.626282581243407,0.404955323743999,
-11.8213784186828));
#68251=CARTESIAN_POINT('Ctrl Pts',(0.238575376523109,0.662775532235479,
-11.800196287357));
#68252=CARTESIAN_POINT('Ctrl Pts',(-0.1078208916813,0.6976941672648,-11.7843096888626));
#68253=CARTESIAN_POINT('Ctrl Pts',(-0.426851047433615,0.560357959801784,
-11.7684230903682));
#68254=CARTESIAN_POINT('Ctrl Pts',(-0.634958032955366,0.302047970066774,
-11.7533805346203));
#68255=CARTESIAN_POINT('Ctrl Pts',(-0.675710582128752,0.0947324392347568,
-11.7436335117039));
#68256=CARTESIAN_POINT('Ctrl Pts',(-0.675354504231418,1.55800137812273E-5,
-11.739182021619));
#68257=CARTESIAN_POINT('Origin',(-1.87869726832665E-16,-4.25270154953079E-17,
-11.9089));
#68258=CARTESIAN_POINT('',(-0.7911,-9.68818082805471E-17,-11.9089));
#68259=CARTESIAN_POINT('Origin',(0.,0.,-11.9089));
#68260=CARTESIAN_POINT('Origin',(0.,0.,-11.9089));
#68261=CARTESIAN_POINT('',(0.392888236737201,-0.550964357679817,-11.9089));
#68262=CARTESIAN_POINT('Ctrl Pts',(0.342488254090117,0.713746195864945,
-11.9089));
#68263=CARTESIAN_POINT('Ctrl Pts',(0.360556518434521,0.703639038104608,
-11.9089));
#68264=CARTESIAN_POINT('Ctrl Pts',(0.378182479561092,0.69280655077716,-11.9089));
#68265=CARTESIAN_POINT('Ctrl Pts',(0.395317146119975,0.681247267951702,
-11.9089));
#68266=CARTESIAN_POINT('Ctrl Pts',(0.421982268203321,0.663258608138712,
-11.9089));
#68267=CARTESIAN_POINT('Ctrl Pts',(0.447458851539857,0.643510628499277,
-11.9089));
#68268=CARTESIAN_POINT('Ctrl Pts',(0.471631160417591,0.622177706263673,
-11.9089));
#68269=CARTESIAN_POINT('Ctrl Pts',(0.483299586240594,0.611879905505248,
-11.9089));
#68270=CARTESIAN_POINT('Ctrl Pts',(0.494663745687151,0.60121247873265,-11.9089));
#68271=CARTESIAN_POINT('Ctrl Pts',(0.505708478051413,0.590193655482738,
-11.9089));
#68272=CARTESIAN_POINT('Ctrl Pts',(0.512460894688372,0.583457078897764,
-11.9089));
#68273=CARTESIAN_POINT('Ctrl Pts',(0.519087121920656,0.576595844964218,
-11.9089));
#68274=CARTESIAN_POINT('Ctrl Pts',(0.525582191777545,0.569617027475966,
-11.9089));
#68275=CARTESIAN_POINT('Ctrl Pts',(0.550035144131404,0.543342838700996,
-11.9089));
#68276=CARTESIAN_POINT('Ctrl Pts',(0.572642835681347,0.515393485339714,
-11.9089));
#68277=CARTESIAN_POINT('Ctrl Pts',(0.593235951420603,0.486007583538113,
-11.9089));
#68278=CARTESIAN_POINT('Ctrl Pts',(0.60601075151929,0.467778238062261,-11.9089));
#68279=CARTESIAN_POINT('Ctrl Pts',(0.618009497356723,0.448995505770734,
-11.9089));
#68280=CARTESIAN_POINT('Ctrl Pts',(0.629182717775896,0.429713041967115,
-11.9089));
#68281=CARTESIAN_POINT('Ctrl Pts',(0.633356702732471,0.422509683327209,
-11.9089));
#68282=CARTESIAN_POINT('Ctrl Pts',(0.637411228744753,0.415243679035629,
-11.9089));
#68283=CARTESIAN_POINT('Ctrl Pts',(0.641342116321425,0.407922266341704,
-11.9089));
#68284=CARTESIAN_POINT('Ctrl Pts',(0.643851100174008,0.403249198015819,
-11.9089));
#68285=CARTESIAN_POINT('Ctrl Pts',(0.646310023336052,0.398553019144131,
-11.9089));
#68286=CARTESIAN_POINT('Ctrl Pts',(0.648718392169465,0.393834526004733,
-11.9089));
#68287=CARTESIAN_POINT('Ctrl Pts',(0.664960125725092,0.362013607509625,
-11.9089));
#68288=CARTESIAN_POINT('Ctrl Pts',(0.678906723612393,0.329179154845523,
-11.9089));
#68289=CARTESIAN_POINT('Ctrl Pts',(0.690491164722862,0.295565210178431,
-11.9089));
#68290=CARTESIAN_POINT('Ctrl Pts',(0.701944731490535,0.262331016495882,
-11.9089));
#68291=CARTESIAN_POINT('Ctrl Pts',(0.711089352408651,0.228333711694692,
-11.9089));
#68292=CARTESIAN_POINT('Ctrl Pts',(0.717810313646535,0.193793925220808,
-11.9089));
#68293=CARTESIAN_POINT('Ctrl Pts',(0.720235359810493,0.181331336354761,
-11.9089));
#68294=CARTESIAN_POINT('Ctrl Pts',(0.722344384174073,0.168798150720673,
-11.9089));
#68295=CARTESIAN_POINT('Ctrl Pts',(0.724130318202715,0.156204981080871,
-11.9089));
#68296=CARTESIAN_POINT('Ctrl Pts',(0.72520494202273,0.148627478302282,-11.9089));
#68297=CARTESIAN_POINT('Ctrl Pts',(0.726161427478842,0.141035887537196,
-11.9089));
#68298=CARTESIAN_POINT('Ctrl Pts',(0.72699834563226,0.133438337157604,-11.9089));
#68299=CARTESIAN_POINT('Ctrl Pts',(0.730622843153363,0.100535116687562,
-11.9089));
#68300=CARTESIAN_POINT('Ctrl Pts',(0.732013163304079,0.0674856197810442,
-11.9089));
#68301=CARTESIAN_POINT('Ctrl Pts',(0.731094528381772,0.0344763444030268,
-11.9089));
#68302=CARTESIAN_POINT('Ctrl Pts',(0.730263242421242,0.0046057761035988,
-11.9089));
#68303=CARTESIAN_POINT('Ctrl Pts',(0.727540491121943,-0.0252324683759116,
-11.9089));
#68304=CARTESIAN_POINT('Ctrl Pts',(0.722968144611873,-0.054854753376587,
-11.9089));
#68305=CARTESIAN_POINT('Ctrl Pts',(0.720637288536924,-0.0699553768301293,
-11.9089));
#68306=CARTESIAN_POINT('Ctrl Pts',(0.71782534797267,-0.0849997333504113,
-11.9089));
#68307=CARTESIAN_POINT('Ctrl Pts',(0.714535318964831,-0.0999621540141962,
-11.9089));
#68308=CARTESIAN_POINT('Ctrl Pts',(0.712583835435694,-0.108837126670006,
-11.9089));
#68309=CARTESIAN_POINT('Ctrl Pts',(0.710464115508743,-0.117683251491007,
-11.9089));
#68310=CARTESIAN_POINT('Ctrl Pts',(0.708176520415106,-0.126494959184421,
-11.9089));
#68311=CARTESIAN_POINT('Ctrl Pts',(0.706420038263088,-0.133260845042161,
-11.9089));
#68312=CARTESIAN_POINT('Ctrl Pts',(0.704566928605242,-0.13999735578593,
-11.9089));
#68313=CARTESIAN_POINT('Ctrl Pts',(0.702618311219262,-0.146701346994649,
-11.9089));
#68314=CARTESIAN_POINT('Ctrl Pts',(0.693128653800149,-0.17934940831711,
-11.9089));
#68315=CARTESIAN_POINT('Ctrl Pts',(0.681375773134325,-0.211235078029093,
-11.9089));
#68316=CARTESIAN_POINT('Ctrl Pts',(0.667432282574939,-0.242091271590305,
-11.9089));
#68317=CARTESIAN_POINT('Ctrl Pts',(0.657257815394937,-0.264606819426136,
-11.9089));
#68318=CARTESIAN_POINT('Ctrl Pts',(0.6459158888732,-0.286574025624279,-11.9089));
#68319=CARTESIAN_POINT('Ctrl Pts',(0.633420198244177,-0.307879193780786,
-11.9089));
#68320=CARTESIAN_POINT('Ctrl Pts',(0.625264218444548,-0.321785149543534,
-11.9089));
#68321=CARTESIAN_POINT('Ctrl Pts',(0.616616438077692,-0.335408851785583,
-11.9089));
#68322=CARTESIAN_POINT('Ctrl Pts',(0.607493621761733,-0.34872796535831,
-11.9089));
#68323=CARTESIAN_POINT('Ctrl Pts',(0.60287540554187,-0.355470460680522,
-11.9089));
#68324=CARTESIAN_POINT('Ctrl Pts',(0.598135429986056,-0.362134865865414,
-11.9089));
#68325=CARTESIAN_POINT('Ctrl Pts',(0.593275738783337,-0.368718057791076,
-11.9089));
#68326=CARTESIAN_POINT('Ctrl Pts',(0.589123720455206,-0.374342599020702,
-11.9089));
#68327=CARTESIAN_POINT('Ctrl Pts',(0.584884848339669,-0.379906916848787,
-11.9089));
#68328=CARTESIAN_POINT('Ctrl Pts',(0.580568488351745,-0.385399387785345,
-11.9089));
#68329=CARTESIAN_POINT('Ctrl Pts',(0.559975931714266,-0.411602952631009,
-11.9089));
#68330=CARTESIAN_POINT('Ctrl Pts',(0.537577275146447,-0.436236631350958,
-11.9089));
#68331=CARTESIAN_POINT('Ctrl Pts',(0.513552303528644,-0.459132736511132,
-11.9089));
#68332=CARTESIAN_POINT('Ctrl Pts',(0.489919994544589,-0.48165462916035,
-11.9089));
#68333=CARTESIAN_POINT('Ctrl Pts',(0.46471309828054,-0.502495897953426,
-11.9089));
#68334=CARTESIAN_POINT('Ctrl Pts',(0.438076047439824,-0.521455358176732,
-11.9089));
#68335=CARTESIAN_POINT('Ctrl Pts',(0.423438349467291,-0.531874036060051,
-11.9089));
#68336=CARTESIAN_POINT('Ctrl Pts',(0.408368394069875,-0.541723664274757,
-11.9089));
#68337=CARTESIAN_POINT('Ctrl Pts',(0.392888236737142,-0.550964357679859,
-11.9089));
#68338=CARTESIAN_POINT('Origin',(0.,0.,-11.9089));
#68339=CARTESIAN_POINT('Origin',(0.,0.,-12.278617978381));
#68340=CARTESIAN_POINT('Ctrl Pts',(0.392888236737129,-0.550964357679868,
-11.9089));
#68341=CARTESIAN_POINT('Ctrl Pts',(0.484548909927025,-0.485601871403322,
-11.9036044671685));
#68342=CARTESIAN_POINT('Ctrl Pts',(0.634341446219948,-0.308693578393974,
-11.8930134015056));
#68343=CARTESIAN_POINT('Ctrl Pts',(0.705002038108303,0.0337351900899797,
-11.8771268030112));
#68344=CARTESIAN_POINT('Ctrl Pts',(0.602308840879945,0.365053324407907,
-11.8612402045168));
#68345=CARTESIAN_POINT('Ctrl Pts',(0.272406965382598,0.694503928448386,
-11.840058073191));
#68346=CARTESIAN_POINT('Ctrl Pts',(-0.363000708994007,0.713347601796957,
-11.8135804090336));
#68347=CARTESIAN_POINT('Ctrl Pts',(-0.666650932811795,0.269067688681329,
-11.7913351998198));
#68348=CARTESIAN_POINT('Ctrl Pts',(-0.677875715687106,0.0226766229145017,
-11.779681056269));
#68349=CARTESIAN_POINT('Ctrl Pts',(-0.677716351375759,0.000193615723412331,
-11.778617978381));
#68350=CARTESIAN_POINT('Ctrl Pts',(0.459308237155017,-0.644108029201275,
-11.9749488707953));
#68351=CARTESIAN_POINT('Ctrl Pts',(0.566464670671375,-0.567695641299125,
-11.9696533379638));
#68352=CARTESIAN_POINT('Ctrl Pts',(0.741580490770848,-0.360879990937501,
-11.9590622723009));
#68353=CARTESIAN_POINT('Ctrl Pts',(0.824186659298766,0.0394383166547306,
-11.9431756738065));
#68354=CARTESIAN_POINT('Ctrl Pts',(0.704132590542465,0.426767673916296,
-11.9272890753121));
#68355=CARTESIAN_POINT('Ctrl Pts',(0.318458918744054,0.811913784240501,
-11.9061069439863));
#68356=CARTESIAN_POINT('Ctrl Pts',(-0.424368052143095,0.833943088194967,
-11.8796292798289));
#68357=CARTESIAN_POINT('Ctrl Pts',(-0.931397559300446,0.0920927363171967,
-11.8478560828401));
#68358=CARTESIAN_POINT('Ctrl Pts',(-0.640145236706153,-0.591940276217127,
-11.8213784186828));
#68359=CARTESIAN_POINT('Ctrl Pts',(-0.141927077663759,-0.811168734010836,
-11.800196287357));
#68360=CARTESIAN_POINT('Ctrl Pts',(0.264031815171026,-0.781952385882165,
-11.7843096888626));
#68361=CARTESIAN_POINT('Ctrl Pts',(0.60394422145073,-0.559828087380095,
-11.7684230903682));
#68362=CARTESIAN_POINT('Ctrl Pts',(0.868547317678143,-0.0821550569317134,
-11.7472409590423));
#68363=CARTESIAN_POINT('Ctrl Pts',(0.720935568709495,0.491650503650886,
-11.7260588277165));
#68364=CARTESIAN_POINT('Ctrl Pts',(0.258901989905492,0.780895405589816,
-11.7048766963906));
#68365=CARTESIAN_POINT('Ctrl Pts',(-0.281744494913556,0.82514119516826,
-11.6836945650647));
#68366=CARTESIAN_POINT('Ctrl Pts',(-0.863972983588544,0.360817083758319,
-11.6572169009074));
#68367=CARTESIAN_POINT('Ctrl Pts',(-0.769136632246591,-0.532698155274108,
-11.6254437039186));
#68368=CARTESIAN_POINT('Ctrl Pts',(-0.104903716392486,-0.865596182377949,
-11.5989660397613));
#68369=CARTESIAN_POINT('Ctrl Pts',(0.417022089888044,-0.710130547992447,
-11.5777839084354));
#68370=CARTESIAN_POINT('Ctrl Pts',(0.707394488276981,-0.425081678732232,
-11.5618973099411));
#68371=CARTESIAN_POINT('Ctrl Pts',(0.822749350428807,-0.03572800263825,
-11.5460107114466));
#68372=CARTESIAN_POINT('Ctrl Pts',(0.715163821668032,0.499635896836913,
-11.5248285801208));
#68373=CARTESIAN_POINT('Ctrl Pts',(0.231228296670995,0.841432107454425,
-11.5036464487949));
#68374=CARTESIAN_POINT('Ctrl Pts',(-0.308185297928774,0.762791662764251,
-11.4824643174691));
#68375=CARTESIAN_POINT('Ctrl Pts',(-0.74889760168553,0.446527416008366,
-11.4612821861432));
#68376=CARTESIAN_POINT('Ctrl Pts',(-0.892089647326341,-0.284283749086055,
-11.4348045219859));
#68377=CARTESIAN_POINT('Ctrl Pts',(-0.241384542900942,-0.903919982673135,
-11.4030313249971));
#68378=CARTESIAN_POINT('Ctrl Pts',(0.480388704926853,-0.727659194643114,
-11.3765536608398));
#68379=CARTESIAN_POINT('Ctrl Pts',(0.777555337808534,-0.271294694573063,
-11.3553715295139));
#68380=CARTESIAN_POINT('Ctrl Pts',(0.814347127607299,0.133940169310587,
-11.3394849310195));
#68381=CARTESIAN_POINT('Ctrl Pts',(0.650220660779249,0.505377237137551,
-11.3235983325252));
#68382=CARTESIAN_POINT('Ctrl Pts',(0.221650746048364,0.843780919035312,
-11.3024162011993));
#68383=CARTESIAN_POINT('Ctrl Pts',(-0.368463008335961,0.791018025834893,
-11.2812340698734));
#68384=CARTESIAN_POINT('Ctrl Pts',(-0.728691043035294,0.381888299710684,
-11.2600519385476));
#68385=CARTESIAN_POINT('Ctrl Pts',(-0.859863472935527,-0.144461580418369,
-11.2388698072217));
#68386=CARTESIAN_POINT('Ctrl Pts',(-0.495910766423547,-0.794174857955777,
-11.2123921430644));
#68387=CARTESIAN_POINT('Ctrl Pts',(0.401173711199402,-0.845220377927278,
-11.1806189460756));
#68388=CARTESIAN_POINT('Ctrl Pts',(0.837199800884732,-0.243634363641056,
-11.1541412819183));
#68389=CARTESIAN_POINT('Ctrl Pts',(0.76826881600657,0.29657400723058,-11.1329591505924));
#68390=CARTESIAN_POINT('Ctrl Pts',(0.533981408593767,0.629257553118175,
-11.117072552098));
#68391=CARTESIAN_POINT('Ctrl Pts',(0.168435037412188,0.806115809149882,
-11.1011859536036));
#68392=CARTESIAN_POINT('Ctrl Pts',(-0.377283459386535,0.786608214983151,
-11.0800038222778));
#68393=CARTESIAN_POINT('Ctrl Pts',(-0.792906556675638,0.364381253655753,
-11.0588216909519));
#68394=CARTESIAN_POINT('Ctrl Pts',(-0.802617937082025,-0.18064815737068,
-11.0376395596261));
#68395=CARTESIAN_POINT('Ctrl Pts',(-0.561862488264964,-0.666741992503685,
-11.0164574283002));
#68396=CARTESIAN_POINT('Ctrl Pts',(0.136132386625423,-0.926341819511223,
-10.9899797641429));
#68397=CARTESIAN_POINT('Ctrl Pts',(0.85292637800386,-0.384518435883188,
-10.9582065671541));
#68398=CARTESIAN_POINT('Ctrl Pts',(0.795823295292128,0.356267445067071,
-10.9317289029968));
#68399=CARTESIAN_POINT('Ctrl Pts',(0.393579533887635,0.723386664183689,
-10.9105467716709));
#68400=CARTESIAN_POINT('Ctrl Pts',(-0.000355675929877251,0.825288486757545,
-10.8946601731765));
#68401=CARTESIAN_POINT('Ctrl Pts',(-0.393461383550265,0.72345089622168,
-10.8787735746821));
#68402=CARTESIAN_POINT('Ctrl Pts',(-0.796774721772053,0.355310195957094,
-10.8575914433563));
#68403=CARTESIAN_POINT('Ctrl Pts',(-0.840229183144532,-0.235561935437421,
-10.8364093120304));
#68404=CARTESIAN_POINT('Ctrl Pts',(-0.494804998307184,-0.6572650327969,
-10.8152271807046));
#68405=CARTESIAN_POINT('Ctrl Pts',(0.00337061571255417,-0.871907666692289,
-10.7940450493787));
#68406=CARTESIAN_POINT('Ctrl Pts',(0.703428476217358,-0.617923597308111,
-10.7675673852214));
#68407=CARTESIAN_POINT('Ctrl Pts',(0.899011593465778,0.259067536837369,
-10.7357941882326));
#68408=CARTESIAN_POINT('Ctrl Pts',(0.375938613330605,0.786721913226838,
-10.7093165240752));
#68409=CARTESIAN_POINT('Ctrl Pts',(-0.168303403544914,0.806143336987419,
-10.6881343927494));
#68410=CARTESIAN_POINT('Ctrl Pts',(-0.534523594447955,0.628797057768532,
-10.672247794255));
#68411=CARTESIAN_POINT('Ctrl Pts',(-0.76822034367083,0.296699449206626,
-10.6563611957606));
#68412=CARTESIAN_POINT('Ctrl Pts',(-0.837305291877463,-0.244979878357376,
-10.6351790644348));
#68413=CARTESIAN_POINT('Ctrl Pts',(-0.487923377363477,-0.72346754139835,
-10.6139969331089));
#68414=CARTESIAN_POINT('Ctrl Pts',(0.0483462858974055,-0.821274586436964,
-10.5928148017831));
#68415=CARTESIAN_POINT('Ctrl Pts',(0.567000592948025,-0.662378040007112,
-10.5716326704572));
#68416=CARTESIAN_POINT('Ctrl Pts',(0.93616106243427,-0.015609562633481,
-10.5451550062999));
#68417=CARTESIAN_POINT('Ctrl Pts',(0.517510382654335,0.779436230665358,
-10.5133818093111));
#68418=CARTESIAN_POINT('Ctrl Pts',(-0.222749378110494,0.842996989493808,
-10.4869041451538));
#68419=CARTESIAN_POINT('Ctrl Pts',(-0.650138150971392,0.50548343203859,
-10.4657220138279));
#68420=CARTESIAN_POINT('Ctrl Pts',(-0.814462273688168,0.133238198796839,
-10.4498354153335));
#68421=CARTESIAN_POINT('Ctrl Pts',(-0.777599598203426,-0.271167705420671,
-10.4339488168391));
#68422=CARTESIAN_POINT('Ctrl Pts',(-0.479598086123451,-0.728753022904691,
-10.4127666855133));
#68423=CARTESIAN_POINT('Ctrl Pts',(0.0964477485296225,-0.867278696520513,
-10.3915845541874));
#68424=CARTESIAN_POINT('Ctrl Pts',(0.568503188538161,-0.594670862165976,
-10.3704024228615));
#68425=CARTESIAN_POINT('Ctrl Pts',(0.860954673904028,-0.137809251394405,
-10.3492202915357));
#68426=CARTESIAN_POINT('Ctrl Pts',(0.723638252600749,0.594128666735248,
-10.3227426273783));
#68427=CARTESIAN_POINT('Ctrl Pts',(-0.110128271419062,0.929090737045152,
-10.2909694303896));
#68428=CARTESIAN_POINT('Ctrl Pts',(-0.715493674016255,0.498327213973867,
-10.2644917662322));
#68429=CARTESIAN_POINT('Ctrl Pts',(-0.82275525250952,-0.0355936775566611,
-10.2433096349064));
#68430=CARTESIAN_POINT('Ctrl Pts',(-0.707027736084488,-0.425691194749398,
-10.227423036412));
#68431=CARTESIAN_POINT('Ctrl Pts',(-0.417138201420715,-0.710062518729677,
-10.2115364379176));
#68432=CARTESIAN_POINT('Ctrl Pts',(0.106214778315677,-0.865917844528771,
-10.1903543065917));
#68433=CARTESIAN_POINT('Ctrl Pts',(0.634946553736723,-0.598596174004323,
-10.1691721752659));
#68434=CARTESIAN_POINT('Ctrl Pts',(0.818269532838146,-0.0852307533471595,
-10.14799004394));
#68435=CARTESIAN_POINT('Ctrl Pts',(0.74542289853333,0.452304148366167,-10.1268079126142));
#68436=CARTESIAN_POINT('Ctrl Pts',(0.166939798545099,0.921288389661671,
-10.1003302484568));
#68437=CARTESIAN_POINT('Ctrl Pts',(-0.685387896845896,0.636852623992408,
-10.0685570514681));
#68438=CARTESIAN_POINT('Ctrl Pts',(-0.86793603686864,-0.0833561374404725,
-10.0420793873107));
#68439=CARTESIAN_POINT('Ctrl Pts',(-0.604054844156638,-0.559741780346003,
-10.0208972559849));
#68440=CARTESIAN_POINT('Ctrl Pts',(-0.263317821004248,-0.78215403727239,
-10.0050106574905));
#68441=CARTESIAN_POINT('Ctrl Pts',(0.141721785662681,-0.811238556195293,
-9.98912405899608));
#68442=CARTESIAN_POINT('Ctrl Pts',(0.641509943308538,-0.591236234716949,
-9.96794192767022));
#68443=CARTESIAN_POINT('Ctrl Pts',(0.871453115729,-0.0452103165325772,-9.94675979634435));
#68444=CARTESIAN_POINT('Ctrl Pts',(0.678851857913411,0.464746667222898,
-9.92557766501851));
#68445=CARTESIAN_POINT('Ctrl Pts',(0.275354301209706,0.827293387555099,
-9.90439553369265));
#68446=CARTESIAN_POINT('Ctrl Pts',(-0.469158289932969,0.810266432879237,
-9.87791786953531));
#68447=CARTESIAN_POINT('Ctrl Pts',(-0.934664449803593,0.0417157057018528,
-9.84614467254655));
#68448=CARTESIAN_POINT('Ctrl Pts',(-0.607572078939521,-0.625393778860442,
-9.8196670083892));
#68449=CARTESIAN_POINT('Ctrl Pts',(-0.0980548570626957,-0.817666411454223,
-9.79848487706337));
#68450=CARTESIAN_POINT('Ctrl Pts',(0.305630886184607,-0.766610053606093,
-9.78259827856895));
#68451=CARTESIAN_POINT('Ctrl Pts',(0.6331762884375,-0.526574636067626,-9.76671168007458));
#68452=CARTESIAN_POINT('Ctrl Pts',(0.871691196454429,-0.0353518122569055,
-9.7455295487487));
#68453=CARTESIAN_POINT('Ctrl Pts',(0.69348056963452,0.52967839787378,-9.72434741742285));
#68454=CARTESIAN_POINT('Ctrl Pts',(0.216559770685256,0.793682036717495,
-9.703165286097));
#68455=CARTESIAN_POINT('Ctrl Pts',(-0.325677859285955,0.808806696472022,
-9.68198315477113));
#68456=CARTESIAN_POINT('Ctrl Pts',(-0.882116078545032,0.313866878207942,
-9.65550549061384));
#68457=CARTESIAN_POINT('Ctrl Pts',(-0.73939742316676,-0.573261968425616,
-9.62373229362499));
#68458=CARTESIAN_POINT('Ctrl Pts',(-0.0582356808045011,-0.869982652255475,
-9.59725462946773));
#68459=CARTESIAN_POINT('Ctrl Pts',(0.45458182105381,-0.686693878945643,
-9.57607249814183));
#68460=CARTESIAN_POINT('Ctrl Pts',(0.729215930288042,-0.386452247883321,
-9.56018589964745));
#68461=CARTESIAN_POINT('Ctrl Pts',(0.823480518688803,0.00853785273125205,
-9.54429930115305));
#68462=CARTESIAN_POINT('Ctrl Pts',(0.687280105947665,0.537346581430056,
-9.52311716982721));
#68463=CARTESIAN_POINT('Ctrl Pts',(0.185675927252062,0.852642337486147,
-9.50193503850133));
#68464=CARTESIAN_POINT('Ctrl Pts',(-0.348732121100362,0.745127651748426,
-9.48075290717549));
#68465=CARTESIAN_POINT('Ctrl Pts',(-0.771811648080317,0.405636684946787,
-9.45957077584961));
#68466=CARTESIAN_POINT('Ctrl Pts',(-0.875523258105161,-0.331813528628048,
-9.43309311169231));
#68467=CARTESIAN_POINT('Ctrl Pts',(-0.19245940133309,-0.915585721091894,
-9.4013199147035));
#68468=CARTESIAN_POINT('Ctrl Pts',(0.518798676753727,-0.700791797000234,
-9.37484225054619));
#68469=CARTESIAN_POINT('Ctrl Pts',(0.791011035633738,-0.229117124893915,
-9.35366011922032));
#68470=CARTESIAN_POINT('Ctrl Pts',(0.805972484214374,0.177509345019459,
-9.33777352072595));
#68471=CARTESIAN_POINT('Ctrl Pts',(0.622122289133055,0.539589581953811,
-9.32188692223153));
#68472=CARTESIAN_POINT('Ctrl Pts',(0.175985973568179,0.85447307137982,-9.3007047909057));
#68473=CARTESIAN_POINT('Ctrl Pts',(-0.410439596498066,0.770073920647401,
-9.27952265957981));
#68474=CARTESIAN_POINT('Ctrl Pts',(-0.74816061082109,0.342176869620224,
-9.25834052825398));
#68475=CARTESIAN_POINT('Ctrl Pts',(-0.850857640946981,-0.190461584392268,
-9.2371583969281));
#68476=CARTESIAN_POINT('Ctrl Pts',(-0.452515495106881,-0.81967732672793,
-9.2106807327708));
#68477=CARTESIAN_POINT('Ctrl Pts',(0.446015846735313,-0.82244008796376,
-9.17890753578198));
#68478=CARTESIAN_POINT('Ctrl Pts',(0.849082854713835,-0.198291491434303,
-9.1524298716247));
#68479=CARTESIAN_POINT('Ctrl Pts',(0.751220872924518,0.337431942021702,
-9.13124774029881));
#68480=CARTESIAN_POINT('Ctrl Pts',(0.499393721105105,0.657044233062526,
-9.11536114180443));
#68481=CARTESIAN_POINT('Ctrl Pts',(0.124871272155171,0.814002595192172,
-9.09947454331003));
#68482=CARTESIAN_POINT('Ctrl Pts',(-0.419010320228561,0.765196474212969,
-9.07829241198418));
#68483=CARTESIAN_POINT('Ctrl Pts',(-0.811342509484049,0.321244202965407,
-9.05711028065831));
#68484=CARTESIAN_POINT('Ctrl Pts',(-0.791750172340431,-0.223519516566628,
-9.03592814933246));
#68485=CARTESIAN_POINT('Ctrl Pts',(-0.525220111816607,-0.695972825928158,
-9.01474601800659));
#68486=CARTESIAN_POINT('Ctrl Pts',(0.185716948854799,-0.917687532971727,
-8.98826835384928));
#68487=CARTESIAN_POINT('Ctrl Pts',(0.872357765986865,-0.338126842991299,
-8.95649515686048));
#68488=CARTESIAN_POINT('Ctrl Pts',(0.77552763160743,0.398519889538282,-8.93001749270316));
#68489=CARTESIAN_POINT('Ctrl Pts',(0.354136265148752,0.743492179596064,
-8.90883536137731));
#68490=CARTESIAN_POINT('Ctrl Pts',(-0.0447058682790427,0.824076815728572,
-8.89294876288291));
#68491=CARTESIAN_POINT('Ctrl Pts',(-0.431770815408578,0.701261023122384,
-8.87706216438852));
#68492=CARTESIAN_POINT('Ctrl Pts',(-0.814717609633828,0.311978379312639,
-8.85588003306266));
#68493=CARTESIAN_POINT('Ctrl Pts',(-0.826356022783278,-0.280375158037511,
-8.8346979017368));
#68494=CARTESIAN_POINT('Ctrl Pts',(-0.458768809576972,-0.682905915223033,
-8.81351577041095));
#68495=CARTESIAN_POINT('Ctrl Pts',(0.050221749372257,-0.870466608306755,
-8.79233363908508));
#68496=CARTESIAN_POINT('Ctrl Pts',(0.735619000821108,-0.579228693086441,
-8.76585597492777));
#68497=CARTESIAN_POINT('Ctrl Pts',(0.883790308873034,0.307005738987016,
-8.73408277793897));
#68498=CARTESIAN_POINT('Ctrl Pts',(0.33311722255521,0.805787891309704,-8.70760511378166));
#68499=CARTESIAN_POINT('Ctrl Pts',(-0.211382054860909,0.795933880606166,
-8.6864229824558));
#68500=CARTESIAN_POINT('Ctrl Pts',(-0.567542525583312,0.599163328763069,
-8.6705363839614));
#68501=CARTESIAN_POINT('Ctrl Pts',(-0.783054772697314,0.254986828179804,
-8.65464978546701));
#68502=CARTESIAN_POINT('Ctrl Pts',(-0.822930239729612,-0.28962236299112,
-8.63346765414114));
#68503=CARTESIAN_POINT('Ctrl Pts',(-0.448339433712863,-0.748642944141454,
-8.6122855228153));
#68504=CARTESIAN_POINT('Ctrl Pts',(0.09241142536838,-0.817489717457452,
-8.59110339148942));
#68505=CARTESIAN_POINT('Ctrl Pts',(0.601777224121419,-0.630950483648119,
-8.56992126016359));
#68506=CARTESIAN_POINT('Ctrl Pts',(0.935647144657611,0.0347219521013799,
-8.54344359600624));
#68507=CARTESIAN_POINT('Ctrl Pts',(0.474875948012168,0.806120752634742,
-8.51167039901748));
#68508=CARTESIAN_POINT('Ctrl Pts',(-0.267729856010204,0.829808371821463,
-8.48519273486012));
#68509=CARTESIAN_POINT('Ctrl Pts',(-0.676363187059825,0.469814808838856,
-8.4640106035343));
#68510=CARTESIAN_POINT('Ctrl Pts',(-0.820445533492922,0.0892767576216661,
-8.44812400503988));
#68511=CARTESIAN_POINT('Ctrl Pts',(-0.7619034974846,-0.312563785666185,
-8.4322374065455));
#68512=CARTESIAN_POINT('Ctrl Pts',(-0.439742132798475,-0.753473389873756,
-8.41105527521964));
#68513=CARTESIAN_POINT('Ctrl Pts',(0.142915624818966,-0.860842395457705,
-8.38987314389378));
#68514=CARTESIAN_POINT('Ctrl Pts',(0.599639089059623,-0.563260394985328,
-8.36869101256792));
#68515=CARTESIAN_POINT('Ctrl Pts',(0.867116398052039,-0.0913427201058315,
-8.34750888124207));
#68516=CARTESIAN_POINT('Ctrl Pts',(0.690664321177558,0.632158199121087,
-8.32103121708474));
#68517=CARTESIAN_POINT('Ctrl Pts',(-0.159898135915144,0.921829930062871,
-8.28925802009595));
#68518=CARTESIAN_POINT('Ctrl Pts',(-0.741239697580997,0.459156749350661,
-8.26278035593863));
#68519=CARTESIAN_POINT('Ctrl Pts',(-0.819653564523485,-0.0797568152445793,
-8.24159822461276));
#68520=CARTESIAN_POINT('Ctrl Pts',(-0.683129576299145,-0.46307147921814,
-8.22571162611839));
#68521=CARTESIAN_POINT('Ctrl Pts',(-0.37837692475353,-0.731453322094652,
-8.20982502762398));
#68522=CARTESIAN_POINT('Ctrl Pts',(0.152595409369933,-0.858958633256121,
-8.18864289629813));
#68523=CARTESIAN_POINT('Ctrl Pts',(0.666197387211884,-0.563609392138577,
-8.16746076497226));
#68524=CARTESIAN_POINT('Ctrl Pts',(0.82166738823947,-0.0411340830821482,
-8.14627863364641));
#68525=CARTESIAN_POINT('Ctrl Pts',(0.720039086476889,0.49170931883848,-8.12509650232054));
#68526=CARTESIAN_POINT('Ctrl Pts',(0.117188860902527,0.928928395595722,
-8.09861883816323));
#68527=CARTESIAN_POINT('Ctrl Pts',(-0.718621729503222,0.599099861220695,
-8.06684564117445));
#68528=CARTESIAN_POINT('Ctrl Pts',(-0.862202324405923,-0.129878256583835,
-8.04036797701711));
#68529=CARTESIAN_POINT('Ctrl Pts',(-0.573101651871943,-0.59139463307986,
-8.01918584569127));
#68530=CARTESIAN_POINT('Ctrl Pts',(-0.220904645367528,-0.795174415166241,
-8.00329924719686));
#68531=CARTESIAN_POINT('Ctrl Pts',(0.185112663155078,-0.802450223707911,
-7.98741264870248));
#68532=CARTESIAN_POINT('Ctrl Pts',(0.672355772075423,-0.555907373905817,
-7.9662305173766));
#68533=CARTESIAN_POINT('Ctrl Pts',(0.872623435995562,0.00168659006782953,
-7.94504838605077));
#68534=CARTESIAN_POINT('Ctrl Pts',(0.652895585756275,0.500556354257191,
-7.92386625472488));
#68535=CARTESIAN_POINT('Ctrl Pts',(0.230497960195097,0.840895374367688,
-7.90268412339905));
#68536=CARTESIAN_POINT('Ctrl Pts',(-0.512023774061414,0.783883185212936,
-7.87620645924171));
#68537=CARTESIAN_POINT('Ctrl Pts',(-0.935555629394363,-0.0085731054685198,
-7.84443326225293));
#68538=CARTESIAN_POINT('Ctrl Pts',(-0.573085689409466,-0.657140778173378,
-7.8179555980956));
#68539=CARTESIAN_POINT('Ctrl Pts',(-0.0539720672566957,-0.821754301096167,
-7.79677346676974));
#68540=CARTESIAN_POINT('Ctrl Pts',(0.346386592324105,-0.749077794049471,
-7.78088686827535));
#68541=CARTESIAN_POINT('Ctrl Pts',(0.660559268446202,-0.491787060076878,
-7.76500026978096));
#68542=CARTESIAN_POINT('Ctrl Pts',(0.872331380217636,0.0115436429949378,
-7.74381813845509));
#68543=CARTESIAN_POINT('Ctrl Pts',(0.664013750878078,0.56618039905986,-7.72263600712925));
#68544=CARTESIAN_POINT('Ctrl Pts',(0.173594650754386,0.804172995640082,
-7.70145387580338));
#68545=CARTESIAN_POINT('Ctrl Pts',(-0.36867222958205,0.790136144864968,
-7.68027174447752));
#68546=CARTESIAN_POINT('Ctrl Pts',(-0.897708497584408,0.266008734120548,
-7.65379408032021));
#68547=CARTESIAN_POINT('Ctrl Pts',(-0.70752208830902,-0.612168545732056,
-7.62202088333141));
#68548=CARTESIAN_POINT('Ctrl Pts',(-0.0113989744896448,-0.871855075757903,
-7.59554321917409));
#68549=CARTESIAN_POINT('Ctrl Pts',(0.490827623867311,-0.661272530098432,
-7.57436108784823));
#68550=CARTESIAN_POINT('Ctrl Pts',(0.748930004517856,-0.346706015541711,
-7.55847448935384));
#68551=CARTESIAN_POINT('Ctrl Pts',(0.821831752970098,0.052779062130137,
-7.54258789085944));
#68552=CARTESIAN_POINT('Ctrl Pts',(0.657410161550947,0.573504291261676,
-7.52140575953358));
#68553=CARTESIAN_POINT('Ctrl Pts',(0.13958692969923,0.861388411050381,-7.50022362820774));
#68554=CARTESIAN_POINT('Ctrl Pts',(-0.388271088612359,0.725310189805061,
-7.47904149688187));
#68555=CARTESIAN_POINT('Ctrl Pts',(-0.79249513545432,0.363573652192116,
-7.45785936555601));
#68556=CARTESIAN_POINT('Ctrl Pts',(-0.856426571169585,-0.378384356783391,
-7.43138170139869));
#68557=CARTESIAN_POINT('Ctrl Pts',(-0.142978046749217,-0.924605381758418,
-7.39960850440991));
#68558=CARTESIAN_POINT('Ctrl Pts',(0.55570930206589,-0.671899085683014,
-7.37313084025257));
#68559=CARTESIAN_POINT('Ctrl Pts',(0.802180681898857,-0.186277397990996,
-7.35194870892673));
#68560=CARTESIAN_POINT('Ctrl Pts',(0.795268550736357,0.220565512013144,
-7.33606211043232));
#68561=CARTESIAN_POINT('Ctrl Pts',(0.592225960946144,0.572242492978857,
-7.32017551193793));
#68562=CARTESIAN_POINT('Ctrl Pts',(0.129812595197046,0.862695764875549,
-7.29899338061208));
#68563=CARTESIAN_POINT('Ctrl Pts',(-0.4512299990804,0.74690427336082,-7.27781124928622));
#68564=CARTESIAN_POINT('Ctrl Pts',(-0.765467966741164,0.301476535704575,
-7.25662911796036));
#68565=CARTESIAN_POINT('Ctrl Pts',(-0.839392798903865,-0.235911147331808,
-7.2354469866345));
#68566=CARTESIAN_POINT('Ctrl Pts',(-0.40781243725763,-0.84281089769987,
-7.20896932247717));
#68567=CARTESIAN_POINT('Ctrl Pts',(0.489568979966038,-0.797282915710522,
-7.17719612548839));
#68568=CARTESIAN_POINT('Ctrl Pts',(0.858512027676108,-0.152375549481188,
-7.15071846133107));
#68569=CARTESIAN_POINT('Ctrl Pts',(0.732001873721275,0.377314686014943,
-7.1295363300052));
#68570=CARTESIAN_POINT('Ctrl Pts',(0.463362767283833,0.682932030860315,
-7.11364973151082));
#68571=CARTESIAN_POINT('Ctrl Pts',(0.0809466243007569,0.819536883613883,
-7.09776313301642));
#68572=CARTESIAN_POINT('Ctrl Pts',(-0.459526225740245,0.741573287317527,
-7.07658100169057));
#68573=CARTESIAN_POINT('Ctrl Pts',(-0.827433652417946,0.277178744641522,
-7.05539887036469));
#68574=CARTESIAN_POINT('Ctrl Pts',(-0.778594220303515,-0.265744896088806,
-7.03421673903885));
#68575=CARTESIAN_POINT('Ctrl Pts',(-0.487059829810343,-0.723192272132506,
-7.01303460771298));
#68576=CARTESIAN_POINT('Ctrl Pts',(0.234764782229873,-0.906381095504675,
-6.98655694355566));
#68577=CARTESIAN_POINT('Ctrl Pts',(0.88926800774623,-0.290758051011389,
-6.95478374656688));
#68578=CARTESIAN_POINT('Ctrl Pts',(0.752990664370407,0.439620596782193,
-6.92830608240955));
#68579=CARTESIAN_POINT('Ctrl Pts',(0.313669529499514,0.761448975097948,
-6.9071239510837));
#68580=CARTESIAN_POINT('Ctrl Pts',(-0.0889268590147663,0.820483532208579,
-6.89123735258931));
#68581=CARTESIAN_POINT('Ctrl Pts',(-0.468832413633215,0.677044479717714,
-6.8753507540949));
#68582=CARTESIAN_POINT('Ctrl Pts',(-0.830305933457297,0.267744933607144,
-6.85416862276906));
#68583=CARTESIAN_POINT('Ctrl Pts',(-0.810094662937232,-0.324378086054845,
-6.83298649144319));
#68584=CARTESIAN_POINT('Ctrl Pts',(-0.421406762012617,-0.706573174286,-6.81180436011734));
#68585=CARTESIAN_POINT('Ctrl Pts',(0.0969277403211786,-0.866509869209777,
-6.79062222879147));
#68586=CARTESIAN_POINT('Ctrl Pts',(0.765683559285303,-0.538859796515862,
-6.76414456463416));
#68587=CARTESIAN_POINT('Ctrl Pts',(0.866014837596959,0.354056683203798,
-6.73237136764536));
#68588=CARTESIAN_POINT('Ctrl Pts',(0.289333110659433,0.822525112548018,
-6.70589370348804));
#68589=CARTESIAN_POINT('Ctrl Pts',(-0.253849804187702,0.783424145888391,
-6.68471157216219));
#68590=CARTESIAN_POINT('Ctrl Pts',(-0.598921237881815,0.567797995500131,
-6.6688249736678));
#68591=CARTESIAN_POINT('Ctrl Pts',(-0.795626144337943,0.212537285908078,
-6.65293837517339));
#68592=CARTESIAN_POINT('Ctrl Pts',(-0.806176889005594,-0.333427828561512,
-6.63175624384755));
#68593=CARTESIAN_POINT('Ctrl Pts',(-0.407459771995628,-0.771654740532012,
-6.61057411252167));
#68594=CARTESIAN_POINT('Ctrl Pts',(0.13620949180056,-0.811342273578339,
-6.58939198119583));
#68595=CARTESIAN_POINT('Ctrl Pts',(0.63481469825267,-0.597699455562655,
-6.56820984986996));
#68596=CARTESIAN_POINT('Ctrl Pts',(0.932429169023787,0.0849531159557454,
-6.54173218571265));
#68597=CARTESIAN_POINT('Ctrl Pts',(0.430869109575266,0.830475561361244,
-6.50995898872384));
#68598=CARTESIAN_POINT('Ctrl Pts',(-0.31193659363892,0.814221567831034,
-6.48348132456654));
#68599=CARTESIAN_POINT('Ctrl Pts',(-0.700633496159194,0.432788416497904,
-6.46229919324067));
#68600=CARTESIAN_POINT('Ctrl Pts',(-0.824057702288797,0.045057274866246,
-6.44641259474628));
#68601=CARTESIAN_POINT('Ctrl Pts',(-0.744005417244997,-0.353056491979323,
-6.43052599625189));
#68602=CARTESIAN_POINT('Ctrl Pts',(-0.398615423024649,-0.776016311853889,
-6.40934386492602));
#68603=CARTESIAN_POINT('Ctrl Pts',(0.188970689385073,-0.851917996021742,
-6.38816173360017));
#68604=CARTESIAN_POINT('Ctrl Pts',(0.629041753542907,-0.530222355654872,
-6.36697960227431));
#68605=CARTESIAN_POINT('Ctrl Pts',(0.870772724474157,-0.0446115706622471,
-6.34579747094845));
#68606=CARTESIAN_POINT('Ctrl Pts',(0.655693065363436,0.668359420519961,
-6.31931980679113));
#68607=CARTESIAN_POINT('Ctrl Pts',(-0.209203633915283,0.911907381421729,
-6.28754660980234));
#68608=CARTESIAN_POINT('Ctrl Pts',(-0.764847329829675,0.41865527253801,
-6.26106894564502));
#68609=CARTESIAN_POINT('Ctrl Pts',(-0.814177759528614,-0.123683869477853,
-6.23988681431916));
#68610=CARTESIAN_POINT('Ctrl Pts',(-0.657268681575078,-0.499125649235067,
-6.22400021582476));
#68611=CARTESIAN_POINT('Ctrl Pts',(-0.338500623740867,-0.750707495992228,
-6.20811361733038));
#68612=CARTESIAN_POINT('Ctrl Pts',(0.198485975997741,-0.849568798889214,
-6.1869314860045));
#68613=CARTESIAN_POINT('Ctrl Pts',(0.695616949385993,-0.526894436738678,
-6.16574935467867));
#68614=CARTESIAN_POINT('Ctrl Pts',(0.822580645933705,0.00296536296201527,
-6.14456722335279));
#68615=CARTESIAN_POINT('Ctrl Pts',(0.692831037543227,0.52996466239058,-6.12338509202694));
#68616=CARTESIAN_POINT('Ctrl Pts',(0.0665577394891163,0.933309743473525,
-6.09690742786962));
#68617=CARTESIAN_POINT('Ctrl Pts',(-0.74885079779902,0.560609547756868,
-6.06513423088083));
#68618=CARTESIAN_POINT('Ctrl Pts',(-0.87668553612213,-0.325243430519842,
-6.03336103389204));
#68619=CARTESIAN_POINT('Ctrl Pts',(-0.201777547445245,-0.913042518007263,
-6.00158783690326));
#68620=CARTESIAN_POINT('Ctrl Pts',(0.658129706567036,-0.66477505348379,
-5.96981463991446));
#68621=CARTESIAN_POINT('Ctrl Pts',(0.915328905939503,0.194087619131439,
-5.93804144292568));
#68622=CARTESIAN_POINT('Ctrl Pts',(0.429806015838223,0.759041618565978,
-5.91156377876836));
#68623=CARTESIAN_POINT('Ctrl Pts',(-0.110017993077991,0.81519553092574,
-5.8903816474425));
#68624=CARTESIAN_POINT('Ctrl Pts',(-0.617424004674881,0.616675186942424,
-5.86919951611664));
#68625=CARTESIAN_POINT('Ctrl Pts',(-0.868776556752314,0.0799444879365195,
-5.84801738479078));
#68626=CARTESIAN_POINT('Ctrl Pts',(-0.697113753108197,-0.43837978060043,
-5.82683525346492));
#68627=CARTESIAN_POINT('Ctrl Pts',(-0.404142498383631,-0.719581388380777,
-5.81094865497054));
#68628=CARTESIAN_POINT('Ctrl Pts',(-0.0107108149795365,-0.823449088968177,
-5.79506205647612));
#68629=CARTESIAN_POINT('Ctrl Pts',(0.519716779792302,-0.700112950868486,
-5.77387992515028));
#68630=CARTESIAN_POINT('Ctrl Pts',(0.931996334502745,-0.0820003976102612,
-5.74740226099295));
#68631=CARTESIAN_POINT('Ctrl Pts',(0.571989477491768,0.741259568978487,
-5.71562906400416));
#68632=CARTESIAN_POINT('Ctrl Pts',(-0.163761877828015,0.856397908273568,
-5.68915139984685));
#68633=CARTESIAN_POINT('Ctrl Pts',(-0.611578414438477,0.550273674755984,
-5.66796926852098));
#68634=CARTESIAN_POINT('Ctrl Pts',(-0.869796878220926,0.0701967522717843,
-5.64678713719512));
#68635=CARTESIAN_POINT('Ctrl Pts',(-0.713927964402905,-0.501400472057978,
-5.62560500586928));
#68636=CARTESIAN_POINT('Ctrl Pts',(-0.247546526044699,-0.785438517556817,
-5.60442287454341));
#68637=CARTESIAN_POINT('Ctrl Pts',(0.157788538732795,-0.810064214593159,
-5.58853627604902));
#68638=CARTESIAN_POINT('Ctrl Pts',(0.524898314535317,-0.63456667797246,
-5.57264967755462));
#68639=CARTESIAN_POINT('Ctrl Pts',(0.849343000973622,-0.197174203863991,
-5.55146754622876));
#68640=CARTESIAN_POINT('Ctrl Pts',(0.763442303930618,0.540826863398601,
-5.52498988207145));
#68641=CARTESIAN_POINT('Ctrl Pts',(-0.0438911083957374,0.935261865875422,
-5.49321668508264));
#68642=CARTESIAN_POINT('Ctrl Pts',(-0.679209033401171,0.546726100752257,
-5.46673902092534));
#68643=CARTESIAN_POINT('Ctrl Pts',(-0.822360459076503,0.0235071457076657,
-5.44555688959947));
#68644=CARTESIAN_POINT('Ctrl Pts',(-0.708393220507744,-0.50956211546672,
-5.42437475827362));
#68645=CARTESIAN_POINT('Ctrl Pts',(-0.219566532678745,-0.844325666406878,
-5.40319262694775));
#68646=CARTESIAN_POINT('Ctrl Pts',(0.319777840880432,-0.758903941179043,
-5.38201049562191));
#68647=CARTESIAN_POINT('Ctrl Pts',(0.644662005989868,-0.515278673062417,
-5.36612389712749));
#68648=CARTESIAN_POINT('Ctrl Pts',(0.810860951904657,-0.143866716523886,
-5.35023729863312));
#68649=CARTESIAN_POINT('Ctrl Pts',(0.775002633482968,0.399539895117439,
-5.32905516730725));
#68650=CARTESIAN_POINT('Ctrl Pts',(0.231783132694296,0.906429486092428,
-5.30257750314994));
#68651=CARTESIAN_POINT('Ctrl Pts',(-0.638897434822695,0.684434994019087,
-5.27080430616114));
#68652=CARTESIAN_POINT('Ctrl Pts',(-0.871611353577846,-0.0229780024351207,
-5.24432664200383));
#68653=CARTESIAN_POINT('Ctrl Pts',(-0.642012997391936,-0.514440104259355,
-5.22314451067796));
#68654=CARTESIAN_POINT('Ctrl Pts',(-0.210064536928675,-0.846963633196215,
-5.20196237935211));
#68655=CARTESIAN_POINT('Ctrl Pts',(0.379224671095523,-0.785674195477476,
-5.18078024802624));
#68656=CARTESIAN_POINT('Ctrl Pts',(0.735010038690682,-0.371420654532431,
-5.15959811670039));
#68657=CARTESIAN_POINT('Ctrl Pts',(0.824922358102787,0.0245828391735762,
-5.14371151820599));
#68658=CARTESIAN_POINT('Ctrl Pts',(0.711163238398459,0.415258911722287,
-5.12782491971161));
#68659=CARTESIAN_POINT('Ctrl Pts',(0.332056770722144,0.806225471417083,
-5.10664278838573));
#68660=CARTESIAN_POINT('Ctrl Pts',(-0.410116348914915,0.840917602492415,
-5.08016512422843));
#68661=CARTESIAN_POINT('Ctrl Pts',(-0.930032409127722,0.108078264400297,
-5.04839192723962));
#68662=CARTESIAN_POINT('Ctrl Pts',(-0.649459303570146,-0.581753344032707,
-5.02191426308231));
#68663=CARTESIAN_POINT('Ctrl Pts',(-0.156312362641779,-0.807710192440725,
-5.00073213175645));
#68664=CARTESIAN_POINT('Ctrl Pts',(0.388174699197929,-0.781533689956709,
-4.97955000043059));
#68665=CARTESIAN_POINT('Ctrl Pts',(0.797649655718905,-0.353341646763458,
-4.95836786910473));
#68666=CARTESIAN_POINT('Ctrl Pts',(0.800657962051566,0.192717117539353,
-4.93718573777887));
#68667=CARTESIAN_POINT('Ctrl Pts',(0.612834485043679,0.552752301506898,
-4.92129913928448));
#68668=CARTESIAN_POINT('Ctrl Pts',(0.273223226583257,0.776879774398488,
-4.90541254079008));
#68669=CARTESIAN_POINT('Ctrl Pts',(-0.268821391201312,0.829455405297251,
-4.88423040946423));
#68670=CARTESIAN_POINT('Ctrl Pts',(-0.856956962236578,0.375449861770003,
-4.8577527453069));
#68671=CARTESIAN_POINT('Ctrl Pts',(-0.778826887468074,-0.519682472881723,
-4.82597954831812));
#68672=CARTESIAN_POINT('Ctrl Pts',(-0.118412479963754,-0.863836109962943,
-4.79950188416079));
#68673=CARTESIAN_POINT('Ctrl Pts',(0.403733302816536,-0.716818477638608,
-4.77831975283494));
#68674=CARTESIAN_POINT('Ctrl Pts',(0.801790918663602,-0.344391969104003,
-4.75713762150907));
#68675=CARTESIAN_POINT('Ctrl Pts',(0.836697813406502,0.247046679084701,
-4.73595549018323));
#68676=CARTESIAN_POINT('Ctrl Pts',(0.485498252731183,0.665195088815462,
-4.71477335885736));
#68677=CARTESIAN_POINT('Ctrl Pts',(0.109271274779151,0.818022616672709,
-4.69888676036297));
#68678=CARTESIAN_POINT('Ctrl Pts',(-0.294666770169491,0.769002347182303,
-4.68300016186857));
#68679=CARTESIAN_POINT('Ctrl Pts',(-0.741843161944716,0.458181113556748,
-4.66181803054272));
#68680=CARTESIAN_POINT('Ctrl Pts',(-0.896213104327743,-0.268588729212688,
-4.6353403663854));
#68681=CARTESIAN_POINT('Ctrl Pts',(-0.257196993176862,-0.900272680894212,
-4.60356716939661));
#68682=CARTESIAN_POINT('Ctrl Pts',(0.46895349403166,-0.735062555652628,
-4.57708950523928));
#68683=CARTESIAN_POINT('Ctrl Pts',(0.771755993962188,-0.284994728847248,
-4.55590737391343));
#68684=CARTESIAN_POINT('Ctrl Pts',(0.834060650473717,0.256548897807251,
-4.53472524258756));
#68685=CARTESIAN_POINT('Ctrl Pts',(0.477797123153197,0.729935066778223,
-4.51354311126171));
#68686=CARTESIAN_POINT('Ctrl Pts',(-0.0605733428831204,0.821294058009192,
-4.49236097993585));
#68687=CARTESIAN_POINT('Ctrl Pts',(-0.446263360789283,0.694226350477263,
-4.47647438144146));
#68688=CARTESIAN_POINT('Ctrl Pts',(-0.722407838794893,0.395373279144789,
-4.46058778294706));
#68689=CARTESIAN_POINT('Ctrl Pts',(-0.862030699206853,-0.131012531344061,
-4.4394056516212));
#68690=CARTESIAN_POINT('Ctrl Pts',(-0.509213832980306,-0.784881587330448,
-4.41292798746389));
#68691=CARTESIAN_POINT('Ctrl Pts',(0.386760515085133,-0.8526766662896,-4.38115479047509));
#68692=CARTESIAN_POINT('Ctrl Pts',(0.833276572853283,-0.256679748755051,
-4.35467712631777));
#68693=CARTESIAN_POINT('Ctrl Pts',(0.772717359300933,0.282377747569235,
-4.33349499499192));
#68694=CARTESIAN_POINT('Ctrl Pts',(0.469635817471363,0.735470396809251,
-4.31231286366604));
#68695=CARTESIAN_POINT('Ctrl Pts',(-0.108352654717711,0.865652929771297,
-4.29113073234021));
#68696=CARTESIAN_POINT('Ctrl Pts',(-0.57783514405307,0.586770488254485,
-4.26994860101433));
#68697=CARTESIAN_POINT('Ctrl Pts',(-0.789546945310624,0.240243280927042,
-4.25406200251995));
#68698=CARTESIAN_POINT('Ctrl Pts',(-0.806558470603616,-0.166302582395967,
-4.23817540402555));
#68699=CARTESIAN_POINT('Ctrl Pts',(-0.572220602744597,-0.657894209990364,
-4.2169932726997));
#68700=CARTESIAN_POINT('Ctrl Pts',(0.119976890218829,-0.927870346353562,
-4.19051560854236));
#68701=CARTESIAN_POINT('Ctrl Pts',(0.846767618623912,-0.399531967824429,
-4.15874241155359));
#68702=CARTESIAN_POINT('Ctrl Pts',(0.801278008580111,0.343784661165928,
-4.13226474739625));
#68703=CARTESIAN_POINT('Ctrl Pts',(0.406160155819965,0.715446180723319,
-4.1110826160704));
#68704=CARTESIAN_POINT('Ctrl Pts',(-0.118156436265154,0.864588666478961,
-4.08990048474454));
#68705=CARTESIAN_POINT('Ctrl Pts',(-0.642967919858539,0.589650359652897,
-4.06871835341868));
#68706=CARTESIAN_POINT('Ctrl Pts',(-0.820267937436497,0.0731680968928279,
-4.04753622209283));
#68707=CARTESIAN_POINT('Ctrl Pts',(-0.7573075007919,-0.328003905653948,
-4.03164962359843));
#68708=CARTESIAN_POINT('Ctrl Pts',(-0.507095079487041,-0.648881881218796,
-4.01576302510404));
#68709=CARTESIAN_POINT('Ctrl Pts',(-0.0102518774661032,-0.871869318621008,
-3.99458089377819));
#68710=CARTESIAN_POINT('Ctrl Pts',(0.692104400777655,-0.629546926172355,
-3.96810322962085));
#68711=CARTESIAN_POINT('Ctrl Pts',(0.904036489905212,0.243637472863961,
-3.93633003263208));
#68712=CARTESIAN_POINT('Ctrl Pts',(0.388176906107868,0.78073877183831,-3.90985236847474));
#68713=CARTESIAN_POINT('Ctrl Pts',(-0.153574277836826,0.80823526950646,
-3.88867023714889));
#68714=CARTESIAN_POINT('Ctrl Pts',(-0.649751318698528,0.582492686206687,
-3.86748810582302));
#68715=CARTESIAN_POINT('Ctrl Pts',(-0.871775832726098,0.033199248195006,
-3.84630597449717));
#68716=CARTESIAN_POINT('Ctrl Pts',(-0.672566233662919,-0.475234385251865,
-3.82512384317131));
#68717=CARTESIAN_POINT('Ctrl Pts',(-0.364878699197954,-0.740246410157821,
-3.80923724467692));
#68718=CARTESIAN_POINT('Ctrl Pts',(0.0335520454040853,-0.822841039121903,
-3.79335064618252));
#68719=CARTESIAN_POINT('Ctrl Pts',(0.556592829034656,-0.671167365424921,
-3.77216851485667));
#68720=CARTESIAN_POINT('Ctrl Pts',(0.935054346233315,-0.0317994248225427,
-3.74569085069934));
#68721=CARTESIAN_POINT('Ctrl Pts',(0.531329001872747,0.770928456494234,
-3.71391765371055));
#68722=CARTESIAN_POINT('Ctrl Pts',(-0.209548262673311,0.846359182556483,
-3.68743998955324));
#68723=CARTESIAN_POINT('Ctrl Pts',(-0.640265964208693,0.516612819007808,
-3.66625785822737));
#68724=CARTESIAN_POINT('Ctrl Pts',(-0.872312539777597,0.0233524855530796,
-3.64507572690152));
#68725=CARTESIAN_POINT('Ctrl Pts',(-0.685951147375653,-0.539042035485203,
-3.62389359557565));
#68726=CARTESIAN_POINT('Ctrl Pts',(-0.204979675929423,-0.797606664995417,
-3.60271146424981));
#68727=CARTESIAN_POINT('Ctrl Pts',(0.201093113573265,-0.800414125658291,
-3.5868248657554));
#68728=CARTESIAN_POINT('Ctrl Pts',(0.558241201240319,-0.605441885445481,
-3.57093826726101));
#68729=CARTESIAN_POINT('Ctrl Pts',(0.85871176293571,-0.151245885696385,
-3.54975613593516));
#68730=CARTESIAN_POINT('Ctrl Pts',(0.733275270191108,0.581072467042636,
-3.52327847177783));
#68731=CARTESIAN_POINT('Ctrl Pts',(-0.0940883185327613,0.931551706336986,
-3.49150527478904));
#68732=CARTESIAN_POINT('Ctrl Pts',(-0.707608428889974,0.509435620712697,
-3.46502761063172));
#68733=CARTESIAN_POINT('Ctrl Pts',(-0.822435398042004,-0.0207201769966671,
-3.44384547930586));
#68734=CARTESIAN_POINT('Ctrl Pts',(-0.679985894907103,-0.546894586151797,
-3.42266334798001));
#68735=CARTESIAN_POINT('Ctrl Pts',(-0.173875497258729,-0.854905026338613,
-3.40148121665414));
#68736=CARTESIAN_POINT('Ctrl Pts',(0.360098980600512,-0.740622564981457,
-3.38029908532829));
#68737=CARTESIAN_POINT('Ctrl Pts',(0.671421347990293,-0.479890181544519,
-3.36441248683389));
#68738=CARTESIAN_POINT('Ctrl Pts',(0.817420588379709,-0.100083450714793,
-3.3485258883395));
#68739=CARTESIAN_POINT('Ctrl Pts',(0.752411610162823,0.440610915248839,
-3.32734375701365));
#68740=CARTESIAN_POINT('Ctrl Pts',(0.182737007354738,0.917575620846529,
-3.30086609285632));
#68741=CARTESIAN_POINT('Ctrl Pts',(-0.674755506495149,0.649111854550621,
-3.26909289586753));
#68742=CARTESIAN_POINT('Ctrl Pts',(-0.869117029466048,-0.0697848793019947,
-3.24261523171021));
#68743=CARTESIAN_POINT('Ctrl Pts',(-0.613439450643915,-0.548198276247722,
-3.22143310038435));
#68744=CARTESIAN_POINT('Ctrl Pts',(-0.164245468909761,-0.857028547702678,
-3.2002509690585));
#68745=CARTESIAN_POINT('Ctrl Pts',(0.42089853297893,-0.764159484363172,
-3.17906883773263));
#68746=CARTESIAN_POINT('Ctrl Pts',(0.753907947908702,-0.331384769821025,
-3.15788670640678));
#68747=CARTESIAN_POINT('Ctrl Pts',(0.822409257101771,0.0688783472016456,
-3.14200010791238));
#68748=CARTESIAN_POINT('Ctrl Pts',(0.687819729871631,0.452876511439188,
-3.12611350941799));
#68749=CARTESIAN_POINT('Ctrl Pts',(0.288250675822232,0.822905072066193,
-3.10493137809213));
#68750=CARTESIAN_POINT('Ctrl Pts',(-0.454714332566075,0.817662955983605,
-3.07845371393481));
#68751=CARTESIAN_POINT('Ctrl Pts',(-0.934496582127582,0.05794248230392,
-3.04668051694602));
#68752=CARTESIAN_POINT('Ctrl Pts',(-0.61725760748963,-0.615814408960401,
-3.0202028527887));
#68753=CARTESIAN_POINT('Ctrl Pts',(-0.112680433289495,-0.814943206389853,
-2.99902072146284));
#68754=CARTESIAN_POINT('Ctrl Pts',(0.429613118847823,-0.759543990660583,
-2.97783859013698));
#68755=CARTESIAN_POINT('Ctrl Pts',(0.815485490159638,-0.309965656073528,
-2.95665645881112));
#68756=CARTESIAN_POINT('Ctrl Pts',(0.789144447933524,0.235465708511735,
-2.93547432748526));
#68757=CARTESIAN_POINT('Ctrl Pts',(0.58224421809318,0.584887068909028,-2.91958772899087));
#68758=CARTESIAN_POINT('Ctrl Pts',(0.231079174441137,0.790440086631248,
-2.90370113049647));
#68759=CARTESIAN_POINT('Ctrl Pts',(-0.313007574327803,0.813810462059596,
-2.88251899917062));
#68760=CARTESIAN_POINT('Ctrl Pts',(-0.875895184041176,0.328854770989161,
-2.85604133501329));
#68761=CARTESIAN_POINT('Ctrl Pts',(-0.749773919115458,-0.560785398773811,
-2.82426813802451));
#68762=CARTESIAN_POINT('Ctrl Pts',(-0.0718191300318257,-0.868951294865558,
-2.79779047386718));
#68763=CARTESIAN_POINT('Ctrl Pts',(0.441671467773378,-0.694086179261763,
-2.77660834254133));
#68764=CARTESIAN_POINT('Ctrl Pts',(0.81913981644577,-0.300806360883462,
-2.75542621121547));
#68765=CARTESIAN_POINT('Ctrl Pts',(0.822212569948914,0.291653531478696,
-2.73424407988961));
#68766=CARTESIAN_POINT('Ctrl Pts',(0.449049354063659,0.690324371005584,
-2.71306194856375));
#68767=CARTESIAN_POINT('Ctrl Pts',(0.0651531347017874,0.822712757843502,
-2.69717535006936));
#68768=CARTESIAN_POINT('Ctrl Pts',(-0.335566880655414,0.752055838366545,
-2.68128875157496));
#68769=CARTESIAN_POINT('Ctrl Pts',(-0.765393673021599,0.417652648791717,
-2.66010662024911));
#68770=CARTESIAN_POINT('Ctrl Pts',(-0.880484198151439,-0.316362783263885,
-2.63362895609178));
#68771=CARTESIAN_POINT('Ctrl Pts',(-0.208445008845069,-0.912793444077713,
-2.601855759103));
#68772=CARTESIAN_POINT('Ctrl Pts',(0.507777844793081,-0.708798984638362,
-2.57537809494567));
#68773=CARTESIAN_POINT('Ctrl Pts',(0.785956306448284,-0.243109016783524,
-2.55419596361982));
#68774=CARTESIAN_POINT('Ctrl Pts',(0.819068571950472,0.301000299132349,
-2.53301383229395));
#68775=CARTESIAN_POINT('Ctrl Pts',(0.437880249640628,0.754556942570053,
-2.5118317009681));
#68776=CARTESIAN_POINT('Ctrl Pts',(-0.104621860425811,0.816852083250257,
-2.49064956964224));
#68777=CARTESIAN_POINT('Ctrl Pts',(-0.482925976241363,0.669241148130661,
-2.47476297114785));
#68778=CARTESIAN_POINT('Ctrl Pts',(-0.742611163852711,0.355980020135029,
-2.45887637265345));
#68779=CARTESIAN_POINT('Ctrl Pts',(-0.853744482606572,-0.177148435395509,
-2.4376942413276));
#68780=CARTESIAN_POINT('Ctrl Pts',(-0.466298755498204,-0.811112387064631,
-2.41121657717027));
#68781=CARTESIAN_POINT('Ctrl Pts',(0.432024176205328,-0.830660161821777,
-2.37944338018149));
#68782=CARTESIAN_POINT('Ctrl Pts',(0.845866350123333,-0.21152885858932,
-2.35296571602416));
#68783=CARTESIAN_POINT('Ctrl Pts',(0.756425889876396,0.323495259334638,
-2.33178358469831));
#68784=CARTESIAN_POINT('Ctrl Pts',(0.429433270552451,0.759645688316193,
-2.31060145337244));
#68785=CARTESIAN_POINT('Ctrl Pts',(-0.154715960077263,0.858579212596816,
-2.28941932204659));
#68786=CARTESIAN_POINT('Ctrl Pts',(-0.608532996475014,0.554869941328941,
-2.26823719072073));
#68787=CARTESIAN_POINT('Ctrl Pts',(-0.801316622834949,0.19746615620993,
-2.25235059222633));
#68788=CARTESIAN_POINT('Ctrl Pts',(-0.796455937755181,-0.209406434066689,
-2.23646399373194));
#68789=CARTESIAN_POINT('Ctrl Pts',(-0.536038735277689,-0.687694469969133,
-2.21528186240609));
#68790=CARTESIAN_POINT('Ctrl Pts',(0.169666939921909,-0.920082041628023,
-2.18880419824875));
#68791=CARTESIAN_POINT('Ctrl Pts',(0.867014727932226,-0.35344964961403,
-2.15703100125997));
#68792=CARTESIAN_POINT('Ctrl Pts',(0.781645283048855,0.386348277820098,
-2.13055333710265));
#68793=CARTESIAN_POINT('Ctrl Pts',(0.367125426573497,0.73623924837685,-2.10937120577679));
#68794=CARTESIAN_POINT('Ctrl Pts',(-0.164448381852627,0.856989635492053,
-2.08818907445093));
#68795=CARTESIAN_POINT('Ctrl Pts',(-0.673726417467051,0.554245439325413,
-2.06700694312507));
#68796=CARTESIAN_POINT('Ctrl Pts',(-0.82301466228896,0.0289814638455597,
-2.04582481179922));
#68797=CARTESIAN_POINT('Ctrl Pts',(-0.738586365580606,-0.368227366525561,
-2.02993821330482));
#68798=CARTESIAN_POINT('Ctrl Pts',(-0.471491638911371,-0.675195341994213,
-2.01405161481043));
#68799=CARTESIAN_POINT('Ctrl Pts',(0.0366168801367174,-0.871160383530664,
-1.99286948348457));
#68800=CARTESIAN_POINT('Ctrl Pts',(0.724935922390556,-0.591443777764724,
-1.96639181932725));
#68801=CARTESIAN_POINT('Ctrl Pts',(0.889637150329744,0.291868007868019,
-1.93461862233846));
#68802=CARTESIAN_POINT('Ctrl Pts',(0.345659362638246,0.800471077121211,
-1.90814095818114));
#68803=CARTESIAN_POINT('Ctrl Pts',(-0.196786632712784,0.798814328159457,
-1.88695882685528));
#68804=CARTESIAN_POINT('Ctrl Pts',(-0.680115363374823,0.546733571437031,
-1.86577669552942));
#68805=CARTESIAN_POINT('Ctrl Pts',(-0.872300216170217,-0.0136976448847273,
-1.84459456420356));
#68806=CARTESIAN_POINT('Ctrl Pts',(-0.64605543815613,-0.510691130154158,
-1.82341243287771));
#68807=CARTESIAN_POINT('Ctrl Pts',(-0.324570867014354,-0.758785190396783,
-1.80752583438331));
#68808=CARTESIAN_POINT('Ctrl Pts',(0.0777227434299177,-0.819848943749846,
-1.79163923588892));
#68809=CARTESIAN_POINT('Ctrl Pts',(0.591856834804682,-0.640286417815664,
-1.77045710456306));
#68810=CARTESIAN_POINT('Ctrl Pts',(0.93541206505034,0.0184960100323257,
-1.74397944040574));
#68811=CARTESIAN_POINT('Ctrl Pts',(0.489131803792666,0.798367879979027,
-1.71220624341694));
#68812=CARTESIAN_POINT('Ctrl Pts',(-0.254728499474417,0.833875129646275,
-1.68572857925963));
#68813=CARTESIAN_POINT('Ctrl Pts',(-0.66710335504059,0.481458641402219,
-1.66454644793376));
#68814=CARTESIAN_POINT('Ctrl Pts',(-0.872306986188969,-0.0235590212162755,
-1.64336431660791));
#68815=CARTESIAN_POINT('Ctrl Pts',(-0.655992010257842,-0.575125877598879,
-1.62218218528205));
#68816=CARTESIAN_POINT('Ctrl Pts',(-0.161820381338305,-0.807469642632321,
-1.60100005395619));
#68817=CARTESIAN_POINT('Ctrl Pts',(0.243816497396363,-0.788450840875503,
-1.5851134554618));
#68818=CARTESIAN_POINT('Ctrl Pts',(0.589970761438499,-0.574567329441633,
-1.5692268569674));
#68819=CARTESIAN_POINT('Ctrl Pts',(0.865598808023936,-0.104880471450991,
-1.54804472564155));
#68820=CARTESIAN_POINT('Ctrl Pts',(0.700989048572545,0.619638755736126,
-1.52156706148422));
#68821=CARTESIAN_POINT('Ctrl Pts',(-0.144013612661718,0.925149324504857,
-1.48979386449544));
#68822=CARTESIAN_POINT('Ctrl Pts',(-0.733962808560724,0.470672854471897,
-1.46331620033811));
#68823=CARTESIAN_POINT('Ctrl Pts',(-0.82013346881962,-0.0648876183040882,
-1.44213406901226));
#68824=CARTESIAN_POINT('Ctrl Pts',(-0.649613384442308,-0.582646510663345,
-1.42095193768639));
#68825=CARTESIAN_POINT('Ctrl Pts',(-0.127681955460861,-0.863013679413998,
-1.39976980636054));
#68826=CARTESIAN_POINT('Ctrl Pts',(0.399379421048456,-0.720200762032534,
-1.37858767503468));
#68827=CARTESIAN_POINT('Ctrl Pts',(0.696240257393158,-0.443114789715985,
-1.36270107654028));
#68828=CARTESIAN_POINT('Ctrl Pts',(0.821617849133442,-0.0560109399970021,
-1.34681447804589));
#68829=CARTESIAN_POINT('Ctrl Pts',(0.72764608942882,0.48040855350751,-1.32563234672003));
#68830=CARTESIAN_POINT('Ctrl Pts',(0.133162765313291,0.926069928117188,
-1.29915468256271));
#68831=CARTESIAN_POINT('Ctrl Pts',(-0.708663509792098,0.611912757795438,
-1.26738148557392));
#68832=CARTESIAN_POINT('Ctrl Pts',(-0.864110924976073,-0.116390075281674,
-1.2409038214166));
#68833=CARTESIAN_POINT('Ctrl Pts',(-0.583093041185656,-0.580372134934255,
-1.21972169009074));
#68834=CARTESIAN_POINT('Ctrl Pts',(-0.117951725407047,-0.864616617992188,
-1.19853955876488));
#68835=CARTESIAN_POINT('Ctrl Pts',(0.461355982526874,-0.7404363240635,-1.17735742743902));
#68836=CARTESIAN_POINT('Ctrl Pts',(0.770627035260557,-0.290391170862284,
-1.15617529611317));
#68837=CARTESIAN_POINT('Ctrl Pts',(0.817519362915898,0.112974794257399,
-1.14028869761877));
#68838=CARTESIAN_POINT('Ctrl Pts',(0.66248839687407,0.48918528128025,-1.12440209912438));
#68839=CARTESIAN_POINT('Ctrl Pts',(0.243611525802989,0.837206446606919,
-1.10321996779852));
#68840=CARTESIAN_POINT('Ctrl Pts',(-0.497998174970216,0.79204523327596,
-1.0767423036412));
#68841=CARTESIAN_POINT('Ctrl Pts',(-0.936260025425832,0.00763924428965602,
-1.04496910665241));
#68842=CARTESIAN_POINT('Ctrl Pts',(-0.583272014082999,-0.648095747459154,
-1.01849144249509));
#68843=CARTESIAN_POINT('Ctrl Pts',(-0.0687228533155248,-0.819821004317041,
-0.997309311169228));
#68844=CARTESIAN_POINT('Ctrl Pts',(0.469809940687286,-0.735359181126046,
-0.976127179843371));
#68845=CARTESIAN_POINT('Ctrl Pts',(0.830964541358147,-0.265693853167689,
-0.954945048517511));
#68846=CARTESIAN_POINT('Ctrl Pts',(0.775350277160346,0.277533794873319,
-0.933762917191653));
#68847=CARTESIAN_POINT('Ctrl Pts',(0.549971243807159,0.615331491039807,
-0.917876318697261));
#68848=CARTESIAN_POINT('Ctrl Pts',(0.188267294934982,0.801715997764048,
-0.901989720202864));
#68849=CARTESIAN_POINT('Ctrl Pts',(-0.356289153983751,0.795813576474891,
-0.880807588877008));
#68850=CARTESIAN_POINT('Ctrl Pts',(-0.892302036349828,0.281309277747789,
-0.854329924719686));
#68851=CARTESIAN_POINT('Ctrl Pts',(-0.718554076398238,-0.600267634106091,
-0.822556727730897));
#68852=CARTESIAN_POINT('Ctrl Pts',(-0.0250182201471705,-0.871555178383084,
-0.796079063573576));
#68853=CARTESIAN_POINT('Ctrl Pts',(0.478333185832665,-0.669347946128884,
-0.774896932247718));
#68854=CARTESIAN_POINT('Ctrl Pts',(0.834121369879876,-0.256351411186756,
-0.75371480092186));
#68855=CARTESIAN_POINT('Ctrl Pts',(0.805351101674305,0.335417494451096,
-0.732532669596));
#68856=CARTESIAN_POINT('Ctrl Pts',(0.411302686227501,0.713458590124914,
-0.711350538270145));
#68857=CARTESIAN_POINT('Ctrl Pts',(0.0208466994859789,0.825025228897732,
-0.695463939775747));
#68858=CARTESIAN_POINT('Ctrl Pts',(-0.375497190132326,0.732935859991011,
-0.679577341281356));
#68859=CARTESIAN_POINT('Ctrl Pts',(-0.786732168724632,0.375917153191761,
-0.658395209955497));
#68860=CARTESIAN_POINT('Ctrl Pts',(-0.86221065869004,-0.363222538767329,
-0.631917545798175));
#68861=CARTESIAN_POINT('Ctrl Pts',(-0.159090613120796,-0.922676197632793,
-0.600144348809385));
#68862=CARTESIAN_POINT('Ctrl Pts',(0.545134702812622,-0.680486963024897,
-0.573666684652064));
#68863=CARTESIAN_POINT('Ctrl Pts',(0.797885170775076,-0.20052070441559,
-0.552484553326204));
#68864=CARTESIAN_POINT('Ctrl Pts',(0.801709368724974,0.344581782361119,
-0.531302422000347));
#68865=CARTESIAN_POINT('Ctrl Pts',(0.396697857986909,0.776998153601058,
-0.510120290674489));
#68866=CARTESIAN_POINT('Ctrl Pts',(-0.14836798230013,0.81004933530726,-0.48893815934863));
#68867=CARTESIAN_POINT('Ctrl Pts',(-0.518192989793109,0.642321898247082,
-0.473051560854238));
#68868=CARTESIAN_POINT('Ctrl Pts',(-0.760668183767484,0.315557812215962,
-0.457164962359843));
#68869=CARTESIAN_POINT('Ctrl Pts',(-0.842991196767877,-0.222772042303558,
-0.435982831033984));
#68870=CARTESIAN_POINT('Ctrl Pts',(-0.42203547005247,-0.834999727972205,
-0.409505166876662));
#68871=CARTESIAN_POINT('Ctrl Pts',(0.476038245560472,-0.80624182046484,
-0.377731969887874));
#68872=CARTESIAN_POINT('Ctrl Pts',(0.856013262987149,-0.165768651945676,
-0.351254305730552));
#68873=CARTESIAN_POINT('Ctrl Pts',(0.737946030751173,0.363680533637555,
-0.330072174404693));
#68874=CARTESIAN_POINT('Ctrl Pts',(0.387995544781613,0.781618685293715,
-0.308890043078836));
#68875=CARTESIAN_POINT('Ctrl Pts',(-0.200644125565596,0.849038180119929,
-0.287707911752977));
#68876=CARTESIAN_POINT('Ctrl Pts',(-0.637457343762986,0.521348487027652,
-0.266525780427118));
#68877=CARTESIAN_POINT('Ctrl Pts',(-0.810801308960607,0.154154372617482,
-0.250639181932725));
#68878=CARTESIAN_POINT('Ctrl Pts',(-0.783995360021825,-0.251970803616545,
-0.23475258343833));
#68879=CARTESIAN_POINT('Ctrl Pts',(-0.498429251676069,-0.715365288338213,
-0.213570452112473));
#68880=CARTESIAN_POINT('Ctrl Pts',(0.219118145102592,-0.909928416986752,
-0.187092787955149));
#68881=CARTESIAN_POINT('Ctrl Pts',(0.884316580820022,-0.305832475245307,
-0.155319590966362));
#68882=CARTESIAN_POINT('Ctrl Pts',(0.760492323845775,0.426932666048197,
-0.128841926809039));
#68883=CARTESIAN_POINT('Ctrl Pts',(0.32603470475945,0.756065290736446,-0.107659795483181));
#68884=CARTESIAN_POINT('Ctrl Pts',(-0.0741110827836955,0.821794729598117,
-0.0917731969887856));
#68885=CARTESIAN_POINT('Ctrl Pts',(-0.459293844256021,0.685000114437588,
-0.0758865984943949));
#68886=CARTESIAN_POINT('Ctrl Pts',(-0.640103745128917,0.483143622270636,
-0.0652955328314636));
#68887=CARTESIAN_POINT('Ctrl Pts',(-0.701077753000047,0.366509473613445,
-0.0599999999999987));
#68888=CARTESIAN_POINT('Ctrl Pts',(0.437168237015721,-0.613060138694139,
-11.9529325805302));
#68889=CARTESIAN_POINT('Ctrl Pts',(0.539159417089925,-0.540331051333857,
-11.9476370476987));
#68890=CARTESIAN_POINT('Ctrl Pts',(0.705834142587216,-0.343484520089658,
-11.9370459820358));
#68891=CARTESIAN_POINT('Ctrl Pts',(0.784458452235278,0.0375372744664799,
-11.9211593835414));
#68892=CARTESIAN_POINT('Ctrl Pts',(0.670191340654958,0.406196224080167,
-11.905272785047));
#68893=CARTESIAN_POINT('Ctrl Pts',(0.303108267623569,0.772777165643128,
-11.8840906537212));
#68894=CARTESIAN_POINT('Ctrl Pts',(-0.403912271093399,0.793744592728965,
-11.8576129895638));
#68895=CARTESIAN_POINT('Ctrl Pts',(-0.886501473350934,0.0876535971293119,
-11.8258397925751));
#68896=CARTESIAN_POINT('Ctrl Pts',(-0.609288364385278,-0.563407023952644,
-11.7993621284177));
#68897=CARTESIAN_POINT('Ctrl Pts',(-0.135085777497467,-0.772068029013216,
-11.7781799970919));
#68898=CARTESIAN_POINT('Ctrl Pts',(0.251304709598349,-0.74425999429876,
-11.7622933985975));
#68899=CARTESIAN_POINT('Ctrl Pts',(0.574832343924073,-0.532842736520013,
-11.7464068001031));
#68900=CARTESIAN_POINT('Ctrl Pts',(0.8266807971614,-0.0781949429499539,
-11.7252246687772));
#68901=CARTESIAN_POINT('Ctrl Pts',(0.686184366139097,0.467951511691284,
-11.7040425374514));
#68902=CARTESIAN_POINT('Ctrl Pts',(0.246422156911299,0.743253963547303,
-11.6828604061255));
#68903=CARTESIAN_POINT('Ctrl Pts',(-0.268163586381898,0.785366976684619,
-11.6616782747996));
#68904=CARTESIAN_POINT('Ctrl Pts',(-0.82232695935117,0.343424645220471,
-11.6352006106423));
#68905=CARTESIAN_POINT('Ctrl Pts',(-0.732061997464235,-0.507020546474788,
-11.6034274136535));
#68906=CARTESIAN_POINT('Ctrl Pts',(-0.0998470505031248,-0.823871915212379,
-11.5769497494962));
#68907=CARTESIAN_POINT('Ctrl Pts',(0.396920405700097,-0.675900179016633,
-11.5557676181703));
#68908=CARTESIAN_POINT('Ctrl Pts',(0.673296005380202,-0.404591498794211,
-11.539881019676));
#68909=CARTESIAN_POINT('Ctrl Pts',(0.783090425855826,-0.0340058084353497,
-11.5239944211816));
#68910=CARTESIAN_POINT('Ctrl Pts',(0.680690834182767,0.47555198557487,-11.5028122898557));
#68911=CARTESIAN_POINT('Ctrl Pts',(0.220082416614076,0.800872619360714,
-11.4816301585298));
#68912=CARTESIAN_POINT('Ctrl Pts',(-0.293329865373632,0.726022874064885,
-11.460448027204));
#68913=CARTESIAN_POINT('Ctrl Pts',(-0.712798547359122,0.425003488822047,
-11.4392658958781));
#68914=CARTESIAN_POINT('Ctrl Pts',(-0.849088317678126,-0.270580441077998,
-11.4127882317208));
#68915=CARTESIAN_POINT('Ctrl Pts',(-0.229749102076862,-0.860348396266937,
-11.381015034732));
#68916=CARTESIAN_POINT('Ctrl Pts',(0.457232564597481,-0.692583893641502,
-11.3545373705747));
#68917=CARTESIAN_POINT('Ctrl Pts',(0.740074896800098,-0.258217496975165,
-11.3333552392488));
#68918=CARTESIAN_POINT('Ctrl Pts',(0.775093214744087,0.127483861482161,
-11.3174686407544));
#68919=CARTESIAN_POINT('Ctrl Pts',(0.618878123555508,0.481016576484203,
-11.3015820422601));
#68920=CARTESIAN_POINT('Ctrl Pts',(0.210966531938114,0.80310821135501,-11.2803999109342));
#68921=CARTESIAN_POINT('Ctrl Pts',(-0.350702013875208,0.75288864389604,
-11.2592177796083));
#68922=CARTESIAN_POINT('Ctrl Pts',(-0.693566003923817,0.363480166947511,
-11.2380356482825));
#68923=CARTESIAN_POINT('Ctrl Pts',(-0.81841553912867,-0.137498109807854,
-11.2168535169566));
#68924=CARTESIAN_POINT('Ctrl Pts',(-0.472006417340506,-0.755893307477461,
-11.1903758527993));
#68925=CARTESIAN_POINT('Ctrl Pts',(0.381835965208045,-0.804478284119145,
-11.1586026558105));
#68926=CARTESIAN_POINT('Ctrl Pts',(0.796844322343783,-0.231890474878377,
-11.1321249916532));
#68927=CARTESIAN_POINT('Ctrl Pts',(0.731236012504642,0.282278272840807,
-11.1109428603273));
#68928=CARTESIAN_POINT('Ctrl Pts',(0.508241943232004,0.598925498983947,
-11.0950562618329));
#68929=CARTESIAN_POINT('Ctrl Pts',(0.160315976071488,0.767258669906312,
-11.0791696633385));
#68930=CARTESIAN_POINT('Ctrl Pts',(-0.359097293392396,0.748691398822516,
-11.0579875320127));
#68931=CARTESIAN_POINT('Ctrl Pts',(-0.754686142027795,0.346817011706505,
-11.0368054006868));
#68932=CARTESIAN_POINT('Ctrl Pts',(-0.763929405500613,-0.171940387934335,
-11.015623269361));
#68933=CARTESIAN_POINT('Ctrl Pts',(-0.534779073333243,-0.634603078779137,
-10.9944411380351));
#68934=CARTESIAN_POINT('Ctrl Pts',(0.129570407511939,-0.881689435003545,
-10.9679634738778));
#68935=CARTESIAN_POINT('Ctrl Pts',(0.811812832458132,-0.365983522865465,
-10.936190276889));
#68936=CARTESIAN_POINT('Ctrl Pts',(0.757462285313874,0.339094312418124,
-10.9097126127317));
#68937=CARTESIAN_POINT('Ctrl Pts',(0.374607849449645,0.688517311643914,
-10.8885304814058));
#68938=CARTESIAN_POINT('Ctrl Pts',(-0.000338531309959313,0.78550716838858,
-10.8726438829114));
#68939=CARTESIAN_POINT('Ctrl Pts',(-0.374495394303978,0.688578447509876,
-10.856757284417));
#68940=CARTESIAN_POINT('Ctrl Pts',(-0.758367850255281,0.338183205514494,
-10.8355751530912));
#68941=CARTESIAN_POINT('Ctrl Pts',(-0.799727679520165,-0.224207161319477,
-10.8143930217653));
#68942=CARTESIAN_POINT('Ctrl Pts',(-0.47095395048083,-0.62558293624273,
-10.7932108904395));
#68943=CARTESIAN_POINT('Ctrl Pts',(0.00320814217882656,-0.829879167526741,
-10.7720287591136));
#68944=CARTESIAN_POINT('Ctrl Pts',(0.669521166699254,-0.588137872986708,
-10.7455510949563));
#68945=CARTESIAN_POINT('Ctrl Pts',(0.855676605772496,0.246579723996904,
-10.7137778979675));
#68946=CARTESIAN_POINT('Ctrl Pts',(0.357817272849018,0.748799616478352,
-10.6873002338102));
#68947=CARTESIAN_POINT('Ctrl Pts',(-0.160190687341481,0.767284870821596,
-10.6661181024843));
#68948=CARTESIAN_POINT('Ctrl Pts',(-0.508757994142515,0.598487200856775,
-10.6502315039899));
#68949=CARTESIAN_POINT('Ctrl Pts',(-0.731189876677205,0.282397668146848,
-10.6343449054955));
#68950=CARTESIAN_POINT('Ctrl Pts',(-0.796944728362207,-0.233171131850758,
-10.6131627741697));
#68951=CARTESIAN_POINT('Ctrl Pts',(-0.464404043789838,-0.688594290340323,
-10.5919806428438));
#68952=CARTESIAN_POINT('Ctrl Pts',(0.0460158535429895,-0.781686749800895,
-10.5707985115179));
#68953=CARTESIAN_POINT('Ctrl Pts',(0.539669506345693,-0.630449481554002,
-10.5496163801921));
#68954=CARTESIAN_POINT('Ctrl Pts',(0.891035361704283,-0.0148571360691248,
-10.5231387160348));
#68955=CARTESIAN_POINT('Ctrl Pts',(0.492564868907406,0.741865125121111,
-10.491365519046));
#68956=CARTESIAN_POINT('Ctrl Pts',(-0.212012206722167,0.802362069509788,
-10.4648878548886));
#68957=CARTESIAN_POINT('Ctrl Pts',(-0.618799590961628,0.481117652480525,
-10.4437057235628));
#68958=CARTESIAN_POINT('Ctrl Pts',(-0.775202810447137,0.126815727999937,
-10.4278191250684));
#68959=CARTESIAN_POINT('Ctrl Pts',(-0.74011702371455,-0.258096629071203,
-10.411932526574));
#68960=CARTESIAN_POINT('Ctrl Pts',(-0.456480055932384,-0.693624996182262,
-10.3907503952481));
#68961=CARTESIAN_POINT('Ctrl Pts',(0.0917986850181122,-0.825473327253274,
-10.3695682639223));
#68962=CARTESIAN_POINT('Ctrl Pts',(0.541099672434501,-0.56600598767403,
-10.3483861325964));
#68963=CARTESIAN_POINT('Ctrl Pts',(0.81945414101959,-0.131166442495638,
-10.3272040012706));
#68964=CARTESIAN_POINT('Ctrl Pts',(0.688756772763614,0.565489927648501,
-10.3007263371132));
#68965=CARTESIAN_POINT('Ctrl Pts',(-0.104819766699716,0.884305846673958,
-10.2689531401245));
#68966=CARTESIAN_POINT('Ctrl Pts',(-0.681004786683215,0.474306385052725,
-10.2424754759671));
#68967=CARTESIAN_POINT('Ctrl Pts',(-0.783096043438991,-0.0338779582154253,
-10.2212933446413));
#68968=CARTESIAN_POINT('Ctrl Pts',(-0.672946931715876,-0.405171634356951,
-10.2054067461469));
#68969=CARTESIAN_POINT('Ctrl Pts',(-0.397030920317412,-0.675835428963228,
-10.1895201476525));
#68970=CARTESIAN_POINT('Ctrl Pts',(0.101094915407747,-0.824178072306936,
-10.1683380163266));
#68971=CARTESIAN_POINT('Ctrl Pts',(0.604340273136911,-0.569742088003379,
-10.1471558850008));
#68972=CARTESIAN_POINT('Ctrl Pts',(0.778826548572907,-0.0811223818042267,
-10.1259737536749));
#68973=CARTESIAN_POINT('Ctrl Pts',(0.709491335059612,0.430501765787835,
-10.1047916223491));
#68974=CARTESIAN_POINT('Ctrl Pts',(0.158892812090172,0.876879595249961,
-10.0783139581917));
#68975=CARTESIAN_POINT('Ctrl Pts',(-0.652350196007727,0.606154465232593,
-10.046540761203));
#68976=CARTESIAN_POINT('Ctrl Pts',(-0.826098981874427,-0.0793381278659279,
-10.0200630970456));
#68977=CARTESIAN_POINT('Ctrl Pts',(-0.574937634292116,-0.532760589737299,
-9.99888096571977));
#68978=CARTESIAN_POINT('Ctrl Pts',(-0.250625132038328,-0.744451925502288,
-9.98299436722538));
#68979=CARTESIAN_POINT('Ctrl Pts',(0.134890381171093,-0.772134485564218,
-9.96710776873098));
#68980=CARTESIAN_POINT('Ctrl Pts',(0.610587288138713,-0.56273691931158,
-9.94592563740513));
#68981=CARTESIAN_POINT('Ctrl Pts',(0.829446527249074,-0.0430310470718053,
-9.92474350607925));
#68982=CARTESIAN_POINT('Ctrl Pts',(0.646129213264504,0.442344518851281,
-9.90356137475341));
#68983=CARTESIAN_POINT('Ctrl Pts',(0.262081418700829,0.787415427104953,
-9.88237924342756));
#68984=CARTESIAN_POINT('Ctrl Pts',(-0.446543488446261,0.771209221434691,
-9.85590157927021));
#68985=CARTESIAN_POINT('Ctrl Pts',(-0.889610890178794,0.0397048867020595,
-9.82412838228145));
#68986=CARTESIAN_POINT('Ctrl Pts',(-0.578285328073375,-0.595247969943875,
-9.7976507181241));
#68987=CARTESIAN_POINT('Ctrl Pts',(-0.0933283262204505,-0.778252499403336,
-9.77646858679826));
#68988=CARTESIAN_POINT('Ctrl Pts',(0.29089858374514,-0.729657207302419,
-9.76058198830386));
#68989=CARTESIAN_POINT('Ctrl Pts',(0.60265533980172,-0.501192198800497,
-9.74469538980948));
#68990=CARTESIAN_POINT('Ctrl Pts',(0.829673131787345,-0.0336477515304431,
-9.72351325848361));
#68991=CARTESIAN_POINT('Ctrl Pts',(0.660052778303402,0.504146350211528,
-9.70233112715774));
#68992=CARTESIAN_POINT('Ctrl Pts',(0.206120956474527,0.755424241663983,
-9.6811489958319));
#68993=CARTESIAN_POINT('Ctrl Pts',(-0.309979234121676,0.769819848590857,
-9.65996686450603));
#68994=CARTESIAN_POINT('Ctrl Pts',(-0.839595504076748,0.298737576869337,
-9.63348920034872));
#68995=CARTESIAN_POINT('Ctrl Pts',(-0.703756305225402,-0.545629065215758,
-9.60171600335992));
#68996=CARTESIAN_POINT('Ctrl Pts',(-0.0554285506970736,-0.828046944414903,
-9.5752383392026));
#68997=CARTESIAN_POINT('Ctrl Pts',(0.432669647991569,-0.653593225951356,
-9.55405620787675));
#68998=CARTESIAN_POINT('Ctrl Pts',(0.694065590076106,-0.367824119472337,
-9.53816960938235));
#68999=CARTESIAN_POINT('Ctrl Pts',(0.78378634966761,0.00812630326319978,
-9.52228301088796));
#69000=CARTESIAN_POINT('Ctrl Pts',(0.65415119509764,0.511444904897103,-9.5011008795621));
#69001=CARTESIAN_POINT('Ctrl Pts',(0.176725804605299,0.811542483523972,
-9.47991874823624));
#69002=CARTESIAN_POINT('Ctrl Pts',(-0.331922213101395,0.709210320033098,
-9.45873661691039));
#69003=CARTESIAN_POINT('Ctrl Pts',(-0.734608069712466,0.386083810570246,
-9.43755448558453));
#69004=CARTESIAN_POINT('Ctrl Pts',(-0.833320476860817,-0.315819146259562,
-9.4110768214272));
#69005=CARTESIAN_POINT('Ctrl Pts',(-0.183182295399402,-0.871451811980982,
-9.37930362443841));
#69006=CARTESIAN_POINT('Ctrl Pts',(0.493791063463925,-0.667011583130608,
-9.35282596028109));
#69007=CARTESIAN_POINT('Ctrl Pts',(0.752881990642999,-0.218073009490135,
-9.33164382895524));
#69008=CARTESIAN_POINT('Ctrl Pts',(0.76712225365182,0.168952875516953,-9.31575723046083));
#69009=CARTESIAN_POINT('Ctrl Pts',(0.592134175587876,0.513579786236636,
-9.29987063196645));
#69010=CARTESIAN_POINT('Ctrl Pts',(0.167502935024326,0.81328497069054,-9.27868850064059));
#69011=CARTESIAN_POINT('Ctrl Pts',(-0.39065520774003,0.732954105823305,
-9.25750636931472));
#69012=CARTESIAN_POINT('Ctrl Pts',(-0.712097081609459,0.325682943911511,
-9.23632423798888));
#69013=CARTESIAN_POINT('Ctrl Pts',(-0.809843814576814,-0.181280779077073,
-9.21514210666301));
#69014=CARTESIAN_POINT('Ctrl Pts',(-0.430702924997686,-0.780166482680521,
-9.18866444250569));
#69015=CARTESIAN_POINT('Ctrl Pts',(0.424516578683828,-0.782796070745956,
-9.15689124551691));
#69016=CARTESIAN_POINT('Ctrl Pts',(0.808154578229917,-0.188733261703544,
-9.13041358135957));
#69017=CARTESIAN_POINT('Ctrl Pts',(0.715009830130715,0.321166735698292,
-9.10923145003374));
#69018=CARTESIAN_POINT('Ctrl Pts',(0.475321483421555,0.625372779701216,
-9.09334485153931));
#69019=CARTESIAN_POINT('Ctrl Pts',(0.118852111688952,0.77476528979884,-9.07745825304495));
#69020=CARTESIAN_POINT('Ctrl Pts',(-0.39881279752422,0.728311766569634,
-9.05627612171906));
#69021=CARTESIAN_POINT('Ctrl Pts',(-0.772233428000458,0.305759293000729,
-9.03509399039322));
#69022=CARTESIAN_POINT('Ctrl Pts',(-0.753585498799065,-0.21274522225268,
-9.01391185906737));
#69023=CARTESIAN_POINT('Ctrl Pts',(-0.499902966579275,-0.662424900555796,
-8.99272972774149));
#69024=CARTESIAN_POINT('Ctrl Pts',(0.176764848846763,-0.873452310382106,
-8.96625206358418));
#69025=CARTESIAN_POINT('Ctrl Pts',(0.830307570719126,-0.321828140409187,
-8.93447886659539));
#69026=CARTESIAN_POINT('Ctrl Pts',(0.738144931967327,0.379310065511296,
-8.90800120243806));
#69027=CARTESIAN_POINT('Ctrl Pts',(0.33706586160392,0.707653682420898,-8.88681907111222));
#69028=CARTESIAN_POINT('Ctrl Pts',(-0.0425509146991354,0.784353903446371,
-8.87093247261781));
#69029=CARTESIAN_POINT('Ctrl Pts',(-0.410958199522342,0.667458191181559,
-8.85504587412343));
#69030=CARTESIAN_POINT('Ctrl Pts',(-0.775445838453558,0.29694010914313,
-8.83386374279756));
#69031=CARTESIAN_POINT('Ctrl Pts',(-0.786523246056195,-0.26686025554749,
-8.81268161147171));
#69032=CARTESIAN_POINT('Ctrl Pts',(-0.436654811424381,-0.6499878531569,
-8.79149948014584));
#69033=CARTESIAN_POINT('Ctrl Pts',(0.047800914194124,-0.82850757236933,
-8.77031734881999));
#69034=CARTESIAN_POINT('Ctrl Pts',(0.700160013885623,-0.551308176300101,
-8.74383968466266));
#69035=CARTESIAN_POINT('Ctrl Pts',(0.841189031607181,0.292207164622127,
-8.71206648767388));
#69036=CARTESIAN_POINT('Ctrl Pts',(0.317059998327239,0.766946558664921,
-8.68558882351655));
#69037=CARTESIAN_POINT('Ctrl Pts',(-0.201192821693523,0.757567540092399,
-8.6644066921907));
#69038=CARTESIAN_POINT('Ctrl Pts',(-0.540185316243243,0.570281904244278,
-8.6485200936963));
#69039=CARTESIAN_POINT('Ctrl Pts',(-0.745309242845801,0.242695717429499,
-8.63263349520192));
#69040=CARTESIAN_POINT('Ctrl Pts',(-0.783262595763387,-0.275661718181675,
-8.61145136387603));
#69041=CARTESIAN_POINT('Ctrl Pts',(-0.426728161974488,-0.71255616505334,
-8.5902692325502));
#69042=CARTESIAN_POINT('Ctrl Pts',(0.0879569244362535,-0.778084322573904,
-8.56908710122433));
#69043=CARTESIAN_POINT('Ctrl Pts',(0.572769802202764,-0.600536825311924,
-8.54790496989848));
#69044=CARTESIAN_POINT('Ctrl Pts',(0.890546216267256,0.0330482524761829,
-8.52142730574115));
#69045=CARTESIAN_POINT('Ctrl Pts',(0.451985538686537,0.767263375100736,
-8.48965410875238));
#69046=CARTESIAN_POINT('Ctrl Pts',(-0.254824494055272,0.789809181775388,
-8.46317644459503));
#69047=CARTESIAN_POINT('Ctrl Pts',(-0.643760503623392,0.447168361221148,
-8.44199431326919));
#69048=CARTESIAN_POINT('Ctrl Pts',(-0.780897659633066,0.0849733568413833,
-8.42610771477479));
#69049=CARTESIAN_POINT('Ctrl Pts',(-0.725177520948885,-0.297497297198533,
-8.41022111628039));
#69050=CARTESIAN_POINT('Ctrl Pts',(-0.418545276104388,-0.717153769176163,
-8.38903898495455));
#69051=CARTESIAN_POINT('Ctrl Pts',(0.136026673789023,-0.819347274722716,
-8.36785685362867));
#69052=CARTESIAN_POINT('Ctrl Pts',(0.570734731503279,-0.536109596861927,
-8.34667472230283));
#69053=CARTESIAN_POINT('Ctrl Pts',(0.825318852045567,-0.0869397338925285,
-8.32549259097696));
#69054=CARTESIAN_POINT('Ctrl Pts',(0.657372281257338,0.601686325367446,
-8.29901492681965));
#69055=CARTESIAN_POINT('Ctrl Pts',(-0.15219057819013,0.877395031820266,
-8.26724172983084));
#69056=CARTESIAN_POINT('Ctrl Pts',(-0.705509776625659,0.437024051366566,
-8.24076406567354));
#69057=CARTESIAN_POINT('Ctrl Pts',(-0.780143865883835,-0.0759123035250102,
-8.21958193434766));
#69058=CARTESIAN_POINT('Ctrl Pts',(-0.650200733115148,-0.440750079806934,
-8.20369533585329));
#69059=CARTESIAN_POINT('Ctrl Pts',(-0.360138050531249,-0.696195133055061,
-8.18780873735887));
#69060=CARTESIAN_POINT('Ctrl Pts',(0.145239864419022,-0.817554315367743,
-8.16662660603304));
#69061=CARTESIAN_POINT('Ctrl Pts',(0.634084725054934,-0.536441771331854,
-8.14544447470716));
#69062=CARTESIAN_POINT('Ctrl Pts',(0.782060617407885,-0.0391512999934004,
-8.12426234338132));
#69063=CARTESIAN_POINT('Ctrl Pts',(0.685331096971596,0.468007491814848,
-8.10308021205544));
#69064=CARTESIAN_POINT('Ctrl Pts',(0.111540015123584,0.8841513305571,-8.07660254789814));
#69065=CARTESIAN_POINT('Ctrl Pts',(-0.683982060748652,0.570221496023044,
-8.04482935090934));
#69066=CARTESIAN_POINT('Ctrl Pts',(-0.820641651118927,-0.123617744826675,
-8.01835168675202));
#69067=CARTESIAN_POINT('Ctrl Pts',(-0.545476476388819,-0.562887682410165,
-7.99716955542616));
#69068=CARTESIAN_POINT('Ctrl Pts',(-0.210256395491838,-0.756844683107489,
-7.98128295693177));
#69069=CARTESIAN_POINT('Ctrl Pts',(0.176189691484825,-0.763769776401557,
-7.96539635843737));
#69070=CARTESIAN_POINT('Ctrl Pts',(0.639946257759712,-0.529111012900144,
-7.94421422711152));
#69071=CARTESIAN_POINT('Ctrl Pts',(0.830560434656543,0.00160529149460393,
-7.92303209578566));
#69072=CARTESIAN_POINT('Ctrl Pts',(0.621424109326631,0.476428074255893,
-7.90184996445979));
#69073=CARTESIAN_POINT('Ctrl Pts',(0.219387284491965,0.800361758378271,
-7.88066783313394));
#69074=CARTESIAN_POINT('Ctrl Pts',(-0.487342730892537,0.746097723455757,
-7.85419016897662));
#69075=CARTESIAN_POINT('Ctrl Pts',(-0.890459112307306,-0.00815985671544194,
-7.82241697198783));
#69076=CARTESIAN_POINT('Ctrl Pts',(-0.545461283363713,-0.625464671055404,
-7.7959393078305));
#69077=CARTESIAN_POINT('Ctrl Pts',(-0.0513704557899223,-0.78214334081074,
-7.77475717650466));
#69078=CARTESIAN_POINT('Ctrl Pts',(0.329689745670944,-0.712970053924232,
-7.75887057801024));
#69079=CARTESIAN_POINT('Ctrl Pts',(0.628718380100739,-0.468081485698276,
-7.74298397951587));
#69080=CARTESIAN_POINT('Ctrl Pts',(0.830282456821142,0.0109872056466471,
-7.72180184818998));
#69081=CARTESIAN_POINT('Ctrl Pts',(0.632006346377846,0.538888848201348,
-7.70061971686417));
#69082=CARTESIAN_POINT('Ctrl Pts',(0.165226880962859,0.765409505688858,
-7.67943758553827));
#69083=CARTESIAN_POINT('Ctrl Pts',(-0.350901150045432,0.752049272167661,
-7.65825545421243));
#69084=CARTESIAN_POINT('Ctrl Pts',(-0.854436322923102,0.253186335273663,
-7.6317777900551));
#69085=CARTESIAN_POINT('Ctrl Pts',(-0.673417454717608,-0.582660231725479,
-7.60000459306631));
#69086=CARTESIAN_POINT('Ctrl Pts',(-0.010849510586414,-0.829829111629177,
-7.573526928909));
#69087=CARTESIAN_POINT('Ctrl Pts',(0.467168297119543,-0.629397260455649,
-7.55234479758313));
#69088=CARTESIAN_POINT('Ctrl Pts',(0.712829388280181,-0.329993771755461,
-7.53645819908875));
#69089=CARTESIAN_POINT('Ctrl Pts',(0.782217059277867,0.050234956998986,
-7.52057160059434));
#69090=CARTESIAN_POINT('Ctrl Pts',(0.625721069366487,0.545859707382523,
-7.49938946926849));
#69091=CARTESIAN_POINT('Ctrl Pts',(0.132858431507887,0.819866970767157,
-7.47820733794263));
#69092=CARTESIAN_POINT('Ctrl Pts',(-0.36955528675953,0.690348117705594,
-7.45702520661678));
#69093=CARTESIAN_POINT('Ctrl Pts',(-0.754294552512423,0.346048338995004,
-7.4358430752909));
#69094=CARTESIAN_POINT('Ctrl Pts',(-0.815144306078038,-0.36014512431548,
-7.4093654111336));
#69095=CARTESIAN_POINT('Ctrl Pts',(-0.136086086799767,-0.880036698628102,
-7.3775922141448));
#69096=CARTESIAN_POINT('Ctrl Pts',(0.528922488702051,-0.6395115849869,-7.35111454998748));
#69097=CARTESIAN_POINT('Ctrl Pts',(0.763513227295881,-0.177298282695796,
-7.32993241866162));
#69098=CARTESIAN_POINT('Ctrl Pts',(0.75693428106787,0.209933609356769,-7.31404582016723));
#69099=CARTESIAN_POINT('Ctrl Pts',(0.563678937842369,0.544658731466687,
-7.29815922167283));
#69100=CARTESIAN_POINT('Ctrl Pts',(0.123555248510802,0.821111306314991,
-7.27697709034699));
#69101=CARTESIAN_POINT('Ctrl Pts',(-0.429479393638669,0.710901303288584,
-7.25579495902111));
#69102=CARTESIAN_POINT('Ctrl Pts',(-0.728570172364044,0.286944485106448,
-7.23461282769527));
#69103=CARTESIAN_POINT('Ctrl Pts',(-0.798931611445651,-0.22453954017939,
-7.2134306963694));
#69104=CARTESIAN_POINT('Ctrl Pts',(-0.388154685257379,-0.802184947884465,
-7.18695303221208));
#69105=CARTESIAN_POINT('Ctrl Pts',(0.465970323534831,-0.758851547759888,
-7.15517983522329));
#69106=CARTESIAN_POINT('Ctrl Pts',(0.817129237482638,-0.145030602419892,
-7.12870217106598));
#69107=CARTESIAN_POINT('Ctrl Pts',(0.696717242889235,0.359127014806003,
-7.1075200397401));
#69108=CARTESIAN_POINT('Ctrl Pts',(0.441027326936127,0.650012709944097,
-7.09163344124572));
#69109=CARTESIAN_POINT('Ctrl Pts',(0.0770447603055038,0.780032809335269,
-7.07574684275133));
#69110=CARTESIAN_POINT('Ctrl Pts',(-0.437375717913696,0.70582728636144,
-7.05456471142546));
#69111=CARTESIAN_POINT('Ctrl Pts',(-0.78754893079125,0.263817918624197,
-7.03338258009962));
#69112=CARTESIAN_POINT('Ctrl Pts',(-0.741063702120943,-0.252935215006503,
-7.01220044877374));
#69113=CARTESIAN_POINT('Ctrl Pts',(-0.46358212175395,-0.688332289858035,
-6.99101831744789));
#69114=CARTESIAN_POINT('Ctrl Pts',(0.223448433227565,-0.862690876263233,
-6.96454065329057));
#69115=CARTESIAN_POINT('Ctrl Pts',(0.846402689376789,-0.276742662718453,
-6.93276745630178));
#69116=CARTESIAN_POINT('Ctrl Pts',(0.716694312453694,0.418429598479429,
-6.90628979214446));
#69117=CARTESIAN_POINT('Ctrl Pts',(0.298549740945737,0.724744907870361,
-6.88510766081859));
#69118=CARTESIAN_POINT('Ctrl Pts',(-0.0846403243704471,0.780933826699518,
-6.86922106232421));
#69119=CARTESIAN_POINT('Ctrl Pts',(-0.446233320337088,0.644408955982971,
-6.85333446382981));
#69120=CARTESIAN_POINT('Ctrl Pts',(-0.790282759485384,0.254838844868011,
-6.83215233250395));
#69121=CARTESIAN_POINT('Ctrl Pts',(-0.771045731306174,-0.308742113761099,
-6.8109702011781));
#69122=CARTESIAN_POINT('Ctrl Pts',(-0.401093723806668,-0.672514281125272,
-6.78978806985224));
#69123=CARTESIAN_POINT('Ctrl Pts',(0.0922555398017252,-0.824741559667119,
-6.76860593852637));
#69124=CARTESIAN_POINT('Ctrl Pts',(0.728775372717111,-0.512885178590886,
-6.74212827436905));
#69125=CARTESIAN_POINT('Ctrl Pts',(0.82427039002562,0.336990115741366,-6.71035507738027));
#69126=CARTESIAN_POINT('Ctrl Pts',(0.275386408658267,0.782876996896595,
-6.68387741322294));
#69127=CARTESIAN_POINT('Ctrl Pts',(-0.241613501318641,0.745660811168969,
-6.66269528189708));
#69128=CARTESIAN_POINT('Ctrl Pts',(-0.57005148285138,0.540428471763071,
-6.6468086834027));
#69129=CARTESIAN_POINT('Ctrl Pts',(-0.75727463761217,0.202292367226153,
-6.63092208490829));
#69130=CARTESIAN_POINT('Ctrl Pts',(-0.767316805534387,-0.317355632215704,
-6.60973995358245));
#69131=CARTESIAN_POINT('Ctrl Pts',(-0.387819019492267,-0.734458725566816,
-6.58855782225657));
#69132=CARTESIAN_POINT('Ctrl Pts',(0.129643795992169,-0.772233203466112,
-6.56737569093074));
#69133=CARTESIAN_POINT('Ctrl Pts',(0.60421477347276,-0.568888594012783,
-6.54619355960485));
#69134=CARTESIAN_POINT('Ctrl Pts',(0.887483356468985,0.0808581273468804,
-6.51971589544755));
#69135=CARTESIAN_POINT('Ctrl Pts',(0.410099958547019,0.79044421082833,-6.48794269845874));
#69136=CARTESIAN_POINT('Ctrl Pts',(-0.296900337661013,0.774973707316207,
-6.46146503430144));
#69137=CARTESIAN_POINT('Ctrl Pts',(-0.666860912852976,0.411926749263547,
-6.44028290297557));
#69138=CARTESIAN_POINT('Ctrl Pts',(-0.784335711330281,0.0428853824613141,
-6.42439630448119));
#69139=CARTESIAN_POINT('Ctrl Pts',(-0.708142180514372,-0.336038136658672,
-6.40850970598678));
#69140=CARTESIAN_POINT('Ctrl Pts',(-0.379400994004317,-0.73861005639688,
-6.38732757466094));
#69141=CARTESIAN_POINT('Ctrl Pts',(0.179861749568897,-0.810853057436283,
-6.36614544333507));
#69142=CARTESIAN_POINT('Ctrl Pts',(0.598720101579247,-0.504664087636979,
-6.34496331200921));
#69143=CARTESIAN_POINT('Ctrl Pts',(0.828798932842316,-0.0424611625032776,
-6.32378118068336));
#69144=CARTESIAN_POINT('Ctrl Pts',(0.624086742236349,0.636142542035344,
-6.29730351652602));
#69145=CARTESIAN_POINT('Ctrl Pts',(-0.199119407007607,0.867950779039128,
-6.26553031953726));
#69146=CARTESIAN_POINT('Ctrl Pts',(-0.72797945196655,0.39847486417064,-6.23905265537991));
#69147=CARTESIAN_POINT('Ctrl Pts',(-0.774932010702059,-0.117721945292821,
-6.21787052405407));
#69148=CARTESIAN_POINT('Ctrl Pts',(-0.625586409139169,-0.4750663333995,
-6.20198392555967));
#69149=CARTESIAN_POINT('Ctrl Pts',(-0.322183903833611,-0.714521199467751,
-6.18609732706528));
#69150=CARTESIAN_POINT('Ctrl Pts',(0.18891837154225,-0.808617098475062,
-6.16491519573941));
#69151=CARTESIAN_POINT('Ctrl Pts',(0.662086178303616,-0.501496584144044,
-6.14373306441357));
#69152=CARTESIAN_POINT('Ctrl Pts',(0.782929853410714,0.00282242379590618,
-6.12255093308769));
#69153=CARTESIAN_POINT('Ctrl Pts',(0.65943455555827,0.504418815941523,-6.10136880176185));
#69154=CARTESIAN_POINT('Ctrl Pts',(0.0633494618177429,0.888321484655266,
-6.07489113760451));
#69155=CARTESIAN_POINT('Ctrl Pts',(-0.712753999556802,0.533586528221487,
-6.04311794061574));
#69156=CARTESIAN_POINT('Ctrl Pts',(-0.834426729678636,-0.309565746092443,
-6.01134474362693));
#69157=CARTESIAN_POINT('Ctrl Pts',(-0.192051279620842,-0.869031198721859,
-5.97957154663817));
#69158=CARTESIAN_POINT('Ctrl Pts',(0.626405930208662,-0.632730951971766,
-5.94779834964936));
#69159=CARTESIAN_POINT('Ctrl Pts',(0.871207376069929,0.18473202833857,-5.91602515266059));
#69160=CARTESIAN_POINT('Ctrl Pts',(0.409088109036795,0.722453592962815,
-5.88954748850325));
#69161=CARTESIAN_POINT('Ctrl Pts',(-0.104714804097165,0.775900722541678,
-5.86836535717741));
#69162=CARTESIAN_POINT('Ctrl Pts',(-0.587662362179258,0.586949639651242,
-5.84718322585153));
#69163=CARTESIAN_POINT('Ctrl Pts',(-0.826898986241856,0.076090929844471,
-5.82600109452569));
#69164=CARTESIAN_POINT('Ctrl Pts',(-0.663510831709495,-0.417248593266023,
-5.80481896319982));
#69165=CARTESIAN_POINT('Ctrl Pts',(-0.38466164816873,-0.684895461262083,
-5.78893236470544));
#69166=CARTESIAN_POINT('Ctrl Pts',(-0.0101945223770054,-0.783756434951424,
-5.77304576621103));
#69167=CARTESIAN_POINT('Ctrl Pts',(0.494664911251325,-0.666365459367492,
-5.75186363488519));
#69168=CARTESIAN_POINT('Ctrl Pts',(0.887071385837545,-0.078047738660052,
-5.72538597072785));
#69169=CARTESIAN_POINT('Ctrl Pts',(0.544417912065992,0.705528690163676,
-5.69361277373907));
#69170=CARTESIAN_POINT('Ctrl Pts',(-0.155868076444456,0.815117024817418,
-5.66713510958174));
#69171=CARTESIAN_POINT('Ctrl Pts',(-0.582098546485917,0.523748874523383,
-5.64595297825589));
#69172=CARTESIAN_POINT('Ctrl Pts',(-0.827870125232059,0.0668130635430879,
-5.62477084693002));
#69173=CARTESIAN_POINT('Ctrl Pts',(-0.679514548851711,-0.477231503110312,
-5.60358871560419));
#69174=CARTESIAN_POINT('Ctrl Pts',(-0.235614059614225,-0.747578084232534,
-5.58240658427831));
#69175=CARTESIAN_POINT('Ctrl Pts',(0.150182669760855,-0.771016750661316,
-5.56651998578392));
#69176=CARTESIAN_POINT('Ctrl Pts',(0.499596680867893,-0.60397870849536,
-5.55063338728952));
#69177=CARTESIAN_POINT('Ctrl Pts',(0.808402184679265,-0.187669830661293,
-5.52945125596367));
#69178=CARTESIAN_POINT('Ctrl Pts',(0.726642152424438,0.514757427097727,
-5.50297359180634));
#69179=CARTESIAN_POINT('Ctrl Pts',(-0.0417754286247196,0.890179509049,-5.47120039481756));
#69180=CARTESIAN_POINT('Ctrl Pts',(-0.646469171849264,0.52037230396045,
-5.44472273066023));
#69181=CARTESIAN_POINT('Ctrl Pts',(-0.782720280203898,0.022374032545029,
-5.42354059933438));
#69182=CARTESIAN_POINT('Ctrl Pts',(-0.674246595796987,-0.484999731440488,
-5.40235846800852));
#69183=CARTESIAN_POINT('Ctrl Pts',(-0.208982783747563,-0.803626700310318,
-5.38117633668266));
#69184=CARTESIAN_POINT('Ctrl Pts',(0.304363613856124,-0.722322552028555,
-5.35999420535681));
#69185=CARTESIAN_POINT('Ctrl Pts',(0.613587412181548,-0.490440734243774,
-5.3441076068624));
#69186=CARTESIAN_POINT('Ctrl Pts',(0.771775082904571,-0.136931920092647,
-5.32822100836802));
#69187=CARTESIAN_POINT('Ctrl Pts',(0.737645240287663,0.380280903838839,
-5.30703887704216));
#69188=CARTESIAN_POINT('Ctrl Pts',(0.220610507918605,0.862736934283135,
-5.28056121288483));
#69189=CARTESIAN_POINT('Ctrl Pts',(-0.608100710201375,0.651443225883695,
-5.24878801589605));
#69190=CARTESIAN_POINT('Ctrl Pts',(-0.829597137570893,-0.0218703955254784,
-5.22231035173872));
#69191=CARTESIAN_POINT('Ctrl Pts',(-0.611066093544301,-0.489642586909114,
-5.20112822041286));
#69192=CARTESIAN_POINT('Ctrl Pts',(-0.199938811978368,-0.80613750938647,
-5.17994608908701));
#69193=CARTESIAN_POINT('Ctrl Pts',(0.360944933020524,-0.74780240178827,
-5.15876395776115));
#69194=CARTESIAN_POINT('Ctrl Pts',(0.699580405510616,-0.353517092876322,
-5.13758182643528));
#69195=CARTESIAN_POINT('Ctrl Pts',(0.785158688205617,0.0233978744402808,
-5.12169522794091));
#69196=CARTESIAN_POINT('Ctrl Pts',(0.676883090725284,0.395242217877812,
-5.10580862944649));
#69197=CARTESIAN_POINT('Ctrl Pts',(0.316050663373499,0.767363046131555,
-5.08462649812065));
#69198=CARTESIAN_POINT('Ctrl Pts',(-0.390347541635626,0.800382915042411,
-5.05814883396331));
#69199=CARTESIAN_POINT('Ctrl Pts',(-0.885202127408502,0.102868576013952,
-5.02637563697454));
#69200=CARTESIAN_POINT('Ctrl Pts',(-0.618153465990248,-0.553711131688124,
-4.9998979728172));
#69201=CARTESIAN_POINT('Ctrl Pts',(-0.148777649674118,-0.768776199260246,
-4.97871584149136));
#69202=CARTESIAN_POINT('Ctrl Pts',(0.369463543596736,-0.743861480741264,
-4.95753371016549));
#69203=CARTESIAN_POINT('Ctrl Pts',(0.759200609827415,-0.336309546148421,
-4.93635157883964));
#69204=CARTESIAN_POINT('Ctrl Pts',(0.762063906997977,0.183427588930845,
-4.91516944751377));
#69205=CARTESIAN_POINT('Ctrl Pts',(0.58329407081499,0.526108024216862,-4.89928284901939));
#69206=CARTESIAN_POINT('Ctrl Pts',(0.260053068103058,0.739431897521899,
-4.88339625052499));
#69207=CARTESIAN_POINT('Ctrl Pts',(-0.255863414058302,0.789473229269786,
-4.86221411919913));
#69208=CARTESIAN_POINT('Ctrl Pts',(-0.815649130744606,0.357352080542846,
-4.83573645504181));
#69209=CARTESIAN_POINT('Ctrl Pts',(-0.741285154047814,-0.494632258034153,
-4.80396325805302));
#69210=CARTESIAN_POINT('Ctrl Pts',(-0.112704652167952,-0.822196683434577,
-4.7774855938957));
#69211=CARTESIAN_POINT('Ctrl Pts',(0.384272177024485,-0.682265730897016,
-4.75630346256984));
#69212=CARTESIAN_POINT('Ctrl Pts',(0.763142251788303,-0.327791269122783,
-4.73512133124398));
#69213=CARTESIAN_POINT('Ctrl Pts',(0.796366532129932,0.23513830673929,-4.71393919991812));
#69214=CARTESIAN_POINT('Ctrl Pts',(0.462095817256364,0.633130740372142,
-4.69275706859227));
#69215=CARTESIAN_POINT('Ctrl Pts',(0.104004079803942,0.778591534488675,
-4.67687047009787));
#69216=CARTESIAN_POINT('Ctrl Pts',(-0.280462970183203,0.731934185332714,
-4.66098387160347));
#69217=CARTESIAN_POINT('Ctrl Pts',(-0.706084152242396,0.436095444070873,
-4.63980174027762));
#69218=CARTESIAN_POINT('Ctrl Pts',(-0.853013011994254,-0.255641967057878,
-4.61332407612029));
#69219=CARTESIAN_POINT('Ctrl Pts',(-0.244799346010742,-0.856876905099193,
-4.58155087913152));
#69220=CARTESIAN_POINT('Ctrl Pts',(0.446348564306262,-0.69963039100146,
-4.55507321497417));
#69221=CARTESIAN_POINT('Ctrl Pts',(0.734555098285578,-0.271257149535717,
-4.53389108364833));
#69222=CARTESIAN_POINT('Ctrl Pts',(0.793856488162095,0.24418249073304,-4.51270895232246));
#69223=CARTESIAN_POINT('Ctrl Pts',(0.454765904643669,0.694750062084561,
-4.49152682099662));
#69224=CARTESIAN_POINT('Ctrl Pts',(-0.0576535306276524,0.781705282786401,
-4.47034468967075));
#69225=CARTESIAN_POINT('Ctrl Pts',(-0.42475216183662,0.660762610328711,
-4.45445809117636));
#69226=CARTESIAN_POINT('Ctrl Pts',(-0.687585668501137,0.376315130940137,
-4.43857149268196));
#69227=CARTESIAN_POINT('Ctrl Pts',(-0.820478298756319,-0.124697344226614,
-4.41738936135611));
#69228=CARTESIAN_POINT('Ctrl Pts',(-0.484668237188422,-0.74704799967164,
-4.39091169719878));
#69229=CARTESIAN_POINT('Ctrl Pts',(0.368117527293529,-0.811575157578735,
-4.35913850020999));
#69230=CARTESIAN_POINT('Ctrl Pts',(0.793110205375747,-0.244307034282585,
-4.33266083605267));
#69231=CARTESIAN_POINT('Ctrl Pts',(0.735470123003793,0.268766314407819,
-4.31147870472682));
#69232=CARTESIAN_POINT('Ctrl Pts',(0.446997997760977,0.700018573021691,
-4.29029657340095));
#69233=CARTESIAN_POINT('Ctrl Pts',(-0.103129739915628,0.823925927215433,
-4.2691144420751));
#69234=CARTESIAN_POINT('Ctrl Pts',(-0.549981800405103,0.558486434887335,
-4.24793231074924));
#69235=CARTESIAN_POINT('Ctrl Pts',(-0.751488473754749,0.228662852267375,
-4.23204571225485));
#69236=CARTESIAN_POINT('Ctrl Pts',(-0.76767999378356,-0.158286311622709,
-4.21615911376045));
#69237=CARTESIAN_POINT('Ctrl Pts',(-0.544637896405776,-0.626181785255629,
-4.19497698243459));
#69238=CARTESIAN_POINT('Ctrl Pts',(0.114193653274018,-0.883144282382366,
-4.16849931827727));
#69239=CARTESIAN_POINT('Ctrl Pts',(0.805950943289732,-0.380273358664594,
-4.13672612128849));
#69240=CARTESIAN_POINT('Ctrl Pts',(0.762654065470712,0.327213235203154,
-4.11024845713116));
#69241=CARTESIAN_POINT('Ctrl Pts',(0.386582048616603,0.680959582705881,
-4.0890663258053));
#69242=CARTESIAN_POINT('Ctrl Pts',(-0.112460950524283,0.822912964525908,
-4.06788419447944));
#69243=CARTESIAN_POINT('Ctrl Pts',(-0.611974985955589,0.561227488063028,
-4.04670206315359));
#69244=CARTESIAN_POINT('Ctrl Pts',(-0.780728624225886,0.0696411806645941,
-4.02551993182773));
#69245=CARTESIAN_POINT('Ctrl Pts',(-0.720803064736381,-0.312193158252911,
-4.00963333333333));
#69246=CARTESIAN_POINT('Ctrl Pts',(-0.482651613809183,-0.61760387708469,
-3.99374673483894));
#69247=CARTESIAN_POINT('Ctrl Pts',(-0.00975770699374649,-0.829842667944631,
-3.97256460351309));
#69248=CARTESIAN_POINT('Ctrl Pts',(0.658742944809585,-0.599200923410776,
-3.94608693935576));
#69249=CARTESIAN_POINT('Ctrl Pts',(0.860459287509756,0.231893434227583,
-3.91431374236698));
#69250=CARTESIAN_POINT('Ctrl Pts',(0.369465644127221,0.743104880000642,
-3.88783607820964));
#69251=CARTESIAN_POINT('Ctrl Pts',(-0.146171548563407,0.769275966075993,
-3.8666539468838));
#69252=CARTESIAN_POINT('Ctrl Pts',(-0.618431405135488,0.554414835407384,
-3.84547181555793));
#69253=CARTESIAN_POINT('Ctrl Pts',(-0.829753688343227,0.0315989473508514,
-3.82428968423208));
#69254=CARTESIAN_POINT('Ctrl Pts',(-0.640146574483296,-0.452326698203083,
-3.80310755290621));
#69255=CARTESIAN_POINT('Ctrl Pts',(-0.347290478918943,-0.704564368560852,
-3.78722095441182));
#69256=CARTESIAN_POINT('Ctrl Pts',(0.0319347387027416,-0.7831776948858,
-3.77133435591742));
#69257=CARTESIAN_POINT('Ctrl Pts',(0.529763427087315,-0.638815135784943,
-3.75015222459158));
#69258=CARTESIAN_POINT('Ctrl Pts',(0.88998199246047,-0.0302665995583043,
-3.72367456043424));
#69259=CARTESIAN_POINT('Ctrl Pts',(0.505717390271106,0.733767450543454,
-3.69190136344546));
#69260=CARTESIAN_POINT('Ctrl Pts',(-0.199447423651738,0.805562195035123,
-3.66542369928813));
#69261=CARTESIAN_POINT('Ctrl Pts',(-0.609403272469123,0.491710570453291,
-3.64424156796228));
#69262=CARTESIAN_POINT('Ctrl Pts',(-0.830264524545408,0.0222268274621526,
-3.62305943663642));
#69263=CARTESIAN_POINT('Ctrl Pts',(-0.652886296214935,-0.513058633108947,
-3.60187730531056));
#69264=CARTESIAN_POINT('Ctrl Pts',(-0.19509905614842,-0.759159691382518,
-3.58069517398471));
#69265=CARTESIAN_POINT('Ctrl Pts',(0.191399837462849,-0.761831824231885,
-3.5648085754903));
#69266=CARTESIAN_POINT('Ctrl Pts',(0.5313323429325,-0.576257816134853,-3.54892197699592));
#69267=CARTESIAN_POINT('Ctrl Pts',(0.817319344918664,-0.143955391732878,
-3.52773984567005));
#69268=CARTESIAN_POINT('Ctrl Pts',(0.697929257925564,0.553063074959991,
-3.50126218151273));
#69269=CARTESIAN_POINT('Ctrl Pts',(-0.0895529864465379,0.886648190049562,
-3.46948898452395));
#69270=CARTESIAN_POINT('Ctrl Pts',(-0.673499633430044,0.484879334103558,
-3.44301132036662));
#69271=CARTESIAN_POINT('Ctrl Pts',(-0.782791606892125,-0.0197214038754891,
-3.42182918904077));
#69272=CARTESIAN_POINT('Ctrl Pts',(-0.647208586358955,-0.520532667870995,
-3.4006470577149));
#69273=CARTESIAN_POINT('Ctrl Pts',(-0.165494189844444,-0.813696104157199,
-3.37946492638905));
#69274=CARTESIAN_POINT('Ctrl Pts',(0.342741156734687,-0.704922391622064,
-3.35828279506319));
#69275=CARTESIAN_POINT('Ctrl Pts',(0.639056875647929,-0.45675807150001,
-3.3423961965688));
#69276=CARTESIAN_POINT('Ctrl Pts',(0.778018525719848,-0.0952591357265069,
-3.3265095980744));
#69277=CARTESIAN_POINT('Ctrl Pts',(0.716143170352185,0.419372180700096,
-3.30532746674855));
#69278=CARTESIAN_POINT('Ctrl Pts',(0.173928549241014,0.873345792748581,
-3.27884980259121));
#69279=CARTESIAN_POINT('Ctrl Pts',(-0.642230317963104,0.617822765029477,
-3.24707660560244));
#69280=CARTESIAN_POINT('Ctrl Pts',(-0.827223047175183,-0.0664210440547759,
-3.22059894144511));
#69281=CARTESIAN_POINT('Ctrl Pts',(-0.583869875304254,-0.521773516292051,
-3.19941681011925));
#69282=CARTESIAN_POINT('Ctrl Pts',(-0.15632835702201,-0.815717265581917,
-3.17823467879339));
#69283=CARTESIAN_POINT('Ctrl Pts',(0.400609992898513,-0.727324762662962,
-3.15705254746754));
#69284=CARTESIAN_POINT('Ctrl Pts',(0.717567380243094,-0.315411054880874,
-3.13587041614168));
#69285=CARTESIAN_POINT('Ctrl Pts',(0.782766726021657,0.0655582094525445,
-3.11998381764728));
#69286=CARTESIAN_POINT('Ctrl Pts',(0.6546648075705,0.431046539287036,-3.10409721915289));
#69287=CARTESIAN_POINT('Ctrl Pts',(0.274356150345474,0.783238641254918,
-3.08291508782703));
#69288=CARTESIAN_POINT('Ctrl Pts',(-0.432795772061448,0.778249210496526,
-3.05643742366971));
#69289=CARTESIAN_POINT('Ctrl Pts',(-0.889451114215646,0.055149485221593,
-3.02466422668093));
#69290=CARTESIAN_POINT('Ctrl Pts',(-0.58750398582496,-0.586130353684993,
-2.99818656252359));
#69291=CARTESIAN_POINT('Ctrl Pts',(-0.107248906905033,-0.775660560786259,
-2.97700443119775));
#69292=CARTESIAN_POINT('Ctrl Pts',(0.408904510245349,-0.722931749253457,
-2.95582229987188));
#69293=CARTESIAN_POINT('Ctrl Pts',(0.776176704892586,-0.295024405049747,
-2.93464016854603));
#69294=CARTESIAN_POINT('Ctrl Pts',(0.751105377928227,0.224115572812998,
-2.91345803722016));
#69295=CARTESIAN_POINT('Ctrl Pts',(0.554178344183514,0.556693801861776,
-2.89757143872578));
#69296=CARTESIAN_POINT('Ctrl Pts',(0.219940482511759,0.752338563051997,
-2.88168484023137));
#69297=CARTESIAN_POINT('Ctrl Pts',(-0.297919693948934,0.774582418045106,
-2.86050270890553));
#69298=CARTESIAN_POINT('Ctrl Pts',(-0.833674474879105,0.313003009390929,
-2.83402504474819));
#69299=CARTESIAN_POINT('Ctrl Pts',(-0.71363262372644,-0.533753902705133,
-2.80225184775942));
#69300=CARTESIAN_POINT('Ctrl Pts',(-0.0683572379509413,-0.827065301467073,
-2.77577418360209));
#69301=CARTESIAN_POINT('Ctrl Pts',(0.420381611491688,-0.660629195775685,
-2.75459205227623));
#69302=CARTESIAN_POINT('Ctrl Pts',(0.779654881965752,-0.286306614671439,
-2.73340992095037));
#69303=CARTESIAN_POINT('Ctrl Pts',(0.78257951976473,0.27759497840861,-2.71222778962451));
#69304=CARTESIAN_POINT('Ctrl Pts',(0.427403862088424,0.657048717677694,
-2.69104565829866));
#69305=CARTESIAN_POINT('Ctrl Pts',(0.0620125630885026,0.783055597140136,
-2.67515905980426));
#69306=CARTESIAN_POINT('Ctrl Pts',(-0.319391575743669,0.71580454779683,
-2.65927246130987));
#69307=CARTESIAN_POINT('Ctrl Pts',(-0.728499459819008,0.397520569820789,
-2.63809032998401));
#69308=CARTESIAN_POINT('Ctrl Pts',(-0.838042285090092,-0.301113172002998,
-2.61161266582668));
#69309=CARTESIAN_POINT('Ctrl Pts',(-0.198397349884215,-0.868794130884054,
-2.5798394688379));
#69310=CARTESIAN_POINT('Ctrl Pts',(0.483301467830881,-0.674632800909974,
-2.55336180468057));
#69311=CARTESIAN_POINT('Ctrl Pts',(0.748070914185315,-0.231390451275595,
-2.53217967335472));
#69312=CARTESIAN_POINT('Ctrl Pts',(0.779587071663486,0.286491204529554,
-2.51099754202886));
#69313=CARTESIAN_POINT('Ctrl Pts',(0.416773141159263,0.718185091463975,
-2.48981541070299));
#69314=CARTESIAN_POINT('Ctrl Pts',(-0.0995787808181823,0.777477424200066,
-2.46863327937715));
#69315=CARTESIAN_POINT('Ctrl Pts',(-0.45964753201515,0.636981767796903,
-2.45274668088275));
#69316=CARTESIAN_POINT('Ctrl Pts',(-0.706815134212639,0.338820742208353,
-2.43686008238836));
#69317=CARTESIAN_POINT('Ctrl Pts',(-0.812591502026715,-0.168609362792247,
-2.4156779510625));
#69318=CARTESIAN_POINT('Ctrl Pts',(-0.443821791933158,-0.772014398154575,
-2.38920028690517));
#69319=CARTESIAN_POINT('Ctrl Pts',(0.411199347587806,-0.790619913006889,
-2.35742708991639));
#69320=CARTESIAN_POINT('Ctrl Pts',(0.805093118566376,-0.201332549053002,
-2.33094942575906));
#69321=CARTESIAN_POINT('Ctrl Pts',(0.719963950045008,0.307901841870368,
-2.3097672944332));
#69322=CARTESIAN_POINT('Ctrl Pts',(0.408733331163781,0.723028544784651,
-2.28858516310735));
#69323=CARTESIAN_POINT('Ctrl Pts',(-0.147258198381348,0.817193183893717,
-2.26740303178149));
#69324=CARTESIAN_POINT('Ctrl Pts',(-0.579199926573699,0.528123587607129,
-2.24622090045563));
#69325=CARTESIAN_POINT('Ctrl Pts',(-0.762690818405532,0.187947710050428,
-2.23033430196123));
#69326=CARTESIAN_POINT('Ctrl Pts',(-0.758064432560231,-0.199312431598691,
-2.21444770346684));
#69327=CARTESIAN_POINT('Ctrl Pts',(-0.510200100753733,-0.654545585561551,
-2.19326557214098));
#69328=CARTESIAN_POINT('Ctrl Pts',(0.161488497277849,-0.875731396719148,
-2.16678790798366));
#69329=CARTESIAN_POINT('Ctrl Pts',(0.825222082722822,-0.336412342945777,
-2.13501471099487));
#69330=CARTESIAN_POINT('Ctrl Pts',(0.743967694720049,0.367725161070136,
-2.10853704683755));
#69331=CARTESIAN_POINT('Ctrl Pts',(0.349428907465107,0.700750363695459,
-2.08735491551169));
#69332=CARTESIAN_POINT('Ctrl Pts',(-0.156521488967608,0.815680229053644,
-2.06617278418584));
#69333=CARTESIAN_POINT('Ctrl Pts',(-0.641250834035424,0.52752918842634,
-2.04499065285997));
#69334=CARTESIAN_POINT('Ctrl Pts',(-0.783342948908494,0.0275844725406853,
-2.02380852153412));
#69335=CARTESIAN_POINT('Ctrl Pts',(-0.702984342986585,-0.350477730689136,
-2.00792192303972));
#69336=CARTESIAN_POINT('Ctrl Pts',(-0.448764363180785,-0.642648952104954,
-1.99203532454533));
#69337=CARTESIAN_POINT('Ctrl Pts',(0.0348518394390736,-0.82916790559871,
-1.97085319321947));
#69338=CARTESIAN_POINT('Ctrl Pts',(0.689991891074865,-0.562934458177559,
-1.94437552906215));
#69339=CARTESIAN_POINT('Ctrl Pts',(0.846754038208352,0.277799116408794,
-1.91260233207336));
#69340=CARTESIAN_POINT('Ctrl Pts',(0.328997570582567,0.761886030467734,
-1.88612466791604));
#69341=CARTESIAN_POINT('Ctrl Pts',(-0.187300941572847,0.76030914165062,
-1.86494253659018));
#69342=CARTESIAN_POINT('Ctrl Pts',(-0.647331814067898,0.520379414536371,
-1.84376040526432));
#69343=CARTESIAN_POINT('Ctrl Pts',(-0.830252794971939,-0.0130373783466202,
-1.82257827393846));
#69344=CARTESIAN_POINT('Ctrl Pts',(-0.614913676842763,-0.486074324318531,
-1.80139614261261));
#69345=CARTESIAN_POINT('Ctrl Pts',(-0.308925602114689,-0.722209525381228,
-1.78550954411821));
#69346=CARTESIAN_POINT('Ctrl Pts',(0.073976279919845,-0.780329827260158,
-1.76962294562382));
#69347=CARTESIAN_POINT('Ctrl Pts',(0.563327604660279,-0.609422740152469,
-1.74844081429796));
#69348=CARTESIAN_POINT('Ctrl Pts',(0.890322468184475,0.0176044482627306,
-1.72196315014064));
#69349=CARTESIAN_POINT('Ctrl Pts',(0.465554220531463,0.759884213577963,
-1.69018995315185));
#69350=CARTESIAN_POINT('Ctrl Pts',(-0.242449840923054,0.793679909981037,
-1.66371228899453));
#69351=CARTESIAN_POINT('Ctrl Pts',(-0.63494702258507,0.45825092700608,-1.64253015766867));
#69352=CARTESIAN_POINT('Ctrl Pts',(-0.83025923865599,-0.0224234075023661,
-1.62134802634281));
#69353=CARTESIAN_POINT('Ctrl Pts',(-0.624371277112666,-0.547403128516433,
-1.60016589501695));
#69354=CARTESIAN_POINT('Ctrl Pts',(-0.154020165762932,-0.768547244656021,
-1.57898376369109));
#69355=CARTESIAN_POINT('Ctrl Pts',(0.232063829254024,-0.750445204758646,
-1.5630971651967));
#69356=CARTESIAN_POINT('Ctrl Pts',(0.561532445545602,-0.546871504013718,
-1.54721056670231));
#69357=CARTESIAN_POINT('Ctrl Pts',(0.823874414294551,-0.0998249260357819,
-1.52602843537644));
#69358=CARTESIAN_POINT('Ctrl Pts',(0.667199326600337,0.589770355762977,
-1.49955077121913));
#69359=CARTESIAN_POINT('Ctrl Pts',(-0.137071735407018,0.880554421743578,
-1.46777757423034));
#69360=CARTESIAN_POINT('Ctrl Pts',(-0.698583654935227,0.447985046545584,
-1.44129991007301));
#69361=CARTESIAN_POINT('Ctrl Pts',(-0.780600637389563,-0.0617598453575331,
-1.42011777874716));
#69362=CARTESIAN_POINT('Ctrl Pts',(-0.618300119713807,-0.554561245075368,
-1.3989356474213));
#69363=CARTESIAN_POINT('Ctrl Pts',(-0.121527311840313,-0.821413896443042,
-1.37775351609544));
#69364=CARTESIAN_POINT('Ctrl Pts',(0.38012816508924,-0.685484979292683,
-1.35657138476958));
#69365=CARTESIAN_POINT('Ctrl Pts',(0.662679441042163,-0.421755361096154,
-1.34068478627519));
#69366=CARTESIAN_POINT('Ctrl Pts',(0.78201346623163,-0.053311048902077,
-1.32479818778079));
#69367=CARTESIAN_POINT('Ctrl Pts',(0.692571420136857,0.457251456418509,
-1.30361605645493));
#69368=CARTESIAN_POINT('Ctrl Pts',(0.126743930630883,0.881430649569758,
-1.27713839229761));
#69369=CARTESIAN_POINT('Ctrl Pts',(-0.674503856347413,0.582416773515433,
-1.24536519530882));
#69370=CARTESIAN_POINT('Ctrl Pts',(-0.82245825156047,-0.110779733305397,
-1.2188875311515));
#69371=CARTESIAN_POINT('Ctrl Pts',(-0.554986251520806,-0.552396500907149,
-1.19770539982564));
#69372=CARTESIAN_POINT('Ctrl Pts',(-0.112266107328216,-0.822939568694453,
-1.17652326849979));
#69373=CARTESIAN_POINT('Ctrl Pts',(0.439117275072637,-0.704745128060961,
-1.15534113717392));
#69374=CARTESIAN_POINT('Ctrl Pts',(0.733480558694665,-0.276393467265362,
-1.13415900584807));
#69375=CARTESIAN_POINT('Ctrl Pts',(0.778112539034564,0.107529078813453,
-1.11827240735367));
#69376=CARTESIAN_POINT('Ctrl Pts',(0.630554518897266,0.465605120247713,
-1.10238580885928));
#69377=CARTESIAN_POINT('Ctrl Pts',(0.231868737890888,0.796850647722728,
-1.08120367753342));
#69378=CARTESIAN_POINT('Ctrl Pts',(-0.473993206691168,0.753866336934694,
-1.0547260133761));
#69379=CARTESIAN_POINT('Ctrl Pts',(-0.891129554390263,0.00727101037626396,
-1.02295281638731));
#69380=CARTESIAN_POINT('Ctrl Pts',(-0.555156597401148,-0.616855637271071,
-0.996475152229989));
#69381=CARTESIAN_POINT('Ctrl Pts',(-0.0654102108264915,-0.78030323458971,
-0.97529302090413));
#69382=CARTESIAN_POINT('Ctrl Pts',(0.447163727728668,-0.699912718259666,
-0.954110889578273));
#69383=CARTESIAN_POINT('Ctrl Pts',(0.790909620559512,-0.252886632503504,
-0.932928758252414));
#69384=CARTESIAN_POINT('Ctrl Pts',(0.737976126523209,0.264155854396524,
-0.911746626926556));
#69385=CARTESIAN_POINT('Ctrl Pts',(0.523461021630659,0.585670713820323,
-0.895860028432162));
#69386=CARTESIAN_POINT('Ctrl Pts',(0.179192260788228,0.763070942295198,
-0.879973429937767));
#69387=CARTESIAN_POINT('Ctrl Pts',(-0.339114974901541,0.757453034972048,
-0.858791298611909));
#69388=CARTESIAN_POINT('Ctrl Pts',(-0.849290468929591,0.267749347956247,
-0.832313634454588));
#69389=CARTESIAN_POINT('Ctrl Pts',(-0.683917668721205,-0.571332978840512,
-0.800540437465799));
#69390=CARTESIAN_POINT('Ctrl Pts',(-0.0238122687778703,-0.829543670184782,
-0.774062773308478));
#69391=CARTESIAN_POINT('Ctrl Pts',(0.455276127534381,-0.637083417819315,
-0.752880641982621));
#69392=CARTESIAN_POINT('Ctrl Pts',(0.793914280715303,-0.243994523545205,
-0.731698510656761));
#69393=CARTESIAN_POINT('Ctrl Pts',(0.766530823567235,0.319249390391231,
-0.710516379330903));
#69394=CARTESIAN_POINT('Ctrl Pts',(0.391476694020716,0.67906779978643,-0.689334248005045));
#69395=CARTESIAN_POINT('Ctrl Pts',(0.0198418276109007,0.785256600327428,
-0.673447649510651));
#69396=CARTESIAN_POINT('Ctrl Pts',(-0.357397127539648,0.697606208289608,
-0.657561051016257));
#69397=CARTESIAN_POINT('Ctrl Pts',(-0.748809377631163,0.357796847151619,
-0.6363789196904));
#69398=CARTESIAN_POINT('Ctrl Pts',(-0.820649583666188,-0.345714150263954,
-0.609901255533077));
#69399=CARTESIAN_POINT('Ctrl Pts',(-0.151421980355895,-0.87820050681865,
-0.578128058544288));
#69400=CARTESIAN_POINT('Ctrl Pts',(0.518857616055017,-0.647685501528246,
-0.551650394386966));
#69401=CARTESIAN_POINT('Ctrl Pts',(0.759424772369192,-0.190855020100471,
-0.530468263061107));
#69402=CARTESIAN_POINT('Ctrl Pts',(0.76306463279521,0.327971932825795,-0.509286131735249));
#69403=CARTESIAN_POINT('Ctrl Pts',(0.377575861208738,0.739544570500736,
-0.488104000409392));
#69404=CARTESIAN_POINT('Ctrl Pts',(-0.141216211695821,0.771002588600507,
-0.466921869083532));
#69405=CARTESIAN_POINT('Ctrl Pts',(-0.493214572385959,0.611360104474943,
-0.451035270589139));
#69406=CARTESIAN_POINT('Ctrl Pts',(-0.724001752965214,0.300347002913539,
-0.435148672094745));
#69407=CARTESIAN_POINT('Ctrl Pts',(-0.802356556010187,-0.212033778434851,
-0.413966540768886));
#69408=CARTESIAN_POINT('Ctrl Pts',(-0.401692126280537,-0.794750299379084,
-0.387488876611564));
#69409=CARTESIAN_POINT('Ctrl Pts',(0.453091810094164,-0.767378607107432,
-0.355715679622776));
#69410=CARTESIAN_POINT('Ctrl Pts',(0.814750920558571,-0.157778118181504,
-0.329238015465453));
#69411=CARTESIAN_POINT('Ctrl Pts',(0.702374874168397,0.346150068442172,
-0.308055884139595));
#69412=CARTESIAN_POINT('Ctrl Pts',(0.369293024947228,0.743942379054456,
-0.286873752813738));
#69413=CARTESIAN_POINT('Ctrl Pts',(-0.190972491990077,0.80811205708209,
-0.265691621487879));
#69414=CARTESIAN_POINT('Ctrl Pts',(-0.606730035741863,0.496217965426545,
-0.24450949016202));
#69415=CARTESIAN_POINT('Ctrl Pts',(-0.771718314924831,0.146723681079384,
-0.228622891667627));
#69416=CARTESIAN_POINT('Ctrl Pts',(-0.746204491110825,-0.239825074069584,
-0.212736293173232));
#69417=CARTESIAN_POINT('Ctrl Pts',(-0.474403504239302,-0.68088258957028,
-0.191554161847375));
#69418=CARTESIAN_POINT('Ctrl Pts',(0.208556009763689,-0.866067206476802,
-0.165076497690051));
#69419=CARTESIAN_POINT('Ctrl Pts',(0.841689935707378,-0.29109045562369,
-0.133303300701264));
#69420=CARTESIAN_POINT('Ctrl Pts',(0.723834370006008,0.406353263108837,
-0.106825636543941));
#69421=CARTESIAN_POINT('Ctrl Pts',(0.310318878599919,0.719620732838044,
-0.0856435052180828));
#69422=CARTESIAN_POINT('Ctrl Pts',(-0.0705387118779829,0.782181820540678,
-0.0697569067236875));
#69423=CARTESIAN_POINT('Ctrl Pts',(-0.437154537896543,0.651981105845494,
-0.0538703082292969));
#69424=CARTESIAN_POINT('Ctrl Pts',(-0.609248872823355,0.459854686869421,
-0.0432792425663656));
#69425=CARTESIAN_POINT('Ctrl Pts',(-0.667283755215006,0.348842645238897,
-0.0379837097349007));
#69426=CARTESIAN_POINT('Ctrl Pts',(0.415028236876425,-0.582012248187004,
-11.9309162902651));
#69427=CARTESIAN_POINT('Ctrl Pts',(0.511854163508475,-0.51296646136859,
-11.9256207574336));
#69428=CARTESIAN_POINT('Ctrl Pts',(0.670087794403581,-0.326089049241816,
-11.9150296917707));
#69429=CARTESIAN_POINT('Ctrl Pts',(0.744730245171791,0.0356362322782299,
-11.8991430932763));
#69430=CARTESIAN_POINT('Ctrl Pts',(0.636250090767451,0.385624774244037,
-11.8832564947819));
#69431=CARTESIAN_POINT('Ctrl Pts',(0.287757616503084,0.733640547045757,
-11.8620743634561));
#69432=CARTESIAN_POINT('Ctrl Pts',(-0.383456490043703,0.75354609726296,
-11.8355966992987));
#69433=CARTESIAN_POINT('Ctrl Pts',(-0.84160538740142,0.0832144579414285,
-11.80382350231));
#69434=CARTESIAN_POINT('Ctrl Pts',(-0.578431492064404,-0.534873771688162,
-11.7773458381526));
#69435=CARTESIAN_POINT('Ctrl Pts',(-0.128244477331174,-0.732967324015595,
-11.7561637068268));
#69436=CARTESIAN_POINT('Ctrl Pts',(0.238577604025672,-0.706567602715354,
-11.7402771083324));
#69437=CARTESIAN_POINT('Ctrl Pts',(0.545720466397418,-0.505857385659933,
-11.724390509838));
#69438=CARTESIAN_POINT('Ctrl Pts',(0.784814276644656,-0.0742348289681934,
-11.7032083785121));
#69439=CARTESIAN_POINT('Ctrl Pts',(0.651433163568701,0.44425251973168,-11.6820262471863));
#69440=CARTESIAN_POINT('Ctrl Pts',(0.233942323917106,0.705612521504789,
-11.6608441158604));
#69441=CARTESIAN_POINT('Ctrl Pts',(-0.25458267785024,0.745592758200979,
-11.6396619845345));
#69442=CARTESIAN_POINT('Ctrl Pts',(-0.780680935113796,0.326032206682622,
-11.6131843203772));
#69443=CARTESIAN_POINT('Ctrl Pts',(-0.69498736268188,-0.481342937675468,
-11.5814111233884));
#69444=CARTESIAN_POINT('Ctrl Pts',(-0.0947903846137628,-0.782147648046809,
-11.5549334592311));
#69445=CARTESIAN_POINT('Ctrl Pts',(0.37681872151215,-0.641669810040819,
-11.5337513279052));
#69446=CARTESIAN_POINT('Ctrl Pts',(0.639197522483424,-0.384101318856191,
-11.5178647294109));
#69447=CARTESIAN_POINT('Ctrl Pts',(0.743431501282844,-0.0322836142324497,
-11.5019781309165));
#69448=CARTESIAN_POINT('Ctrl Pts',(0.646217846697502,0.451468074312828,
-11.4807959995906));
#69449=CARTESIAN_POINT('Ctrl Pts',(0.208936536557157,0.760313131267001,
-11.4596138682647));
#69450=CARTESIAN_POINT('Ctrl Pts',(-0.27847443281849,0.68925408536552,-11.4384317369389));
#69451=CARTESIAN_POINT('Ctrl Pts',(-0.676699493032713,0.403479561635729,
-11.417249605613));
#69452=CARTESIAN_POINT('Ctrl Pts',(-0.806086988029912,-0.25687713306994,
-11.3907719414558));
#69453=CARTESIAN_POINT('Ctrl Pts',(-0.218113661252782,-0.81677680986074,
-11.3589987444669));
#69454=CARTESIAN_POINT('Ctrl Pts',(0.43407642426811,-0.657508592639888,
-11.3325210803096));
#69455=CARTESIAN_POINT('Ctrl Pts',(0.702594455791664,-0.245140299377268,
-11.3113389489837));
#69456=CARTESIAN_POINT('Ctrl Pts',(0.735839301880873,0.121027553653736,
-11.2954523504894));
#69457=CARTESIAN_POINT('Ctrl Pts',(0.58753558633177,0.456655915830853,-11.279565751995));
#69458=CARTESIAN_POINT('Ctrl Pts',(0.200282317827862,0.762435503674711,
-11.2583836206691));
#69459=CARTESIAN_POINT('Ctrl Pts',(-0.332941019414456,0.714759261957186,
-11.2372014893433));
#69460=CARTESIAN_POINT('Ctrl Pts',(-0.658440964812338,0.345072034184339,
-11.2160193580174));
#69461=CARTESIAN_POINT('Ctrl Pts',(-0.776967605321815,-0.130534639197338,
-11.1948372266915));
#69462=CARTESIAN_POINT('Ctrl Pts',(-0.448102068257463,-0.717611756999146,
-11.1683595625342));
#69463=CARTESIAN_POINT('Ctrl Pts',(0.362498219216689,-0.763736190311011,
-11.1365863655454));
#69464=CARTESIAN_POINT('Ctrl Pts',(0.756488843802834,-0.2201465861157,-11.1101087013881));
#69465=CARTESIAN_POINT('Ctrl Pts',(0.694203209002715,0.267982538451035,
-11.0889265700622));
#69466=CARTESIAN_POINT('Ctrl Pts',(0.482502477870242,0.568593444849717,
-11.0730399715678));
#69467=CARTESIAN_POINT('Ctrl Pts',(0.152196914730789,0.728401530662744,
-11.0571533730735));
#69468=CARTESIAN_POINT('Ctrl Pts',(-0.340911127398258,0.710774582661878,
-11.0359712417476));
#69469=CARTESIAN_POINT('Ctrl Pts',(-0.716465727379952,0.329252769757259,
-11.0147891104217));
#69470=CARTESIAN_POINT('Ctrl Pts',(-0.7252408739192,-0.163232618497991,
-10.9936069790959));
#69471=CARTESIAN_POINT('Ctrl Pts',(-0.507695658401522,-0.602464165054588,
-10.97242484777));
#69472=CARTESIAN_POINT('Ctrl Pts',(0.123008428398455,-0.837037050495868,
-10.9459471836127));
#69473=CARTESIAN_POINT('Ctrl Pts',(0.770699286912404,-0.347448609847742,
-10.9141739866239));
#69474=CARTESIAN_POINT('Ctrl Pts',(0.719101275335622,0.321921179769178,
-10.8876963224665));
#69475=CARTESIAN_POINT('Ctrl Pts',(0.355636165011655,0.653647959104139,
-10.8665141911407));
#69476=CARTESIAN_POINT('Ctrl Pts',(-0.000321386690041276,0.745725850019615,
-10.8506275926463));
#69477=CARTESIAN_POINT('Ctrl Pts',(-0.35552940505769,0.653705998798072,
-10.8347409941519));
#69478=CARTESIAN_POINT('Ctrl Pts',(-0.719960978738509,0.321056215071895,
-10.8135588628261));
#69479=CARTESIAN_POINT('Ctrl Pts',(-0.759226175895796,-0.212852387201534,
-10.7923767315002));
#69480=CARTESIAN_POINT('Ctrl Pts',(-0.447102902654478,-0.593900839688561,
-10.7711946001744));
#69481=CARTESIAN_POINT('Ctrl Pts',(0.00304566864510004,-0.787850668361192,
-10.7500124688485));
#69482=CARTESIAN_POINT('Ctrl Pts',(0.635613857181148,-0.558352148665305,
-10.7235348046912));
#69483=CARTESIAN_POINT('Ctrl Pts',(0.812341618079216,0.23409191115644,-10.6917616077024));
#69484=CARTESIAN_POINT('Ctrl Pts',(0.339695932367431,0.710877319729864,
-10.6652839435451));
#69485=CARTESIAN_POINT('Ctrl Pts',(-0.152077971138047,0.728426404655775,
-10.6441018122192));
#69486=CARTESIAN_POINT('Ctrl Pts',(-0.482992393837075,0.568177343945017,
-10.6282152137248));
#69487=CARTESIAN_POINT('Ctrl Pts',(-0.69415940968358,0.268095887087071,
-10.6123286152304));
#69488=CARTESIAN_POINT('Ctrl Pts',(-0.75658416484695,-0.22136238534414,
-10.5911464839045));
#69489=CARTESIAN_POINT('Ctrl Pts',(-0.440884710216198,-0.653721039282296,
-10.5699643525787));
#69490=CARTESIAN_POINT('Ctrl Pts',(0.043685421188573,-0.742098913164826,
-10.5487822212529));
#69491=CARTESIAN_POINT('Ctrl Pts',(0.512338419743362,-0.598520923100893,
-10.527600089927));
#69492=CARTESIAN_POINT('Ctrl Pts',(0.845909660974294,-0.014104709504769,
-10.5011224257697));
#69493=CARTESIAN_POINT('Ctrl Pts',(0.467619355160476,0.704294019576864,
-10.4693492287809));
#69494=CARTESIAN_POINT('Ctrl Pts',(-0.20127503533384,0.761727149525769,
-10.4428715646235));
#69495=CARTESIAN_POINT('Ctrl Pts',(-0.587461030951866,0.45675187292246,
-10.4216894332977));
#69496=CARTESIAN_POINT('Ctrl Pts',(-0.735943347206106,0.120393257203035,
-10.4058028348033));
#69497=CARTESIAN_POINT('Ctrl Pts',(-0.702634449225675,-0.245025552721734,
-10.3899162363089));
#69498=CARTESIAN_POINT('Ctrl Pts',(-0.433362025741317,-0.658496969459834,
-10.368734104983));
#69499=CARTESIAN_POINT('Ctrl Pts',(0.0871496215066032,-0.783667957986035,
-10.3475519736572));
#69500=CARTESIAN_POINT('Ctrl Pts',(0.513696156330839,-0.537341113182083,
-10.3263698423313));
#69501=CARTESIAN_POINT('Ctrl Pts',(0.777953608135155,-0.12452363359687,
-10.3051877110055));
#69502=CARTESIAN_POINT('Ctrl Pts',(0.653875292926478,0.536851188561754,
-10.2787100468481));
#69503=CARTESIAN_POINT('Ctrl Pts',(-0.0995112619803705,0.839520956302764,
-10.2469368498594));
#69504=CARTESIAN_POINT('Ctrl Pts',(-0.646515899350175,0.450285556131582,
-10.220459185702));
#69505=CARTESIAN_POINT('Ctrl Pts',(-0.743436834368463,-0.0321622388741894,
-10.1992770543762));
#69506=CARTESIAN_POINT('Ctrl Pts',(-0.638866127347263,-0.384652073964505,
-10.1833904558818));
#69507=CARTESIAN_POINT('Ctrl Pts',(-0.376923639214111,-0.641608339196779,
-10.1675038573874));
#69508=CARTESIAN_POINT('Ctrl Pts',(0.0959750524998173,-0.782438300085102,
-10.1463217260615));
#69509=CARTESIAN_POINT('Ctrl Pts',(0.573733992537099,-0.540888002002435,
-10.1251395947357));
#69510=CARTESIAN_POINT('Ctrl Pts',(0.739383564307667,-0.0770140102612942,
-10.1039574634098));
#69511=CARTESIAN_POINT('Ctrl Pts',(0.673559771585897,0.408699383209504,
-10.082775332084));
#69512=CARTESIAN_POINT('Ctrl Pts',(0.150845825635244,0.832470800838251,
-10.0562976679266));
#69513=CARTESIAN_POINT('Ctrl Pts',(-0.619312495169557,0.575456306472777,
-10.0245244709379));
#69514=CARTESIAN_POINT('Ctrl Pts',(-0.784261926880214,-0.0753201182913833,
-9.99804680678051));
#69515=CARTESIAN_POINT('Ctrl Pts',(-0.545820424427594,-0.505779399128595,
-9.97686467545469));
#69516=CARTESIAN_POINT('Ctrl Pts',(-0.237932443072409,-0.706749813732185,
-9.96097807696027));
#69517=CARTESIAN_POINT('Ctrl Pts',(0.128058976679507,-0.733030414933145,
-9.94509147846588));
#69518=CARTESIAN_POINT('Ctrl Pts',(0.579664632968886,-0.534237603906211,
-9.92390934714004));
#69519=CARTESIAN_POINT('Ctrl Pts',(0.787439938769152,-0.0408517776110334,
-9.90272721581415));
#69520=CARTESIAN_POINT('Ctrl Pts',(0.613406568615596,0.419942370479663,
-9.88154508448832));
#69521=CARTESIAN_POINT('Ctrl Pts',(0.248808536191952,0.74753746665481,-9.86036295316244));
#69522=CARTESIAN_POINT('Ctrl Pts',(-0.423928686959554,0.732152009990144,
-9.83388528900514));
#69523=CARTESIAN_POINT('Ctrl Pts',(-0.844557330553996,0.0376940677022658,
-9.80211209201634));
#69524=CARTESIAN_POINT('Ctrl Pts',(-0.548998577207228,-0.565102161027307,
-9.775634427859));
#69525=CARTESIAN_POINT('Ctrl Pts',(-0.0886017953782055,-0.738838587352449,
-9.75445229653318));
#69526=CARTESIAN_POINT('Ctrl Pts',(0.276166281305673,-0.692704360998744,
-9.73856569803876));
#69527=CARTESIAN_POINT('Ctrl Pts',(0.57213439116594,-0.475809761533366,
-9.72267909954437));
#69528=CARTESIAN_POINT('Ctrl Pts',(0.787655067120261,-0.0319436908039809,
-9.70149696821853));
#69529=CARTESIAN_POINT('Ctrl Pts',(0.626624986972285,0.478614302549277,
-9.68031483689264));
#69530=CARTESIAN_POINT('Ctrl Pts',(0.195682142263798,0.717166446610471,
-9.65913270556681));
#69531=CARTESIAN_POINT('Ctrl Pts',(-0.294280608957396,0.73083300070969,
-9.63795057424093));
#69532=CARTESIAN_POINT('Ctrl Pts',(-0.797074929608463,0.283608275530733,
-9.61147291008363));
#69533=CARTESIAN_POINT('Ctrl Pts',(-0.668115187284044,-0.5179961620059,
-9.57969971309482));
#69534=CARTESIAN_POINT('Ctrl Pts',(-0.0526214205896454,-0.78611123657433,
-9.5532220489375));
#69535=CARTESIAN_POINT('Ctrl Pts',(0.410757474929328,-0.62049257295707,
-9.53203991761165));
#69536=CARTESIAN_POINT('Ctrl Pts',(0.658915249864171,-0.349195991061354,
-9.51615331911726));
#69537=CARTESIAN_POINT('Ctrl Pts',(0.744092180646416,0.00771475379514762,
-9.50026672062285));
#69538=CARTESIAN_POINT('Ctrl Pts',(0.621022284247614,0.485543228364149,
-9.47908458929701));
#69539=CARTESIAN_POINT('Ctrl Pts',(0.167775681958537,0.770442629561796,
-9.45790245797112));
#69540=CARTESIAN_POINT('Ctrl Pts',(-0.315112305102429,0.67329298831777,
-9.4367203266453));
#69541=CARTESIAN_POINT('Ctrl Pts',(-0.697404491344613,0.366530936193706,
-9.4155381953194));
#69542=CARTESIAN_POINT('Ctrl Pts',(-0.791117695616473,-0.299824763891077,
-9.38906053116213));
#69543=CARTESIAN_POINT('Ctrl Pts',(-0.173905189465712,-0.827317902870068,
-9.35728733417329));
#69544=CARTESIAN_POINT('Ctrl Pts',(0.468783450174122,-0.633231369260984,
-9.33080967001601));
#69545=CARTESIAN_POINT('Ctrl Pts',(0.714752945652261,-0.207028894086353,
-9.30962753869013));
#69546=CARTESIAN_POINT('Ctrl Pts',(0.728272023089266,0.160396406014447,
-9.29374094019575));
#69547=CARTESIAN_POINT('Ctrl Pts',(0.562146062042697,0.487569990519461,
-9.27785434170134));
#69548=CARTESIAN_POINT('Ctrl Pts',(0.159019896480474,0.772096870001262,
-9.2566722103755));
#69549=CARTESIAN_POINT('Ctrl Pts',(-0.370870818981993,0.695834290999209,
-9.23549007904961));
#69550=CARTESIAN_POINT('Ctrl Pts',(-0.676033552397828,0.309189018202799,
-9.21430794772379));
#69551=CARTESIAN_POINT('Ctrl Pts',(-0.768829988206647,-0.172099973761879,
-9.1931258163979));
#69552=CARTESIAN_POINT('Ctrl Pts',(-0.40889035488849,-0.740655638633112,
-9.1666481522406));
#69553=CARTESIAN_POINT('Ctrl Pts',(0.403017310632342,-0.743152053528152,
-9.1348749552518));
#69554=CARTESIAN_POINT('Ctrl Pts',(0.767226301746,-0.179175031972786,-9.10839729109448));
#69555=CARTESIAN_POINT('Ctrl Pts',(0.678798787336911,0.304901529374881,
-9.08721515976862));
#69556=CARTESIAN_POINT('Ctrl Pts',(0.451249245738007,0.593701326339906,
-9.07132856127423));
#69557=CARTESIAN_POINT('Ctrl Pts',(0.112832951222732,0.735527984405508,
-9.05544196277983));
#69558=CARTESIAN_POINT('Ctrl Pts',(-0.378615274819878,0.691427058926299,
-9.03425983145398));
#69559=CARTESIAN_POINT('Ctrl Pts',(-0.733124346516869,0.290274383036051,
-9.01307770012811));
#69560=CARTESIAN_POINT('Ctrl Pts',(-0.715420825257699,-0.201970927938732,
-8.99189556880227));
#69561=CARTESIAN_POINT('Ctrl Pts',(-0.474585821341943,-0.628876975183433,
-8.97071343747639));
#69562=CARTESIAN_POINT('Ctrl Pts',(0.167812748838726,-0.829217087792485,
-8.94423577331909));
#69563=CARTESIAN_POINT('Ctrl Pts',(0.788257375451387,-0.305529437827074,
-8.91246257633028));
#69564=CARTESIAN_POINT('Ctrl Pts',(0.700762232327224,0.360100241484309,
-8.88598491217298));
#69565=CARTESIAN_POINT('Ctrl Pts',(0.319995458059088,0.671815185245732,
-8.8648027808471));
#69566=CARTESIAN_POINT('Ctrl Pts',(-0.040395961119228,0.744630991164172,
-8.84891618235272));
#69567=CARTESIAN_POINT('Ctrl Pts',(-0.390145583636105,0.633655359240732,
-8.83302958385832));
#69568=CARTESIAN_POINT('Ctrl Pts',(-0.736174067273288,0.281901838973623,
-8.81184745253247));
#69569=CARTESIAN_POINT('Ctrl Pts',(-0.746690469329113,-0.253345353057471,
-8.7906653212066));
#69570=CARTESIAN_POINT('Ctrl Pts',(-0.414540813271791,-0.617069791090766,
-8.76948318988076));
#69571=CARTESIAN_POINT('Ctrl Pts',(0.0453800790159918,-0.786548536431907,
-8.74830105855488));
#69572=CARTESIAN_POINT('Ctrl Pts',(0.664701026950137,-0.523387659513758,
-8.72182339439757));
#69573=CARTESIAN_POINT('Ctrl Pts',(0.798587754341329,0.277408590257236,
-8.69005019740877));
#69574=CARTESIAN_POINT('Ctrl Pts',(0.301002774099267,0.728105226020141,
-8.66357253325146));
#69575=CARTESIAN_POINT('Ctrl Pts',(-0.191003588526136,0.719201199578629,
-8.6423904019256));
#69576=CARTESIAN_POINT('Ctrl Pts',(-0.512828106903175,0.541400479725488,
-8.62650380343121));
#69577=CARTESIAN_POINT('Ctrl Pts',(-0.707563712994288,0.230404606679193,
-8.61061720493682));
#69578=CARTESIAN_POINT('Ctrl Pts',(-0.743594951797162,-0.261701073372229,
-8.58943507361094));
#69579=CARTESIAN_POINT('Ctrl Pts',(-0.405116890236114,-0.676469385965225,
-8.5682529422851));
#69580=CARTESIAN_POINT('Ctrl Pts',(0.0835024235041277,-0.738678927690356,
-8.54707081095923));
#69581=CARTESIAN_POINT('Ctrl Pts',(0.543762380284107,-0.570123166975729,
-8.52588867963338));
#69582=CARTESIAN_POINT('Ctrl Pts',(0.845445287876903,0.0313745528509859,
-8.49941101547605));
#69583=CARTESIAN_POINT('Ctrl Pts',(0.429095129360905,0.728405997566729,
-8.46763781848728));
#69584=CARTESIAN_POINT('Ctrl Pts',(-0.24191913210034,0.749809991729314,
-8.44116015432992));
#69585=CARTESIAN_POINT('Ctrl Pts',(-0.611157820186959,0.42452191360344,
-8.4199780230041));
#69586=CARTESIAN_POINT('Ctrl Pts',(-0.74134978577321,0.080669956061101,
-8.40409142450968));
#69587=CARTESIAN_POINT('Ctrl Pts',(-0.688451544413171,-0.282430808730881,
-8.38820482601531));
#69588=CARTESIAN_POINT('Ctrl Pts',(-0.3973484194103,-0.68083414847857,-8.36702269468943));
#69589=CARTESIAN_POINT('Ctrl Pts',(0.129137722759079,-0.777852153987728,
-8.34584056336358));
#69590=CARTESIAN_POINT('Ctrl Pts',(0.541830373946935,-0.508958798738525,
-8.32465843203773));
#69591=CARTESIAN_POINT('Ctrl Pts',(0.783521306039094,-0.0825367476792268,
-8.30347630071186));
#69592=CARTESIAN_POINT('Ctrl Pts',(0.624080241337119,0.571214451613806,
-8.27699863655454));
#69593=CARTESIAN_POINT('Ctrl Pts',(-0.144483020465117,0.832960133577659,
-8.24522543956576));
#69594=CARTESIAN_POINT('Ctrl Pts',(-0.66977985567032,0.414891353382473,
-8.21874777540842));
#69595=CARTESIAN_POINT('Ctrl Pts',(-0.740634167244186,-0.0720677918054417,
-8.19756564408258));
#69596=CARTESIAN_POINT('Ctrl Pts',(-0.617271889931151,-0.418428680395727,
-8.18167904558817));
#69597=CARTESIAN_POINT('Ctrl Pts',(-0.341899176308968,-0.66093694401547,
-8.1657924470938));
#69598=CARTESIAN_POINT('Ctrl Pts',(0.137884319468111,-0.776149997479365,
-8.14461031576791));
#69599=CARTESIAN_POINT('Ctrl Pts',(0.601972062897985,-0.509274150525132,
-8.12342818444209));
#69600=CARTESIAN_POINT('Ctrl Pts',(0.742453846576301,-0.0371685169046532,
-8.1022460531162));
#69601=CARTESIAN_POINT('Ctrl Pts',(0.650623107466303,0.444305664791217,
-8.08106392179036));
#69602=CARTESIAN_POINT('Ctrl Pts',(0.105891169344639,0.839374265518477,
-8.05458625763302));
#69603=CARTESIAN_POINT('Ctrl Pts',(-0.649342391994081,0.541343130825394,
-8.02281306064425));
#69604=CARTESIAN_POINT('Ctrl Pts',(-0.779080977831934,-0.117357233069515,
-7.99633539648691));
#69605=CARTESIAN_POINT('Ctrl Pts',(-0.517851300905695,-0.534380731740471,
-7.97515326516107));
#69606=CARTESIAN_POINT('Ctrl Pts',(-0.199608145616148,-0.718514951048735,
-7.95926666666666));
#69607=CARTESIAN_POINT('Ctrl Pts',(0.167266719814572,-0.725089329095204,
-7.94338006817229));
#69608=CARTESIAN_POINT('Ctrl Pts',(0.607536743444001,-0.502314651894469,
-7.92219793684639));
#69609=CARTESIAN_POINT('Ctrl Pts',(0.788497433317525,0.00152399292137779,
-7.90101580552058));
#69610=CARTESIAN_POINT('Ctrl Pts',(0.589952632896988,0.452299794254596,
-7.87983367419468));
#69611=CARTESIAN_POINT('Ctrl Pts',(0.208276608788832,0.759828142388853,
-7.85865154286886));
#69612=CARTESIAN_POINT('Ctrl Pts',(-0.462661687723661,0.708312261698578,
-7.8321738787115));
#69613=CARTESIAN_POINT('Ctrl Pts',(-0.845362595220247,-0.00774660796236431,
-7.80040068172274));
#69614=CARTESIAN_POINT('Ctrl Pts',(-0.517836877317961,-0.59378856393743,
-7.7739230175654));
#69615=CARTESIAN_POINT('Ctrl Pts',(-0.0487688443231488,-0.742532380525313,
-7.75274088623955));
#69616=CARTESIAN_POINT('Ctrl Pts',(0.312992899017785,-0.676862313798992,
-7.73685428774516));
#69617=CARTESIAN_POINT('Ctrl Pts',(0.596877491755274,-0.444375911319675,
-7.72096768925076));
#69618=CARTESIAN_POINT('Ctrl Pts',(0.788233533424651,0.0104307682983569,
-7.69978555792491));
#69619=CARTESIAN_POINT('Ctrl Pts',(0.599998941877613,0.511597297342836,
-7.67860342659904));
#69620=CARTESIAN_POINT('Ctrl Pts',(0.156859111171333,0.726646015737633,
-7.65742129527319));
#69621=CARTESIAN_POINT('Ctrl Pts',(-0.333130070508813,0.713962399470354,
-7.63623916394732));
#69622=CARTESIAN_POINT('Ctrl Pts',(-0.811164148261794,0.240363936426778,
-7.60976149979001));
#69623=CARTESIAN_POINT('Ctrl Pts',(-0.639312821126197,-0.553151917718901,
-7.57798830280121));
#69624=CARTESIAN_POINT('Ctrl Pts',(-0.010300046683182,-0.787803147500451,
-7.55151063864389));
#69625=CARTESIAN_POINT('Ctrl Pts',(0.443508970371773,-0.597521990812866,
-7.53032850731804));
#69626=CARTESIAN_POINT('Ctrl Pts',(0.676728772042507,-0.313281527969212,
-7.51444190882364));
#69627=CARTESIAN_POINT('Ctrl Pts',(0.742602365585634,0.0476908518678349,
-7.49855531032925));
#69628=CARTESIAN_POINT('Ctrl Pts',(0.594031977182028,0.518215123503371,
-7.47737317900339));
#69629=CARTESIAN_POINT('Ctrl Pts',(0.126129933316543,0.778345530483932,
-7.45619104767754));
#69630=CARTESIAN_POINT('Ctrl Pts',(-0.350839484906702,0.655386045606128,
-7.43500891635167));
#69631=CARTESIAN_POINT('Ctrl Pts',(-0.716093969570523,0.32852302579789,
-7.41382678502582));
#69632=CARTESIAN_POINT('Ctrl Pts',(-0.773862040986492,-0.341905891847567,
-7.3873491208685));
#69633=CARTESIAN_POINT('Ctrl Pts',(-0.129194126850317,-0.835468015497788,
-7.3555759238797));
#69634=CARTESIAN_POINT('Ctrl Pts',(0.502135675338213,-0.607124084290786,
-7.32909825972239));
#69635=CARTESIAN_POINT('Ctrl Pts',(0.724845772692903,-0.168319167400595,
-7.30791612839653));
#69636=CARTESIAN_POINT('Ctrl Pts',(0.718600011399384,0.199301706700394,
-7.29202952990213));
#69637=CARTESIAN_POINT('Ctrl Pts',(0.535131914738594,0.517074969954517,
-7.27614293140774));
#69638=CARTESIAN_POINT('Ctrl Pts',(0.117297901824557,0.779526847754431,
-7.25496080008188));
#69639=CARTESIAN_POINT('Ctrl Pts',(-0.407728788196936,0.674898333216349,
-7.23377866875603));
#69640=CARTESIAN_POINT('Ctrl Pts',(-0.691672377986925,0.27241243450832,
-7.21259653743016));
#69641=CARTESIAN_POINT('Ctrl Pts',(-0.758470423987435,-0.213167933026972,
-7.19141440610431));
#69642=CARTESIAN_POINT('Ctrl Pts',(-0.368496933257126,-0.761558998069061,
-7.16493674194697));
#69643=CARTESIAN_POINT('Ctrl Pts',(0.442371667103622,-0.720420179809253,
-7.1331635449582));
#69644=CARTESIAN_POINT('Ctrl Pts',(0.77574644728917,-0.137685655358597,
-7.10668588080086));
#69645=CARTESIAN_POINT('Ctrl Pts',(0.661432612057195,0.340939343597065,
-7.08550374947501));
#69646=CARTESIAN_POINT('Ctrl Pts',(0.418691886588421,0.617093389027879,
-7.06961715098062));
#69647=CARTESIAN_POINT('Ctrl Pts',(0.0731428963102508,0.740528735056654,
-7.05373055248622));
#69648=CARTESIAN_POINT('Ctrl Pts',(-0.415225210087146,0.670081285405351,
-7.03254842116036));
#69649=CARTESIAN_POINT('Ctrl Pts',(-0.747664209164554,0.250457092606872,
-7.01136628983452));
#69650=CARTESIAN_POINT('Ctrl Pts',(-0.70353318393837,-0.240125533924201,
-6.99018415850864));
#69651=CARTESIAN_POINT('Ctrl Pts',(-0.440104413697557,-0.653472307583564,
-6.9690020271828));
#69652=CARTESIAN_POINT('Ctrl Pts',(0.212132084225257,-0.819000657021791,
-6.94252436302547));
#69653=CARTESIAN_POINT('Ctrl Pts',(0.803537371007348,-0.262727274425518,
-6.91075116603669));
#69654=CARTESIAN_POINT('Ctrl Pts',(0.68039796053698,0.397238600176665,-6.88427350187936));
#69655=CARTESIAN_POINT('Ctrl Pts',(0.283429952391962,0.688040840642773,
-6.8630913705535));
#69656=CARTESIAN_POINT('Ctrl Pts',(-0.0803537897261284,0.741384121190458,
-6.8472047720591));
#69657=CARTESIAN_POINT('Ctrl Pts',(-0.42363422704096,0.611773432248228,
-6.83131817356472));
#69658=CARTESIAN_POINT('Ctrl Pts',(-0.750259585513473,0.241932756128878,
-6.81013604223885));
#69659=CARTESIAN_POINT('Ctrl Pts',(-0.731996799675116,-0.293106141467353,
-6.788953910913));
#69660=CARTESIAN_POINT('Ctrl Pts',(-0.380780685600718,-0.638455387964545,
-6.76777177958714));
#69661=CARTESIAN_POINT('Ctrl Pts',(0.0875833392822713,-0.782973250124461,
-6.74658964826127));
#69662=CARTESIAN_POINT('Ctrl Pts',(0.691867186148921,-0.48691056066591,
-6.72011198410396));
#69663=CARTESIAN_POINT('Ctrl Pts',(0.78252594245428,0.319923548278934,-6.68833878711517));
#69664=CARTESIAN_POINT('Ctrl Pts',(0.261439706657101,0.743228881245174,
-6.66186112295785));
#69665=CARTESIAN_POINT('Ctrl Pts',(-0.22937719844958,0.707897476449544,
-6.64067899163199));
#69666=CARTESIAN_POINT('Ctrl Pts',(-0.541181727820946,0.513058948026012,
-6.62479239313759));
#69667=CARTESIAN_POINT('Ctrl Pts',(-0.718923130886396,0.192047448544228,
-6.60890579464321));
#69668=CARTESIAN_POINT('Ctrl Pts',(-0.728456722063183,-0.301283435869895,
-6.58772366331733));
#69669=CARTESIAN_POINT('Ctrl Pts',(-0.368178266988903,-0.69726271060162,
-6.56654153199149));
#69670=CARTESIAN_POINT('Ctrl Pts',(0.123078100183777,-0.733124133353885,
-6.54535940066562));
#69671=CARTESIAN_POINT('Ctrl Pts',(0.573614848692852,-0.54007773246291,
-6.52417726933977));
#69672=CARTESIAN_POINT('Ctrl Pts',(0.842537543914182,0.0767631387380145,
-6.49769960518244));
#69673=CARTESIAN_POINT('Ctrl Pts',(0.389330807518773,0.750412860295417,
-6.46592640819366));
#69674=CARTESIAN_POINT('Ctrl Pts',(-0.281864081683107,0.735725846801378,
-6.43944874403633));
#69675=CARTESIAN_POINT('Ctrl Pts',(-0.633088329546757,0.391065082029191,
-6.41826661271048));
#69676=CARTESIAN_POINT('Ctrl Pts',(-0.744613720371767,0.0407134900563816,
-6.40238001421609));
#69677=CARTESIAN_POINT('Ctrl Pts',(-0.672278943783744,-0.319019781338021,
-6.38649341572168));
#69678=CARTESIAN_POINT('Ctrl Pts',(-0.360186564983986,-0.701203800939871,
-6.36531128439583));
#69679=CARTESIAN_POINT('Ctrl Pts',(0.170752809752722,-0.769788118850823,
-6.34412915306997));
#69680=CARTESIAN_POINT('Ctrl Pts',(0.568398449615586,-0.479105819619089,
-6.32294702174411));
#69681=CARTESIAN_POINT('Ctrl Pts',(0.786825141210475,-0.0403107543443066,
-6.30176489041825));
#69682=CARTESIAN_POINT('Ctrl Pts',(0.592480419109261,0.603925663550727,
-6.27528722626093));
#69683=CARTESIAN_POINT('Ctrl Pts',(-0.18903518009993,0.823994176656527,
-6.24351402927215));
#69684=CARTESIAN_POINT('Ctrl Pts',(-0.691111574103426,0.378294455803269,
-6.21703636511482));
#69685=CARTESIAN_POINT('Ctrl Pts',(-0.735686261875505,-0.111760021107787,
-6.19585423378896));
#69686=CARTESIAN_POINT('Ctrl Pts',(-0.593904136703258,-0.451007017563935,
-6.17996763529457));
#69687=CARTESIAN_POINT('Ctrl Pts',(-0.305867183926357,-0.678334902943274,
-6.16408103680018));
#69688=CARTESIAN_POINT('Ctrl Pts',(0.17935076708676,-0.767665398060909,
-6.14289890547431));
#69689=CARTESIAN_POINT('Ctrl Pts',(0.628555407221239,-0.476098731549411,
-6.12171677414847));
#69690=CARTESIAN_POINT('Ctrl Pts',(0.743279060887722,0.00267948462979709,
-6.1005346428226));
#69691=CARTESIAN_POINT('Ctrl Pts',(0.626038073573313,0.478872969492467,
-6.07935251149674));
#69692=CARTESIAN_POINT('Ctrl Pts',(0.0601411841463684,0.843333225837006,
-6.05287484733942));
#69693=CARTESIAN_POINT('Ctrl Pts',(-0.676657201314584,0.506563508686106,
-6.02110165035063));
#69694=CARTESIAN_POINT('Ctrl Pts',(-0.792167923235142,-0.293888061665043,
-5.98932845336184));
#69695=CARTESIAN_POINT('Ctrl Pts',(-0.18232501179644,-0.825019879436455,
-5.95755525637306));
#69696=CARTESIAN_POINT('Ctrl Pts',(0.594682153850289,-0.600686850459742,
-5.92578205938427));
#69697=CARTESIAN_POINT('Ctrl Pts',(0.827085846200354,0.1753764375457,-5.89400886239548));
#69698=CARTESIAN_POINT('Ctrl Pts',(0.38837020223537,0.685865567359653,-5.86753119823816));
#69699=CARTESIAN_POINT('Ctrl Pts',(-0.0994116151163395,0.736605914157616,
-5.84634906691231));
#69700=CARTESIAN_POINT('Ctrl Pts',(-0.557900719683635,0.557224092360063,
-5.82516693558644));
#69701=CARTESIAN_POINT('Ctrl Pts',(-0.785021415731397,0.0722373717524209,
-5.80398480426059));
#69702=CARTESIAN_POINT('Ctrl Pts',(-0.629907910310793,-0.396117405931614,
-5.78280267293472));
#69703=CARTESIAN_POINT('Ctrl Pts',(-0.36518079795383,-0.650209534143389,
-5.76691607444034));
#69704=CARTESIAN_POINT('Ctrl Pts',(-0.00967822977447486,-0.744063780934671,
-5.75102947594593));
#69705=CARTESIAN_POINT('Ctrl Pts',(0.469613042710347,-0.632617967866498,
-5.72984734462008));
#69706=CARTESIAN_POINT('Ctrl Pts',(0.842146437172344,-0.0740950797098429,
-5.70336968046277));
#69707=CARTESIAN_POINT('Ctrl Pts',(0.516846346640217,0.669797811348866,
-5.67159648347396));
#69708=CARTESIAN_POINT('Ctrl Pts',(-0.147974275060897,0.773836141361268,
-5.64511881931665));
#69709=CARTESIAN_POINT('Ctrl Pts',(-0.552618678533357,0.497224074290783,
-5.62393668799079));
#69710=CARTESIAN_POINT('Ctrl Pts',(-0.785943372243192,0.0634293748143924,
-5.60275455666493));
#69711=CARTESIAN_POINT('Ctrl Pts',(-0.645101133300516,-0.453062534162647,
-5.58157242533907));
#69712=CARTESIAN_POINT('Ctrl Pts',(-0.223681593183752,-0.709717650908249,
-5.56039029401322));
#69713=CARTESIAN_POINT('Ctrl Pts',(0.142576800788917,-0.731969286729474,
-5.54450369551882));
#69714=CARTESIAN_POINT('Ctrl Pts',(0.474295047200469,-0.573390739018259,
-5.52861709702442));
#69715=CARTESIAN_POINT('Ctrl Pts',(0.767461368384907,-0.178165457458594,
-5.50743496569857));
#69716=CARTESIAN_POINT('Ctrl Pts',(0.689842000918259,0.488687990796851,
-5.48095730154124));
#69717=CARTESIAN_POINT('Ctrl Pts',(-0.0396597488537021,0.84509715222258,
-5.44918410455246));
#69718=CARTESIAN_POINT('Ctrl Pts',(-0.613729310297357,0.494018507168641,
-5.42270644039513));
#69719=CARTESIAN_POINT('Ctrl Pts',(-0.743080101331292,0.0212409193823935,
-5.40152430906928));
#69720=CARTESIAN_POINT('Ctrl Pts',(-0.64009997108623,-0.460437347414257,
-5.38034217774342));
#69721=CARTESIAN_POINT('Ctrl Pts',(-0.19839903481638,-0.762927734213757,
-5.35916004641756));
#69722=CARTESIAN_POINT('Ctrl Pts',(0.288949386831816,-0.685741162878066,
-5.33797791509171));
#69723=CARTESIAN_POINT('Ctrl Pts',(0.582512818373229,-0.465602795425132,
-5.3220913165973));
#69724=CARTESIAN_POINT('Ctrl Pts',(0.732689213904483,-0.129997123661407,
-5.30620471810292));
#69725=CARTESIAN_POINT('Ctrl Pts',(0.70028784709236,0.361021912560238,-5.28502258677706));
#69726=CARTESIAN_POINT('Ctrl Pts',(0.209437883142914,0.819044382473843,
-5.25854492261973));
#69727=CARTESIAN_POINT('Ctrl Pts',(-0.577303985580056,0.618451457748302,
-5.22677172563096));
#69728=CARTESIAN_POINT('Ctrl Pts',(-0.787582921563938,-0.0207627886158348,
-5.20029406147361));
#69729=CARTESIAN_POINT('Ctrl Pts',(-0.580119189696666,-0.464845069558873,
-5.17911193014777));
#69730=CARTESIAN_POINT('Ctrl Pts',(-0.18981308702806,-0.765311385576726,
-5.1579297988219));
#69731=CARTESIAN_POINT('Ctrl Pts',(0.342665194945523,-0.709930608099066,
-5.13674766749606));
#69732=CARTESIAN_POINT('Ctrl Pts',(0.664150772330552,-0.335613531220212,
-5.11556553617018));
#69733=CARTESIAN_POINT('Ctrl Pts',(0.745395018308445,0.0222129097069853,
-5.0996789376758));
#69734=CARTESIAN_POINT('Ctrl Pts',(0.642602943052109,0.375225524033337,
-5.0837923391814));
#69735=CARTESIAN_POINT('Ctrl Pts',(0.300044556024852,0.728500620846027,
-5.06261020785554));
#69736=CARTESIAN_POINT('Ctrl Pts',(-0.370578734356334,0.759848227592405,
-5.03613254369823));
#69737=CARTESIAN_POINT('Ctrl Pts',(-0.840371845689285,0.0976588876276082,
-5.00435934670943));
#69738=CARTESIAN_POINT('Ctrl Pts',(-0.58684762841035,-0.525668919343541,
-4.97788168255212));
#69739=CARTESIAN_POINT('Ctrl Pts',(-0.141242936706458,-0.729842206079766,
-4.95669955122626));
#69740=CARTESIAN_POINT('Ctrl Pts',(0.350752387995542,-0.70618927152582,
-4.93551741990039));
#69741=CARTESIAN_POINT('Ctrl Pts',(0.720751563935925,-0.319277445533383,
-4.91433528857454));
#69742=CARTESIAN_POINT('Ctrl Pts',(0.723469851944388,0.174138060322337,
-4.89315315724868));
#69743=CARTESIAN_POINT('Ctrl Pts',(0.553753656586301,0.499463746926826,
-4.87726655875429));
#69744=CARTESIAN_POINT('Ctrl Pts',(0.246882909622859,0.701984020645308,
-4.86137996025989));
#69745=CARTESIAN_POINT('Ctrl Pts',(-0.242905436915294,0.749491053242322,
-4.84019782893404));
#69746=CARTESIAN_POINT('Ctrl Pts',(-0.774341299252633,0.339254299315688,
-4.81372016477671));
#69747=CARTESIAN_POINT('Ctrl Pts',(-0.703743420627555,-0.469582043186583,
-4.78194696778792));
#69748=CARTESIAN_POINT('Ctrl Pts',(-0.10699682437215,-0.780557256906211,
-4.75546930363059));
#69749=CARTESIAN_POINT('Ctrl Pts',(0.364811051232433,-0.647712984155424,
-4.73428717230475));
#69750=CARTESIAN_POINT('Ctrl Pts',(0.724493584913005,-0.311190569141564,
-4.71310504097887));
#69751=CARTESIAN_POINT('Ctrl Pts',(0.756035250853362,0.223229934393878,
-4.69192290965303));
#69752=CARTESIAN_POINT('Ctrl Pts',(0.438693381781545,0.601066391928822,
-4.67074077832716));
#69753=CARTESIAN_POINT('Ctrl Pts',(0.0987368848287337,0.739160452304642,
-4.65485417983278));
#69754=CARTESIAN_POINT('Ctrl Pts',(-0.266259170196915,0.694866023483125,
-4.63896758133838));
#69755=CARTESIAN_POINT('Ctrl Pts',(-0.670325142540075,0.414009774584999,
-4.61778545001252));
#69756=CARTESIAN_POINT('Ctrl Pts',(-0.809812919660765,-0.242695204903068,
-4.5913077858552));
#69757=CARTESIAN_POINT('Ctrl Pts',(-0.232401698844621,-0.813481129304173,
-4.55953458886641));
#69758=CARTESIAN_POINT('Ctrl Pts',(0.423743634580864,-0.66419822635029,
-4.53305692470909));
#69759=CARTESIAN_POINT('Ctrl Pts',(0.697354202608967,-0.257519570224186,
-4.51187479338323));
#69760=CARTESIAN_POINT('Ctrl Pts',(0.753652325850476,0.23181608365883,-4.49069266205737));
#69761=CARTESIAN_POINT('Ctrl Pts',(0.431734686134142,0.659565057390897,
-4.46951053073151));
#69762=CARTESIAN_POINT('Ctrl Pts',(-0.0547337183721843,0.742116507563613,
-4.44832839940566));
#69763=CARTESIAN_POINT('Ctrl Pts',(-0.403240962883958,0.627298870180159,
-4.43244180091126));
#69764=CARTESIAN_POINT('Ctrl Pts',(-0.652763498207381,0.357256982735486,
-4.41655520241687));
#69765=CARTESIAN_POINT('Ctrl Pts',(-0.778925898305787,-0.118382157109167,
-4.395373071091));
#69766=CARTESIAN_POINT('Ctrl Pts',(-0.460122641396538,-0.709214412012832,
-4.36889540693369));
#69767=CARTESIAN_POINT('Ctrl Pts',(0.349474539501924,-0.77047364886787,
-4.33712220994489));
#69768=CARTESIAN_POINT('Ctrl Pts',(0.75294383789821,-0.231934319810118,
-4.31064454578758));
#69769=CARTESIAN_POINT('Ctrl Pts',(0.698222886706653,0.255154881246402,
-4.28946241446172));
#69770=CARTESIAN_POINT('Ctrl Pts',(0.424360178050591,0.66456674923413,-4.26828028313586));
#69771=CARTESIAN_POINT('Ctrl Pts',(-0.0979068251135458,0.782198924659571,
-4.24709815181));
#69772=CARTESIAN_POINT('Ctrl Pts',(-0.522128456757134,0.530202381520183,
-4.22591602048414));
#69773=CARTESIAN_POINT('Ctrl Pts',(-0.713430002198875,0.217082423607711,
-4.21002942198974));
#69774=CARTESIAN_POINT('Ctrl Pts',(-0.728801516963504,-0.150270040849453,
-4.19414282349536));
#69775=CARTESIAN_POINT('Ctrl Pts',(-0.517055190066955,-0.594469360520892,
-4.17296069216949));
#69776=CARTESIAN_POINT('Ctrl Pts',(0.108410416329209,-0.838418218411172,
-4.14648302801217));
#69777=CARTESIAN_POINT('Ctrl Pts',(0.765134267955551,-0.361014749504757,
-4.11470983102339));
#69778=CARTESIAN_POINT('Ctrl Pts',(0.724030122361315,0.310641809240379,
-4.08823216686606));
#69779=CARTESIAN_POINT('Ctrl Pts',(0.36700394141324,0.646472984688444,-4.06705003554021));
#69780=CARTESIAN_POINT('Ctrl Pts',(-0.106765464783411,0.781237262572854,
-4.04586790421435));
#69781=CARTESIAN_POINT('Ctrl Pts',(-0.580982052052641,0.53280461647316,
-4.02468577288849));
#69782=CARTESIAN_POINT('Ctrl Pts',(-0.741189311015275,0.0661142644363603,
-4.00350364156263));
#69783=CARTESIAN_POINT('Ctrl Pts',(-0.684298628680863,-0.296382410851875,
-3.98761704306823));
#69784=CARTESIAN_POINT('Ctrl Pts',(-0.458208148131325,-0.586325872950584,
-3.97173044457385));
#69785=CARTESIAN_POINT('Ctrl Pts',(-0.0092635365213895,-0.787816017268254,
-3.95054831324798));
#69786=CARTESIAN_POINT('Ctrl Pts',(0.625381488841516,-0.568854920649197,
-3.92407064909066));
#69787=CARTESIAN_POINT('Ctrl Pts',(0.8168820851143,0.220149395591204,-3.89229745210187));
#69788=CARTESIAN_POINT('Ctrl Pts',(0.350754382146573,0.705470988162975,
-3.86581978794455));
#69789=CARTESIAN_POINT('Ctrl Pts',(-0.138768819289989,0.730316662645527,
-3.84463765661869));
#69790=CARTESIAN_POINT('Ctrl Pts',(-0.587111491572448,0.526336984608081,
-3.82345552529284));
#69791=CARTESIAN_POINT('Ctrl Pts',(-0.787731543960356,0.0299986465066971,
-3.80227339396697));
#69792=CARTESIAN_POINT('Ctrl Pts',(-0.607726915303675,-0.429419011154302,
-3.78109126264112));
#69793=CARTESIAN_POINT('Ctrl Pts',(-0.32970225863993,-0.668882326963883,
-3.76520466414672));
#69794=CARTESIAN_POINT('Ctrl Pts',(0.0303174320013971,-0.743514350649698,
-3.74931806565233));
#69795=CARTESIAN_POINT('Ctrl Pts',(0.502934025139974,-0.606462906144964,
-3.72813593432647));
#69796=CARTESIAN_POINT('Ctrl Pts',(0.844909638687625,-0.0287337742940667,
-3.70165827016915));
#69797=CARTESIAN_POINT('Ctrl Pts',(0.480105778669465,0.696606444592673,
-3.66988507318036));
#69798=CARTESIAN_POINT('Ctrl Pts',(-0.189346584630163,0.764765207513764,
-3.64340740902304));
#69799=CARTESIAN_POINT('Ctrl Pts',(-0.578540580729554,0.466808321898773,
-3.62222527769718));
#69800=CARTESIAN_POINT('Ctrl Pts',(-0.788216509313215,0.0211011693712273,
-3.60104314637132));
#69801=CARTESIAN_POINT('Ctrl Pts',(-0.619821445054221,-0.487075230732692,
-3.57986101504546));
#69802=CARTESIAN_POINT('Ctrl Pts',(-0.185218436367416,-0.720712717769618,
-3.55867888371961));
#69803=CARTESIAN_POINT('Ctrl Pts',(0.181706561352431,-0.723249522805478,
-3.54279228522521));
#69804=CARTESIAN_POINT('Ctrl Pts',(0.504423484624682,-0.547073746824225,
-3.52690568673082));
#69805=CARTESIAN_POINT('Ctrl Pts',(0.775926926901616,-0.136664897769372,
-3.50572355540496));
#69806=CARTESIAN_POINT('Ctrl Pts',(0.662583245660023,0.525053682877346,
-3.47924589124763));
#69807=CARTESIAN_POINT('Ctrl Pts',(-0.0850176543603167,0.841744673762138,
-3.44747269425885));
#69808=CARTESIAN_POINT('Ctrl Pts',(-0.63939083797011,0.460323047494419,
-3.42099503010152));
#69809=CARTESIAN_POINT('Ctrl Pts',(-0.743147815742249,-0.0187226307543114,
-3.39981289877567));
#69810=CARTESIAN_POINT('Ctrl Pts',(-0.614431277810804,-0.494170749590194,
-3.37863076744981));
#69811=CARTESIAN_POINT('Ctrl Pts',(-0.157112882430159,-0.772487181975783,
-3.35744863612394));
#69812=CARTESIAN_POINT('Ctrl Pts',(0.325383332868861,-0.669222218262672,
-3.3362665047981));
#69813=CARTESIAN_POINT('Ctrl Pts',(0.606692403305564,-0.433625961455501,
-3.32037990630369));
#69814=CARTESIAN_POINT('Ctrl Pts',(0.738616463059989,-0.0904348207382206,
-3.30449330780931));
#69815=CARTESIAN_POINT('Ctrl Pts',(0.679874730541545,0.398133446151352,
-3.28331117648344));
#69816=CARTESIAN_POINT('Ctrl Pts',(0.165120091127291,0.829115964650634,
-3.25683351232612));
#69817=CARTESIAN_POINT('Ctrl Pts',(-0.609705129431059,0.586533675508332,
-3.22506031533734));
#69818=CARTESIAN_POINT('Ctrl Pts',(-0.785329064884318,-0.0630572088075564,
-3.19858265118001));
#69819=CARTESIAN_POINT('Ctrl Pts',(-0.554300299964595,-0.49534875633638,
-3.17740051985415));
#69820=CARTESIAN_POINT('Ctrl Pts',(-0.148411245134259,-0.774405983461156,
-3.1562183885283));
#69821=CARTESIAN_POINT('Ctrl Pts',(0.380321452818095,-0.690490040962752,
-3.13503625720243));
#69822=CARTESIAN_POINT('Ctrl Pts',(0.681226812577487,-0.299437339940724,
-3.11385412587658));
#69823=CARTESIAN_POINT('Ctrl Pts',(0.743124194941543,0.0622380717034434,
-3.09796752738218));
#69824=CARTESIAN_POINT('Ctrl Pts',(0.621509885269368,0.409216567134883,
-3.0820809288878));
#69825=CARTESIAN_POINT('Ctrl Pts',(0.260461624868717,0.743572210443643,
-3.06089879756193));
#69826=CARTESIAN_POINT('Ctrl Pts',(-0.410877211556822,0.738835465009447,
-3.03442113340462));
#69827=CARTESIAN_POINT('Ctrl Pts',(-0.844405646303706,0.0523564881392667,
-3.00264793641582));
#69828=CARTESIAN_POINT('Ctrl Pts',(-0.557750364160292,-0.556446298409586,
-2.9761702722585));
#69829=CARTESIAN_POINT('Ctrl Pts',(-0.101817380520569,-0.736377915182664,
-2.95498814093264));
#69830=CARTESIAN_POINT('Ctrl Pts',(0.38819590164287,-0.686319507846331,
-2.93380600960679));
#69831=CARTESIAN_POINT('Ctrl Pts',(0.736867919625537,-0.280083154025966,
-2.91262387828092));
#69832=CARTESIAN_POINT('Ctrl Pts',(0.713066307922928,0.212765437114261,
-2.89144174695507));
#69833=CARTESIAN_POINT('Ctrl Pts',(0.526112470273849,0.528500534814524,
-2.87555514846067));
#69834=CARTESIAN_POINT('Ctrl Pts',(0.208801790582379,0.714237039472746,
-2.85966854996628));
#69835=CARTESIAN_POINT('Ctrl Pts',(-0.282831813570063,0.735354374030618,
-2.83848641864042));
#69836=CARTESIAN_POINT('Ctrl Pts',(-0.791453765717036,0.297151247792696,
-2.8120087544831));
#69837=CARTESIAN_POINT('Ctrl Pts',(-0.677491328337421,-0.506722406636456,
-2.78023555749431));
#69838=CARTESIAN_POINT('Ctrl Pts',(-0.064895345870056,-0.785179308068587,
-2.753757893337));
#69839=CARTESIAN_POINT('Ctrl Pts',(0.399091755209997,-0.627172212289608,
-2.73257576201113));
#69840=CARTESIAN_POINT('Ctrl Pts',(0.740169947485737,-0.271806868459416,
-2.71139363068528));
#69841=CARTESIAN_POINT('Ctrl Pts',(0.742946469580542,0.263536425338524,
-2.69021149935941));
#69842=CARTESIAN_POINT('Ctrl Pts',(0.405758370113191,0.623773064349805,
-2.66902936803356));
#69843=CARTESIAN_POINT('Ctrl Pts',(0.0588719914752158,0.743398436436768,
-2.65314276953916));
#69844=CARTESIAN_POINT('Ctrl Pts',(-0.303216270831923,0.679553257227116,
-2.63725617104477));
#69845=CARTESIAN_POINT('Ctrl Pts',(-0.691605246616418,0.377388490849861,
-2.61607403971891));
#69846=CARTESIAN_POINT('Ctrl Pts',(-0.795600372028744,-0.285863560742109,
-2.58959637556159));
#69847=CARTESIAN_POINT('Ctrl Pts',(-0.188349690923361,-0.824794817690396,
-2.5578231785728));
#69848=CARTESIAN_POINT('Ctrl Pts',(0.45882509086868,-0.640466617181587,
-2.53134551441548));
#69849=CARTESIAN_POINT('Ctrl Pts',(0.710185521922345,-0.219671885767667,
-2.51016338308962));
#69850=CARTESIAN_POINT('Ctrl Pts',(0.740105571376498,0.271982109926758,
-2.48898125176376));
#69851=CARTESIAN_POINT('Ctrl Pts',(0.395666032677899,0.6818132403579,-2.4677991204379));
#69852=CARTESIAN_POINT('Ctrl Pts',(-0.0945357012105535,0.738102765149872,
-2.44661698911204));
#69853=CARTESIAN_POINT('Ctrl Pts',(-0.436369087788938,0.604722387463148,
-2.43073039061765));
#69854=CARTESIAN_POINT('Ctrl Pts',(-0.671019104572567,0.321661464281676,
-2.41484379212326));
#69855=CARTESIAN_POINT('Ctrl Pts',(-0.771438521446857,-0.160070290188984,
-2.3936616607974));
#69856=CARTESIAN_POINT('Ctrl Pts',(-0.421344828368112,-0.73291640924452,
-2.36718399664008));
#69857=CARTESIAN_POINT('Ctrl Pts',(0.390374518970285,-0.750579664192001,
-2.33541079965129));
#69858=CARTESIAN_POINT('Ctrl Pts',(0.764319887009418,-0.191136239516684,
-2.30893313549396));
#69859=CARTESIAN_POINT('Ctrl Pts',(0.683502010213621,0.292308424406099,
-2.28775100416811));
#69860=CARTESIAN_POINT('Ctrl Pts',(0.38803339177511,0.686411401253109,-2.26656887284225));
#69861=CARTESIAN_POINT('Ctrl Pts',(-0.139800436685434,0.77580715519062,
-2.24538674151639));
#69862=CARTESIAN_POINT('Ctrl Pts',(-0.549866856672383,0.501377233885317,
-2.22420461019053));
#69863=CARTESIAN_POINT('Ctrl Pts',(-0.724065013976115,0.178429263890927,
-2.20831801169614));
#69864=CARTESIAN_POINT('Ctrl Pts',(-0.719672927365281,-0.189218429130693,
-2.19243141320174));
#69865=CARTESIAN_POINT('Ctrl Pts',(-0.484361466229776,-0.621396701153967,
-2.17124928187589));
#69866=CARTESIAN_POINT('Ctrl Pts',(0.153310054633789,-0.831380751810275,
-2.14477161771856));
#69867=CARTESIAN_POINT('Ctrl Pts',(0.783429437513418,-0.319375036277522,
-2.11299842072978));
#69868=CARTESIAN_POINT('Ctrl Pts',(0.706290106391243,0.349102044320172,
-2.08652075657245));
#69869=CARTESIAN_POINT('Ctrl Pts',(0.331732388356717,0.665261479014068,
-2.06533862524659));
#69870=CARTESIAN_POINT('Ctrl Pts',(-0.148594596082589,0.774370822615237,
-2.04415649392074));
#69871=CARTESIAN_POINT('Ctrl Pts',(-0.608775250603796,0.500812937527267,
-2.02297436259487));
#69872=CARTESIAN_POINT('Ctrl Pts',(-0.743671235528029,0.026187481235811,
-2.00179223126902));
#69873=CARTESIAN_POINT('Ctrl Pts',(-0.667382320392564,-0.33272809485271,
-1.98590563277462));
#69874=CARTESIAN_POINT('Ctrl Pts',(-0.426037087450199,-0.610102562215694,
-1.97001903428023));
#69875=CARTESIAN_POINT('Ctrl Pts',(0.0330867987414303,-0.787175427666758,
-1.94883690295438));
#69876=CARTESIAN_POINT('Ctrl Pts',(0.655047859759172,-0.534425138590393,
-1.92235923879705));
#69877=CARTESIAN_POINT('Ctrl Pts',(0.803870926086962,0.263730224949567,
-1.89058604180827));
#69878=CARTESIAN_POINT('Ctrl Pts',(0.312335778526887,0.723300983814258,
-1.86410837765094));
#69879=CARTESIAN_POINT('Ctrl Pts',(-0.17781525043291,0.721803955141782,
-1.84292624632508));
#69880=CARTESIAN_POINT('Ctrl Pts',(-0.614548264760971,0.494025257635711,
-1.82174411499922));
#69881=CARTESIAN_POINT('Ctrl Pts',(-0.788205373773664,-0.0123771118085124,
-1.80056198367336));
#69882=CARTESIAN_POINT('Ctrl Pts',(-0.583771915529394,-0.461457518482905,
-1.77937985234751));
#69883=CARTESIAN_POINT('Ctrl Pts',(-0.293280337215025,-0.68563386036567,
-1.76349325385311));
#69884=CARTESIAN_POINT('Ctrl Pts',(0.070229816409773,-0.740810710770472,
-1.74760665535872));
#69885=CARTESIAN_POINT('Ctrl Pts',(0.534798374515875,-0.578559062489274,
-1.72642452403286));
#69886=CARTESIAN_POINT('Ctrl Pts',(0.845232871318611,0.0167128864931346,
-1.69994685987554));
#69887=CARTESIAN_POINT('Ctrl Pts',(0.441976637270261,0.7214005471769,-1.66817366288675));
#69888=CARTESIAN_POINT('Ctrl Pts',(-0.230171182371692,0.753484690315798,
-1.64169599872943));
#69889=CARTESIAN_POINT('Ctrl Pts',(-0.602790690129551,0.435043212609942,
-1.62051386740357));
#69890=CARTESIAN_POINT('Ctrl Pts',(-0.788211491123012,-0.0212877937884581,
-1.59933173607771));
#69891=CARTESIAN_POINT('Ctrl Pts',(-0.592750543967491,-0.519680379433986,
-1.57814960475185));
#69892=CARTESIAN_POINT('Ctrl Pts',(-0.14621995018756,-0.729624846679722,
-1.55696747342599));
#69893=CARTESIAN_POINT('Ctrl Pts',(0.220311161111685,-0.712439568641789,
-1.5410808749316));
#69894=CARTESIAN_POINT('Ctrl Pts',(0.533094129652703,-0.519175678585803,
-1.52519427643721));
#69895=CARTESIAN_POINT('Ctrl Pts',(0.782150020565167,-0.0947693806205724,
-1.50401214511135));
#69896=CARTESIAN_POINT('Ctrl Pts',(0.633409604628127,0.559901955789828,
-1.47753448095402));
#69897=CARTESIAN_POINT('Ctrl Pts',(-0.130129858152316,0.835959518982299,
-1.44576128396524));
#69898=CARTESIAN_POINT('Ctrl Pts',(-0.663204501309733,0.425297238619271,
-1.41928361980792));
#69899=CARTESIAN_POINT('Ctrl Pts',(-0.741067805959503,-0.0586320724109774,
-1.39810148848206));
#69900=CARTESIAN_POINT('Ctrl Pts',(-0.586986854985309,-0.526475979487392,
-1.3769193571562));
#69901=CARTESIAN_POINT('Ctrl Pts',(-0.115372668219765,-0.779814113472083,
-1.35573722583034));
#69902=CARTESIAN_POINT('Ctrl Pts',(0.360876909130024,-0.650769196552833,
-1.33455509450448));
#69903=CARTESIAN_POINT('Ctrl Pts',(0.629118624691168,-0.400395932476321,
-1.31866849601009));
#69904=CARTESIAN_POINT('Ctrl Pts',(0.742409083329817,-0.0506111578071527,
-1.30278189751569));
#69905=CARTESIAN_POINT('Ctrl Pts',(0.657496750844895,0.434094359329509,
-1.28159976618984));
#69906=CARTESIAN_POINT('Ctrl Pts',(0.120325095948475,0.836791371022327,
-1.25512210203251));
#69907=CARTESIAN_POINT('Ctrl Pts',(-0.640344202902728,0.552920789235428,
-1.22334890504373));
#69908=CARTESIAN_POINT('Ctrl Pts',(-0.780805578144866,-0.105169391329118,
-1.1968712408864));
#69909=CARTESIAN_POINT('Ctrl Pts',(-0.526879461855956,-0.524420866880043,
-1.17568910956055));
#69910=CARTESIAN_POINT('Ctrl Pts',(-0.106580489249386,-0.781262519396717,
-1.15450697823469));
#69911=CARTESIAN_POINT('Ctrl Pts',(0.416878567618402,-0.669053932058423,
-1.13332484690883));
#69912=CARTESIAN_POINT('Ctrl Pts',(0.696334082128771,-0.262395763668439,
-1.11214271558297));
#69913=CARTESIAN_POINT('Ctrl Pts',(0.738705715153232,0.102083363369506,
-1.09625611708858));
#69914=CARTESIAN_POINT('Ctrl Pts',(0.598620640920461,0.442024959215177,
-1.08036951859418));
#69915=CARTESIAN_POINT('Ctrl Pts',(0.220125949978788,0.756494848838535,
-1.05918738726833));
#69916=CARTESIAN_POINT('Ctrl Pts',(-0.449988238412121,0.715687440593429,
-1.032709723111));
#69917=CARTESIAN_POINT('Ctrl Pts',(-0.845999083354694,0.00690277646287119,
-1.00093652612222));
#69918=CARTESIAN_POINT('Ctrl Pts',(-0.527041180719297,-0.585615527082987,
-0.97445886196489));
#69919=CARTESIAN_POINT('Ctrl Pts',(-0.0620975683374578,-0.740785464862379,
-0.953276730639033));
#69920=CARTESIAN_POINT('Ctrl Pts',(0.424517514770048,-0.664466255393287,
-0.932094599313175));
#69921=CARTESIAN_POINT('Ctrl Pts',(0.75085469976088,-0.240079411839319,
-0.910912467987315));
#69922=CARTESIAN_POINT('Ctrl Pts',(0.700601975886072,0.25077791391973,-0.889730336661459));
#69923=CARTESIAN_POINT('Ctrl Pts',(0.496950799454161,0.556009936600838,
-0.873843738167064));
#69924=CARTESIAN_POINT('Ctrl Pts',(0.170117226641474,0.724425886826345,
-0.857957139672669));
#69925=CARTESIAN_POINT('Ctrl Pts',(-0.321940795819329,0.719092493469208,
-0.836775008346812));
#69926=CARTESIAN_POINT('Ctrl Pts',(-0.806278901509358,0.254189418164704,
-0.810297344189489));
#69927=CARTESIAN_POINT('Ctrl Pts',(-0.64928126104417,-0.542398323574931,
-0.778524147200702));
#69928=CARTESIAN_POINT('Ctrl Pts',(-0.0226063174085712,-0.787532161986483,
-0.752046483043379));
#69929=CARTESIAN_POINT('Ctrl Pts',(0.432219069236098,-0.604818889509744,
-0.730864351717523));
#69930=CARTESIAN_POINT('Ctrl Pts',(0.753707191550731,-0.231637635903656,
-0.709682220391664));
#69931=CARTESIAN_POINT('Ctrl Pts',(0.727710545460163,0.303081286331367,
-0.688500089065805));
#69932=CARTESIAN_POINT('Ctrl Pts',(0.371650701813931,0.644677009447944,
-0.667317957739948));
#69933=CARTESIAN_POINT('Ctrl Pts',(0.0188369557358222,0.745487971757124,
-0.651431359245553));
#69934=CARTESIAN_POINT('Ctrl Pts',(-0.339297064946969,0.662276556588206,
-0.635544760751158));
#69935=CARTESIAN_POINT('Ctrl Pts',(-0.710886586537695,0.339676541111478,
-0.614362629425303));
#69936=CARTESIAN_POINT('Ctrl Pts',(-0.779088508642335,-0.32820576176058,
-0.587884965267977));
#69937=CARTESIAN_POINT('Ctrl Pts',(-0.143753347590996,-0.833724816004507,
-0.556111768279191));
#69938=CARTESIAN_POINT('Ctrl Pts',(0.492580529297411,-0.614884040031596,
-0.529634104121868));
#69939=CARTESIAN_POINT('Ctrl Pts',(0.720964373963307,-0.181189335785351,
-0.508451972796009));
#69940=CARTESIAN_POINT('Ctrl Pts',(0.724419896865446,0.311362083290472,
-0.48726984147015));
#69941=CARTESIAN_POINT('Ctrl Pts',(0.358453864430568,0.702090987400412,
-0.466087710144294));
#69942=CARTESIAN_POINT('Ctrl Pts',(-0.134064441091513,0.731955841893754,
-0.444905578818434));
#69943=CARTESIAN_POINT('Ctrl Pts',(-0.468236154978809,0.580398310702801,
-0.429018980324041));
#69944=CARTESIAN_POINT('Ctrl Pts',(-0.687335322162944,0.285136193611118,
-0.413132381829648));
#69945=CARTESIAN_POINT('Ctrl Pts',(-0.761721915252497,-0.201295514566145,
-0.391950250503788));
#69946=CARTESIAN_POINT('Ctrl Pts',(-0.381348782508604,-0.754500870785961,
-0.365472586346466));
#69947=CARTESIAN_POINT('Ctrl Pts',(0.430145374627856,-0.728515393750025,
-0.333699389357679));
#69948=CARTESIAN_POINT('Ctrl Pts',(0.773488578129993,-0.149787584417332,
-0.307221725200355));
#69949=CARTESIAN_POINT('Ctrl Pts',(0.666803717585622,0.32861960324679,-0.286039593874498));
#69950=CARTESIAN_POINT('Ctrl Pts',(0.350590505112842,0.706266072815195,
-0.264857462548639));
#69951=CARTESIAN_POINT('Ctrl Pts',(-0.181300858414558,0.767185934044253,
-0.243675331222782));
#69952=CARTESIAN_POINT('Ctrl Pts',(-0.57600272772074,0.471087443825438,
-0.222493199896921));
#69953=CARTESIAN_POINT('Ctrl Pts',(-0.732635320889055,0.139292989541286,
-0.206606601402529));
#69954=CARTESIAN_POINT('Ctrl Pts',(-0.708413622199826,-0.227679344522623,
-0.190720002908134));
#69955=CARTESIAN_POINT('Ctrl Pts',(-0.450377756802535,-0.646399890802347,
-0.169537871582277));
#69956=CARTESIAN_POINT('Ctrl Pts',(0.197993874424786,-0.822205995966851,
-0.143060207424953));
#69957=CARTESIAN_POINT('Ctrl Pts',(0.799063290594735,-0.276348436002072,
-0.111287010436166));
#69958=CARTESIAN_POINT('Ctrl Pts',(0.687176416166241,0.385773860169478,
-0.0848093462788429));
#69959=CARTESIAN_POINT('Ctrl Pts',(0.294603052440389,0.683176174939641,
-0.0636272149529848));
#69960=CARTESIAN_POINT('Ctrl Pts',(-0.0669663409722705,0.742568911483241,
-0.0477406164585896));
#69961=CARTESIAN_POINT('Ctrl Pts',(-0.415015231537065,0.618962097253398,
-0.0318540179641988));
#69962=CARTESIAN_POINT('Ctrl Pts',(-0.578394000517792,0.436565751468206,
-0.0212629523012676));
#69963=CARTESIAN_POINT('Ctrl Pts',(-0.633489757429965,0.331175816864348,
-0.0159674194698027));
#69964=CARTESIAN_POINT('Ctrl Pts',(0.392888236737129,-0.550964357679868,
-11.9089));
#69965=CARTESIAN_POINT('Ctrl Pts',(0.484548909927025,-0.485601871403322,
-11.9036044671685));
#69966=CARTESIAN_POINT('Ctrl Pts',(0.634341446219948,-0.308693578393974,
-11.8930134015056));
#69967=CARTESIAN_POINT('Ctrl Pts',(0.705002038108303,0.0337351900899797,
-11.8771268030112));
#69968=CARTESIAN_POINT('Ctrl Pts',(0.602308840879945,0.365053324407907,
-11.8612402045168));
#69969=CARTESIAN_POINT('Ctrl Pts',(0.272406965382598,0.694503928448386,
-11.840058073191));
#69970=CARTESIAN_POINT('Ctrl Pts',(-0.363000708994007,0.713347601796957,
-11.8135804090336));
#69971=CARTESIAN_POINT('Ctrl Pts',(-0.796709301451907,0.0787753187535436,
-11.7818072120449));
#69972=CARTESIAN_POINT('Ctrl Pts',(-0.54757461974353,-0.506340519423678,
-11.7553295478875));
#69973=CARTESIAN_POINT('Ctrl Pts',(-0.121403177164881,-0.693866619017976,
-11.7341474165617));
#69974=CARTESIAN_POINT('Ctrl Pts',(0.225850498452994,-0.668875211131948,
-11.7182608180673));
#69975=CARTESIAN_POINT('Ctrl Pts',(0.516608588870761,-0.478872034799853,
-11.7023742195729));
#69976=CARTESIAN_POINT('Ctrl Pts',(0.742947756127913,-0.0702747149864332,
-11.681192088247));
#69977=CARTESIAN_POINT('Ctrl Pts',(0.616681960998304,0.420553527772077,
-11.6600099569212));
#69978=CARTESIAN_POINT('Ctrl Pts',(0.221462490922912,0.667971079462276,
-11.6388278255953));
#69979=CARTESIAN_POINT('Ctrl Pts',(-0.241001769318581,0.705818539717338,
-11.6176456942695));
#69980=CARTESIAN_POINT('Ctrl Pts',(-0.739034910876422,0.308639768144774,
-11.5911680301121));
#69981=CARTESIAN_POINT('Ctrl Pts',(-0.657912727899525,-0.455665328876149,
-11.5593948331233));
#69982=CARTESIAN_POINT('Ctrl Pts',(-0.0897337187244002,-0.740423380881239,
-11.532917168966));
#69983=CARTESIAN_POINT('Ctrl Pts',(0.356717037324203,-0.607439441065005,
-11.5117350376402));
#69984=CARTESIAN_POINT('Ctrl Pts',(0.605099039586646,-0.36361113891817,
-11.4958484391458));
#69985=CARTESIAN_POINT('Ctrl Pts',(0.703772576709861,-0.0305614200295496,
-11.4799618406514));
#69986=CARTESIAN_POINT('Ctrl Pts',(0.611744859212238,0.427384163050785,
-11.4587797093255));
#69987=CARTESIAN_POINT('Ctrl Pts',(0.197790656500237,0.719753643173289,
-11.4375975779997));
#69988=CARTESIAN_POINT('Ctrl Pts',(-0.263619000263347,0.652485296666156,
-11.4164154466738));
#69989=CARTESIAN_POINT('Ctrl Pts',(-0.640600438706306,0.381955634449409,
-11.395233315348));
#69990=CARTESIAN_POINT('Ctrl Pts',(-0.763085658381697,-0.243173825061882,
-11.3687556511906));
#69991=CARTESIAN_POINT('Ctrl Pts',(-0.206478220428704,-0.773205223454543,
-11.3369824542018));
#69992=CARTESIAN_POINT('Ctrl Pts',(0.410920283938739,-0.622433291638274,
-11.3105047900445));
#69993=CARTESIAN_POINT('Ctrl Pts',(0.665114014783227,-0.232063101779371,
-11.2893226587187));
#69994=CARTESIAN_POINT('Ctrl Pts',(0.696585389017661,0.11457124582531,-11.2734360602242));
#69995=CARTESIAN_POINT('Ctrl Pts',(0.55619304910803,0.432295255177504,-11.2575494617299));
#69996=CARTESIAN_POINT('Ctrl Pts',(0.189598103717612,0.721762795994409,
-11.236367330404));
#69997=CARTESIAN_POINT('Ctrl Pts',(-0.315180024953703,0.676629880018334,
-11.2151851990782));
#69998=CARTESIAN_POINT('Ctrl Pts',(-0.623315925700859,0.326663901421167,
-11.1940030677523));
#69999=CARTESIAN_POINT('Ctrl Pts',(-0.735519671514959,-0.123571168586822,
-11.1728209364264));
#70000=CARTESIAN_POINT('Ctrl Pts',(-0.424197719174421,-0.679330206520831,
-11.1463432722691));
#70001=CARTESIAN_POINT('Ctrl Pts',(0.343160473225332,-0.722994096502876,
-11.1145700752803));
#70002=CARTESIAN_POINT('Ctrl Pts',(0.716133365261885,-0.208402697353022,
-11.088092411123));
#70003=CARTESIAN_POINT('Ctrl Pts',(0.657170405500786,0.253686804061263,
-11.0669102797971));
#70004=CARTESIAN_POINT('Ctrl Pts',(0.456763012508479,0.538261390715488,
-11.0510236813027));
#70005=CARTESIAN_POINT('Ctrl Pts',(0.144077853390088,0.689544391419175,
-11.0351370828084));
#70006=CARTESIAN_POINT('Ctrl Pts',(-0.322724961404119,0.672857766501242,
-11.0139549514825));
#70007=CARTESIAN_POINT('Ctrl Pts',(-0.67824531273211,0.311688527808011,
-10.9927728201566));
#70008=CARTESIAN_POINT('Ctrl Pts',(-0.686552342337786,-0.154524849061646,
-10.9715906888308));
#70009=CARTESIAN_POINT('Ctrl Pts',(-0.480612243469802,-0.570325251330041,
-10.9504085575049));
#70010=CARTESIAN_POINT('Ctrl Pts',(0.116446449284972,-0.792384665988189,
-10.9239308933476));
#70011=CARTESIAN_POINT('Ctrl Pts',(0.729585741366676,-0.32891369683002,
-10.8921576963588));
#70012=CARTESIAN_POINT('Ctrl Pts',(0.680740265357369,0.304748047120233,
-10.8656800322015));
#70013=CARTESIAN_POINT('Ctrl Pts',(0.336664480573665,0.618778606564363,
-10.8444979008756));
#70014=CARTESIAN_POINT('Ctrl Pts',(-0.00030424207012357,0.705944531650651,
-10.8286113023812));
#70015=CARTESIAN_POINT('Ctrl Pts',(-0.336563415811402,0.618833550086267,
-10.8127247038868));
#70016=CARTESIAN_POINT('Ctrl Pts',(-0.681554107221738,0.303929224629296,
-10.791542572561));
#70017=CARTESIAN_POINT('Ctrl Pts',(-0.718724672271428,-0.20149761308359,
-10.7703604412351));
#70018=CARTESIAN_POINT('Ctrl Pts',(-0.423251854828125,-0.562218743134393,
-10.7491783099093));
#70019=CARTESIAN_POINT('Ctrl Pts',(0.0028831951113741,-0.745822169195642,
-10.7279961785834));
#70020=CARTESIAN_POINT('Ctrl Pts',(0.601706547663041,-0.528566424343903,
-10.7015185144261));
#70021=CARTESIAN_POINT('Ctrl Pts',(0.769006630385937,0.221604098315976,
-10.6697453174373));
#70022=CARTESIAN_POINT('Ctrl Pts',(0.321574591885842,0.672955022981378,
-10.64326765328));
#70023=CARTESIAN_POINT('Ctrl Pts',(-0.143965254934612,0.689567938489952,
-10.6220855219541));
#70024=CARTESIAN_POINT('Ctrl Pts',(-0.457226793531636,0.537867487033261,
-10.6061989234597));
#70025=CARTESIAN_POINT('Ctrl Pts',(-0.657128942689954,0.253794106027293,
-10.5903123249653));
#70026=CARTESIAN_POINT('Ctrl Pts',(-0.716223601331694,-0.20955363883752,
-10.5691301936395));
#70027=CARTESIAN_POINT('Ctrl Pts',(-0.417365376642559,-0.61884778822427,
-10.5479480623136));
#70028=CARTESIAN_POINT('Ctrl Pts',(0.0413549888341567,-0.702511076528755,
-10.5267659309878));
#70029=CARTESIAN_POINT('Ctrl Pts',(0.485007333141031,-0.566592364647785,
-10.5055837996619));
#70030=CARTESIAN_POINT('Ctrl Pts',(0.800783960244305,-0.0133522829404121,
-10.4791061355046));
#70031=CARTESIAN_POINT('Ctrl Pts',(0.442673841413548,0.666722914032616,
-10.4473329385158));
#70032=CARTESIAN_POINT('Ctrl Pts',(-0.190537863945514,0.721092229541751,
-10.4208552743584));
#70033=CARTESIAN_POINT('Ctrl Pts',(-0.556122470942101,0.432386093364394,
-10.3996731430326));
#70034=CARTESIAN_POINT('Ctrl Pts',(-0.696683883965076,0.113970786406134,
-10.3837865445382));
#70035=CARTESIAN_POINT('Ctrl Pts',(-0.6651518747368,-0.231954476372266,
-10.3678999460438));
#70036=CARTESIAN_POINT('Ctrl Pts',(-0.410243995550251,-0.623368942737406,
-10.346717814718));
#70037=CARTESIAN_POINT('Ctrl Pts',(0.082500557995093,-0.741862588718796,
-10.3255356833921));
#70038=CARTESIAN_POINT('Ctrl Pts',(0.48629264022718,-0.508676238690136,
-10.3043535520662));
#70039=CARTESIAN_POINT('Ctrl Pts',(0.736453075250717,-0.117880824698104,
-10.2831714207404));
#70040=CARTESIAN_POINT('Ctrl Pts',(0.618993813089344,0.508212449475007,
-10.2566937565831));
#70041=CARTESIAN_POINT('Ctrl Pts',(-0.0942027572610254,0.79473606593157,
-10.2249205595943));
#70042=CARTESIAN_POINT('Ctrl Pts',(-0.612027012017135,0.42626472721044,
-10.1984428954369));
#70043=CARTESIAN_POINT('Ctrl Pts',(-0.703777625297934,-0.0304465195329539,
-10.1772607641111));
#70044=CARTESIAN_POINT('Ctrl Pts',(-0.604785322978651,-0.364132513572057,
-10.1613741656167));
#70045=CARTESIAN_POINT('Ctrl Pts',(-0.356816358110809,-0.607381249430332,
-10.1454875671223));
#70046=CARTESIAN_POINT('Ctrl Pts',(0.0908551895918876,-0.740698527863264,
-10.1243054357964));
#70047=CARTESIAN_POINT('Ctrl Pts',(0.543127711937286,-0.512033916001494,
-10.1031233044706));
#70048=CARTESIAN_POINT('Ctrl Pts',(0.69994058004243,-0.0729056387183608,
-10.0819411731447));
#70049=CARTESIAN_POINT('Ctrl Pts',(0.637628208112178,0.386897000631171,
-10.0607590418189));
#70050=CARTESIAN_POINT('Ctrl Pts',(0.142798839180318,0.788062006426542,
-10.0342813776615));
#70051=CARTESIAN_POINT('Ctrl Pts',(-0.586274794331389,0.544758147712961,
-10.0025081806728));
#70052=CARTESIAN_POINT('Ctrl Pts',(-0.742424871886001,-0.071302108716839,
-9.97603051651542));
#70053=CARTESIAN_POINT('Ctrl Pts',(-0.516703214563073,-0.478798208519891,
-9.95484838518958));
#70054=CARTESIAN_POINT('Ctrl Pts',(-0.225239754106489,-0.669047701962083,
-9.93896178669518));
#70055=CARTESIAN_POINT('Ctrl Pts',(0.12122757218792,-0.693926344302069,
-9.92307518820078));
#70056=CARTESIAN_POINT('Ctrl Pts',(0.54874197779906,-0.505738288500843,
-9.90189305687493));
#70057=CARTESIAN_POINT('Ctrl Pts',(0.745433350289229,-0.0386725081502612,
-9.88071092554906));
#70058=CARTESIAN_POINT('Ctrl Pts',(0.580683923966688,0.397540222108045,
-9.85952879422322));
#70059=CARTESIAN_POINT('Ctrl Pts',(0.235535653683076,0.707659506204665,
-9.83834666289734));
#70060=CARTESIAN_POINT('Ctrl Pts',(-0.401313885472845,0.693094798545597,
-9.81186899874004));
#70061=CARTESIAN_POINT('Ctrl Pts',(-0.799503770929198,0.0356832487024724,
-9.78009580175124));
#70062=CARTESIAN_POINT('Ctrl Pts',(-0.519711826341081,-0.534956352110741,
-9.75361813759391));
#70063=CARTESIAN_POINT('Ctrl Pts',(-0.0838752645359608,-0.69942467530156,
-9.73243600626807));
#70064=CARTESIAN_POINT('Ctrl Pts',(0.261433978866206,-0.655751514695071,
-9.71654940777366));
#70065=CARTESIAN_POINT('Ctrl Pts',(0.541613442530161,-0.450427324266235,
-9.70066280927928));
#70066=CARTESIAN_POINT('Ctrl Pts',(0.745637002453177,-0.0302396300775194,
-9.6794806779534));
#70067=CARTESIAN_POINT('Ctrl Pts',(0.593197195641168,0.453082254887026,
-9.65829854662756));
#70068=CARTESIAN_POINT('Ctrl Pts',(0.185243328053068,0.678908651556959,
-9.6371164153017));
#70069=CARTESIAN_POINT('Ctrl Pts',(-0.278581983793115,0.691846152828526,
-9.61593428397583));
#70070=CARTESIAN_POINT('Ctrl Pts',(-0.754554355140179,0.268478974192128,
-9.58945661981852));
#70071=CARTESIAN_POINT('Ctrl Pts',(-0.632474069342684,-0.490363258796042,
-9.55768342282974));
#70072=CARTESIAN_POINT('Ctrl Pts',(-0.0498142904822183,-0.744175528733757,
-9.5312057586724));
#70073=CARTESIAN_POINT('Ctrl Pts',(0.388845301867087,-0.587391919962783,
-9.51002362734656));
#70074=CARTESIAN_POINT('Ctrl Pts',(0.623764909652236,-0.33056786265037,
-9.49413702885215));
#70075=CARTESIAN_POINT('Ctrl Pts',(0.704398011625223,0.00730320432709524,
-9.47825043035776));
#70076=CARTESIAN_POINT('Ctrl Pts',(0.587893373397589,0.459641551831196,
-9.45706829903191));
#70077=CARTESIAN_POINT('Ctrl Pts',(0.158825559311775,0.729342775599619,
-9.43588616770604));
#70078=CARTESIAN_POINT('Ctrl Pts',(-0.298302397103462,0.637375656602442,
-9.4147040363802));
#70079=CARTESIAN_POINT('Ctrl Pts',(-0.660200912976761,0.346978061817164,
-9.39352190505432));
#70080=CARTESIAN_POINT('Ctrl Pts',(-0.748914914372129,-0.283830381522591,
-9.36704424089701));
#70081=CARTESIAN_POINT('Ctrl Pts',(-0.164628083532023,-0.783183993759156,
-9.33527104390821));
#70082=CARTESIAN_POINT('Ctrl Pts',(0.443775836884319,-0.599451155391359,
-9.30879337975089));
#70083=CARTESIAN_POINT('Ctrl Pts',(0.676623900661522,-0.195984778682572,
-9.28761124842504));
#70084=CARTESIAN_POINT('Ctrl Pts',(0.689421792526712,0.151839936511941,
-9.27172464993064));
#70085=CARTESIAN_POINT('Ctrl Pts',(0.532157948497518,0.461560194802287,
-9.25583805143624));
#70086=CARTESIAN_POINT('Ctrl Pts',(0.150536857936622,0.730908769311981,
-9.2346559201104));
#70087=CARTESIAN_POINT('Ctrl Pts',(-0.351086430223958,0.658714476175113,
-9.21347378878452));
#70088=CARTESIAN_POINT('Ctrl Pts',(-0.639970023186198,0.292695092494087,
-9.19229165745868));
#70089=CARTESIAN_POINT('Ctrl Pts',(-0.72781616183648,-0.162919168446685,
-9.17110952613282));
#70090=CARTESIAN_POINT('Ctrl Pts',(-0.387077784779294,-0.701144794585703,
-9.14463186197549));
#70091=CARTESIAN_POINT('Ctrl Pts',(0.381518042580854,-0.703508036310348,
-9.11285866498672));
#70092=CARTESIAN_POINT('Ctrl Pts',(0.726298025262084,-0.169616802242028,
-9.08638100082937));
#70093=CARTESIAN_POINT('Ctrl Pts',(0.642587744543107,0.288636323051471,
-9.06519886950353));
#70094=CARTESIAN_POINT('Ctrl Pts',(0.427177008054458,0.562029872978596,
-9.04931227100912));
#70095=CARTESIAN_POINT('Ctrl Pts',(0.106813790756512,0.696290679012175,
-9.03342567251474));
#70096=CARTESIAN_POINT('Ctrl Pts',(-0.358417752115536,0.654542351282965,
-9.01224354118889));
#70097=CARTESIAN_POINT('Ctrl Pts',(-0.69401526503328,0.274789473071372,
-8.99106140986302));
#70098=CARTESIAN_POINT('Ctrl Pts',(-0.677256151716331,-0.191196633624784,
-8.96987927853717));
#70099=CARTESIAN_POINT('Ctrl Pts',(-0.449268676104613,-0.595329049811071,
-8.9486971472113));
#70100=CARTESIAN_POINT('Ctrl Pts',(0.158860648830693,-0.784981865202862,
-8.92221948305397));
#70101=CARTESIAN_POINT('Ctrl Pts',(0.746207180183646,-0.289230735244962,
-8.89044628606521));
#70102=CARTESIAN_POINT('Ctrl Pts',(0.663379532687123,0.340890417457322,
-8.86396862190785));
#70103=CARTESIAN_POINT('Ctrl Pts',(0.302925054514254,0.635976688070566,
-8.84278649058203));
#70104=CARTESIAN_POINT('Ctrl Pts',(-0.0382410075393195,0.704908078881972,
-8.8268998920876));
#70105=CARTESIAN_POINT('Ctrl Pts',(-0.36933296774987,0.599852527299907,
-8.81101329359323));
#70106=CARTESIAN_POINT('Ctrl Pts',(-0.696902296093017,0.266863568804114,
-8.78983116226737));
#70107=CARTESIAN_POINT('Ctrl Pts',(-0.706857692602032,-0.239830450567451,
-8.7686490309415));
#70108=CARTESIAN_POINT('Ctrl Pts',(-0.392426815119199,-0.584151729024632,
-8.74746689961565));
#70109=CARTESIAN_POINT('Ctrl Pts',(0.0429592438378583,-0.744589500494483,
-8.72628476828979));
#70110=CARTESIAN_POINT('Ctrl Pts',(0.629242040014653,-0.495467142727417,
-8.69980710413247));
#70111=CARTESIAN_POINT('Ctrl Pts',(0.755986477075477,0.262610015892347,
-8.66803390714367));
#70112=CARTESIAN_POINT('Ctrl Pts',(0.284945549871296,0.689263893375359,
-8.64155624298637));
#70113=CARTESIAN_POINT('Ctrl Pts',(-0.18081435535875,0.680834859064861,
-8.62037411166049));
#70114=CARTESIAN_POINT('Ctrl Pts',(-0.485470897563107,0.512519055206698,
-8.60448751316611));
#70115=CARTESIAN_POINT('Ctrl Pts',(-0.669818183142776,0.218113495928887,
-8.58860091467172));
#70116=CARTESIAN_POINT('Ctrl Pts',(-0.703927307830937,-0.247740428562784,
-8.56741878334585));
#70117=CARTESIAN_POINT('Ctrl Pts',(-0.383505618497739,-0.64038260687711,
-8.54623665202));
#70118=CARTESIAN_POINT('Ctrl Pts',(0.0790479225720012,-0.699273532806809,
-8.52505452069413));
#70119=CARTESIAN_POINT('Ctrl Pts',(0.514754958365451,-0.539709508639534,
-8.50387238936828));
#70120=CARTESIAN_POINT('Ctrl Pts',(0.800344359486549,0.0297008532257883,
-8.47739472521096));
#70121=CARTESIAN_POINT('Ctrl Pts',(0.406204720035274,0.689548620032724,
-8.44562152822216));
#70122=CARTESIAN_POINT('Ctrl Pts',(-0.229013770145407,0.709810801683236,
-8.41914386406485));
#70123=CARTESIAN_POINT('Ctrl Pts',(-0.578555136750526,0.401875465985733,
-8.39796173273899));
#70124=CARTESIAN_POINT('Ctrl Pts',(-0.701801911913352,0.0763665552808169,
-8.3820751342446));
#70125=CARTESIAN_POINT('Ctrl Pts',(-0.651725567877458,-0.267364320263228,
-8.3661885357502));
#70126=CARTESIAN_POINT('Ctrl Pts',(-0.376151562716211,-0.644514527780979,
-8.34500640442435));
#70127=CARTESIAN_POINT('Ctrl Pts',(0.122248771729135,-0.736357033252738,
-8.32382427309847));
#70128=CARTESIAN_POINT('Ctrl Pts',(0.512926016390591,-0.481808000615124,
-8.30264214177264));
#70129=CARTESIAN_POINT('Ctrl Pts',(0.741723760032622,-0.0781337614659248,
-8.28146001044675));
#70130=CARTESIAN_POINT('Ctrl Pts',(0.590788201416899,0.540742577860168,
-8.25498234628945));
#70131=CARTESIAN_POINT('Ctrl Pts',(-0.136775462740103,0.788525235335051,
-8.22320914930065));
#70132=CARTESIAN_POINT('Ctrl Pts',(-0.634049934714981,0.39275865539838,
-8.19673148514334));
#70133=CARTESIAN_POINT('Ctrl Pts',(-0.701124468604536,-0.0682232800858731,
-8.17554935381747));
#70134=CARTESIAN_POINT('Ctrl Pts',(-0.584343046747153,-0.396107280984521,
-8.15966275532308));
#70135=CARTESIAN_POINT('Ctrl Pts',(-0.323660302086688,-0.625678754975878,
-8.14377615682868));
#70136=CARTESIAN_POINT('Ctrl Pts',(0.130528774517201,-0.734745679590988,
-8.12259402550284));
#70137=CARTESIAN_POINT('Ctrl Pts',(0.569859400741034,-0.482106529718409,
-8.10141189417698));
#70138=CARTESIAN_POINT('Ctrl Pts',(0.702847075744717,-0.0351857338159052,
-8.08022976285111));
#70139=CARTESIAN_POINT('Ctrl Pts',(0.615915117961009,0.420603837767584,
-8.05904763152526));
#70140=CARTESIAN_POINT('Ctrl Pts',(0.100242323565696,0.794597200479857,
-8.03256996736792));
#70141=CARTESIAN_POINT('Ctrl Pts',(-0.614702723239511,0.512464765627743,
-8.00079677037916));
#70142=CARTESIAN_POINT('Ctrl Pts',(-0.737520304544937,-0.111096721312356,
-7.9743191062218));
#70143=CARTESIAN_POINT('Ctrl Pts',(-0.490226125422572,-0.505873781070776,
-7.95313697489597));
#70144=CARTESIAN_POINT('Ctrl Pts',(-0.188959895740458,-0.680185218989984,
-7.93725037640156));
#70145=CARTESIAN_POINT('Ctrl Pts',(0.158343748144318,-0.68640888178885,
-7.92136377790718));
#70146=CARTESIAN_POINT('Ctrl Pts',(0.57512722912829,-0.475518290888796,
-7.9001816465813));
#70147=CARTESIAN_POINT('Ctrl Pts',(0.746434431978506,0.00144269434815235,
-7.87899951525548));
#70148=CARTESIAN_POINT('Ctrl Pts',(0.558481156467344,0.428171514253297,
-7.85781738392959));
#70149=CARTESIAN_POINT('Ctrl Pts',(0.197165933085699,0.719294526399437,
-7.83663525260375));
#70150=CARTESIAN_POINT('Ctrl Pts',(-0.437980644554784,0.670526799941397,
-7.81015758844643));
#70151=CARTESIAN_POINT('Ctrl Pts',(-0.80026607813319,-0.00733335920928448,
-7.77838439145762));
#70152=CARTESIAN_POINT('Ctrl Pts',(-0.490212471272208,-0.562112456819458,
-7.75190672730032));
#70153=CARTESIAN_POINT('Ctrl Pts',(-0.0461672328563757,-0.702921420239883,
-7.73072459597445));
#70154=CARTESIAN_POINT('Ctrl Pts',(0.296296052364626,-0.640754573673755,
-7.71483799748007));
#70155=CARTESIAN_POINT('Ctrl Pts',(0.565036603409811,-0.420670336941072,
-7.69895139898565));
#70156=CARTESIAN_POINT('Ctrl Pts',(0.746184610028158,0.00987433095006524,
-7.67776926765981));
#70157=CARTESIAN_POINT('Ctrl Pts',(0.56799153737738,0.484305746484325,-7.65658713633396));
#70158=CARTESIAN_POINT('Ctrl Pts',(0.148491341379806,0.687882525786409,
-7.63540500500808));
#70159=CARTESIAN_POINT('Ctrl Pts',(-0.315358990972195,0.675875526773047,
-7.61422287368224));
#70160=CARTESIAN_POINT('Ctrl Pts',(-0.767891973600488,0.227541537579893,
-7.5877452095249));
#70161=CARTESIAN_POINT('Ctrl Pts',(-0.605208187534785,-0.523643603712323,
-7.55597201253612));
#70162=CARTESIAN_POINT('Ctrl Pts',(-0.00975058277995205,-0.745777183371727,
-7.5294943483788));
#70163=CARTESIAN_POINT('Ctrl Pts',(0.419849643624006,-0.565646721170082,
-7.50831221705293));
#70164=CARTESIAN_POINT('Ctrl Pts',(0.640628155804832,-0.296569284182963,
-7.49242561855854));
#70165=CARTESIAN_POINT('Ctrl Pts',(0.702987671893402,0.0451467467366845,
-7.47653902006416));
#70166=CARTESIAN_POINT('Ctrl Pts',(0.562342884997569,0.490570539624217,
-7.45535688873828));
#70167=CARTESIAN_POINT('Ctrl Pts',(0.119401435125199,0.736824090200709,
-7.43417475741245));
#70168=CARTESIAN_POINT('Ctrl Pts',(-0.332123683053873,0.620423973506661,
-7.41299262608657));
#70169=CARTESIAN_POINT('Ctrl Pts',(-0.677893386628627,0.310997712600778,
-7.39181049476072));
#70170=CARTESIAN_POINT('Ctrl Pts',(-0.732579775894945,-0.323666659379656,
-7.3653328306034));
#70171=CARTESIAN_POINT('Ctrl Pts',(-0.122302166900868,-0.790899332367473,
-7.3335596336146));
#70172=CARTESIAN_POINT('Ctrl Pts',(0.475348861974375,-0.574736583594672,
-7.30708196945728));
#70173=CARTESIAN_POINT('Ctrl Pts',(0.686178318089926,-0.159340052105395,
-7.28589983813143));
#70174=CARTESIAN_POINT('Ctrl Pts',(0.680265741730897,0.18866980404402,-7.27001323963702));
#70175=CARTESIAN_POINT('Ctrl Pts',(0.50658489163482,0.489491208442347,-7.25412664114265));
#70176=CARTESIAN_POINT('Ctrl Pts',(0.111040555138311,0.737942389193872,
-7.23294450981677));
#70177=CARTESIAN_POINT('Ctrl Pts',(-0.385978182755204,0.638895363144113,
-7.21176237849093));
#70178=CARTESIAN_POINT('Ctrl Pts',(-0.654774583609806,0.257880383910193,
-7.19058024716506));
#70179=CARTESIAN_POINT('Ctrl Pts',(-0.718009236529222,-0.201796325874554,
-7.16939811583921));
#70180=CARTESIAN_POINT('Ctrl Pts',(-0.348839181256874,-0.720933048253655,
-7.14292045168188));
#70181=CARTESIAN_POINT('Ctrl Pts',(0.418773010672415,-0.681988811858619,
-7.1111472546931));
#70182=CARTESIAN_POINT('Ctrl Pts',(0.7343636570957,-0.130340708297302,-7.08466959053577));
#70183=CARTESIAN_POINT('Ctrl Pts',(0.626147981225155,0.322751672388126,
-7.06348745920991));
#70184=CARTESIAN_POINT('Ctrl Pts',(0.396356446240715,0.58417406811166,-7.04760086071553));
#70185=CARTESIAN_POINT('Ctrl Pts',(0.069241032314998,0.70102466077804,-7.03171426222112));
#70186=CARTESIAN_POINT('Ctrl Pts',(-0.393074702260597,0.634335284449263,
-7.01053213089527));
#70187=CARTESIAN_POINT('Ctrl Pts',(-0.707779487537858,0.237096266589547,
-6.98934999956941));
#70188=CARTESIAN_POINT('Ctrl Pts',(-0.666002665755798,-0.227315852841898,
-6.96816786824355));
#70189=CARTESIAN_POINT('Ctrl Pts',(-0.416626705641162,-0.618612325309093,
-6.9469857369177));
#70190=CARTESIAN_POINT('Ctrl Pts',(0.200815735222948,-0.77531043778035,
-6.92050807276037));
#70191=CARTESIAN_POINT('Ctrl Pts',(0.760672052637908,-0.248711886132582,
-6.88873487577159));
#70192=CARTESIAN_POINT('Ctrl Pts',(0.644101608620266,0.376047601873901,
-6.86225721161426));
#70193=CARTESIAN_POINT('Ctrl Pts',(0.268310163838186,0.651336773415186,
-6.8410750802884));
#70194=CARTESIAN_POINT('Ctrl Pts',(-0.07606725508181,0.701834415681397,
-6.825188481794));
#70195=CARTESIAN_POINT('Ctrl Pts',(-0.401035133744832,0.579137908513486,
-6.80930188329962));
#70196=CARTESIAN_POINT('Ctrl Pts',(-0.710236411541561,0.229026667389746,
-6.78811975197375));
#70197=CARTESIAN_POINT('Ctrl Pts',(-0.692947868044057,-0.277470169173608,
-6.76693762064789));
#70198=CARTESIAN_POINT('Ctrl Pts',(-0.360467647394768,-0.604396494803816,
-6.74575548932204));
#70199=CARTESIAN_POINT('Ctrl Pts',(0.0829111387628172,-0.741204940581804,
-6.72457335799618));
#70200=CARTESIAN_POINT('Ctrl Pts',(0.654958999580732,-0.460935942740932,
-6.69809569383886));
#70201=CARTESIAN_POINT('Ctrl Pts',(0.740781494882939,0.3028569808165,-6.66632249685007));
#70202=CARTESIAN_POINT('Ctrl Pts',(0.247493004655936,0.703580765593753,
-6.63984483269275));
#70203=CARTESIAN_POINT('Ctrl Pts',(-0.217140895580519,0.670134141730119,
-6.61866270136689));
#70204=CARTESIAN_POINT('Ctrl Pts',(-0.512311972790511,0.485689424288953,
-6.6027761028725));
#70205=CARTESIAN_POINT('Ctrl Pts',(-0.680571624160622,0.181802529862302,
-6.5868895043781));
#70206=CARTESIAN_POINT('Ctrl Pts',(-0.689596638591978,-0.285211239524086,
-6.56570737305225));
#70207=CARTESIAN_POINT('Ctrl Pts',(-0.34853751448554,-0.660066695636425,
-6.54452524172639));
#70208=CARTESIAN_POINT('Ctrl Pts',(0.116512404375386,-0.694015063241657,
-6.52334311040052));
#70209=CARTESIAN_POINT('Ctrl Pts',(0.543014923912942,-0.511266870913038,
-6.50216097907468));
#70210=CARTESIAN_POINT('Ctrl Pts',(0.797591731359379,0.0726681501291486,
-6.47568331491733));
#70211=CARTESIAN_POINT('Ctrl Pts',(0.368561656490527,0.710381509762504,
-6.44391011792857));
#70212=CARTESIAN_POINT('Ctrl Pts',(-0.266827825705201,0.696477986286548,
-6.41743245377122));
#70213=CARTESIAN_POINT('Ctrl Pts',(-0.599315746240538,0.370203414794835,
-6.39625032244539));
#70214=CARTESIAN_POINT('Ctrl Pts',(-0.704891729413253,0.0385415976514491,
-6.38036372395098));
#70215=CARTESIAN_POINT('Ctrl Pts',(-0.636415707053117,-0.30200142601737,
-6.36447712545659));
#70216=CARTESIAN_POINT('Ctrl Pts',(-0.340972135963656,-0.663797545482861,
-6.34329499413074));
#70217=CARTESIAN_POINT('Ctrl Pts',(0.161643869936548,-0.728723180265365,
-6.32211286280486));
#70218=CARTESIAN_POINT('Ctrl Pts',(0.538076797651925,-0.453547551601197,
-6.30093073147902));
#70219=CARTESIAN_POINT('Ctrl Pts',(0.744851349578635,-0.038160346185337,
-6.27974860015315));
#70220=CARTESIAN_POINT('Ctrl Pts',(0.560874095982173,0.57170878506611,-6.25327093599583));
#70221=CARTESIAN_POINT('Ctrl Pts',(-0.178950953192254,0.780037574273926,
-6.22149773900705));
#70222=CARTESIAN_POINT('Ctrl Pts',(-0.654243696240302,0.358114047435898,
-6.19502007484972));
#70223=CARTESIAN_POINT('Ctrl Pts',(-0.696440513048951,-0.105798096922755,
-6.17383794352387));
#70224=CARTESIAN_POINT('Ctrl Pts',(-0.562221864267348,-0.426947701728367,
-6.15795134502947));
#70225=CARTESIAN_POINT('Ctrl Pts',(-0.289550464019102,-0.642148606418798,
-6.14206474653509));
#70226=CARTESIAN_POINT('Ctrl Pts',(0.169783162631269,-0.726713697646756,
-6.1208826152092));
#70227=CARTESIAN_POINT('Ctrl Pts',(0.595024636138863,-0.450700878954778,
-6.09970048388339));
#70228=CARTESIAN_POINT('Ctrl Pts',(0.70362826836473,0.00253654546368757,
-6.07851835255749));
#70229=CARTESIAN_POINT('Ctrl Pts',(0.592641591588357,0.453327123043412,
-6.05733622123166));
#70230=CARTESIAN_POINT('Ctrl Pts',(0.0569329064749938,0.798344967018745,
-6.03085855707431));
#70231=CARTESIAN_POINT('Ctrl Pts',(-0.640560403072364,0.479540489150726,
-5.99908536008555));
#70232=CARTESIAN_POINT('Ctrl Pts',(-0.74990911679165,-0.278210377237643,
-5.96731216309674));
#70233=CARTESIAN_POINT('Ctrl Pts',(-0.172598743972036,-0.781008560151051,
-5.93553896610797));
#70234=CARTESIAN_POINT('Ctrl Pts',(0.562958377491915,-0.568642748947718,
-5.90376576911917));
#70235=CARTESIAN_POINT('Ctrl Pts',(0.78296431633078,0.166020846752831,-5.87199257213039));
#70236=CARTESIAN_POINT('Ctrl Pts',(0.367652295433943,0.649277541756489,
-5.84551490797305));
#70237=CARTESIAN_POINT('Ctrl Pts',(-0.094108426135513,0.697311105773554,
-5.82433277664721));
#70238=CARTESIAN_POINT('Ctrl Pts',(-0.528139077188013,0.527498545068882,
-5.80315064532134));
#70239=CARTESIAN_POINT('Ctrl Pts',(-0.743143845220938,0.0683838136603718,
-5.78196851399549));
#70240=CARTESIAN_POINT('Ctrl Pts',(-0.596304988912091,-0.374986218597206,
-5.76078638266963));
#70241=CARTESIAN_POINT('Ctrl Pts',(-0.345699947738929,-0.615523607024695,
-5.74489978417524));
#70242=CARTESIAN_POINT('Ctrl Pts',(-0.009161937171944,-0.704371126917918,
-5.72901318568084));
#70243=CARTESIAN_POINT('Ctrl Pts',(0.44456117416937,-0.598870476365504,
-5.70783105435499));
#70244=CARTESIAN_POINT('Ctrl Pts',(0.797221488507143,-0.0701424207596342,
-5.68135339019766));
#70245=CARTESIAN_POINT('Ctrl Pts',(0.489274781214441,0.634066932534056,
-5.64958019320888));
#70246=CARTESIAN_POINT('Ctrl Pts',(-0.140080473677338,0.732555257905117,
-5.62310252905155));
#70247=CARTESIAN_POINT('Ctrl Pts',(-0.523138810580797,0.470699274058183,
-5.60192039772569));
#70248=CARTESIAN_POINT('Ctrl Pts',(-0.744016619254324,0.0600456860856954,
-5.58073826639983));
#70249=CARTESIAN_POINT('Ctrl Pts',(-0.610687717749323,-0.428893565214981,
-5.55955613507398));
#70250=CARTESIAN_POINT('Ctrl Pts',(-0.211749126753277,-0.671857217583966,
-5.53837400374811));
#70251=CARTESIAN_POINT('Ctrl Pts',(0.134970931816977,-0.692921822797631,
-5.52248740525373));
#70252=CARTESIAN_POINT('Ctrl Pts',(0.448993413533046,-0.542802769541158,
-5.50660080675932));
#70253=CARTESIAN_POINT('Ctrl Pts',(0.726520552090549,-0.168661084255895,
-5.48541867543347));
#70254=CARTESIAN_POINT('Ctrl Pts',(0.65304184941208,0.462618554495975,-5.45894101127615));
#70255=CARTESIAN_POINT('Ctrl Pts',(-0.0375440690826849,0.800014795396159,
-5.42716781428736));
#70256=CARTESIAN_POINT('Ctrl Pts',(-0.580989448745449,0.467664710376834,
-5.40069015013004));
#70257=CARTESIAN_POINT('Ctrl Pts',(-0.703439922458687,0.0201078062197571,
-5.37950801880418));
#70258=CARTESIAN_POINT('Ctrl Pts',(-0.605953346375472,-0.435874963388025,
-5.35832588747833));
#70259=CARTESIAN_POINT('Ctrl Pts',(-0.187815285885199,-0.722228768117197,
-5.33714375615245));
#70260=CARTESIAN_POINT('Ctrl Pts',(0.273535159807509,-0.649159773727578,
-5.31596162482661));
#70261=CARTESIAN_POINT('Ctrl Pts',(0.551438224564908,-0.44076485660649,
-5.3000750263322));
#70262=CARTESIAN_POINT('Ctrl Pts',(0.693603344904396,-0.123062327230168,
-5.28418842783782));
#70263=CARTESIAN_POINT('Ctrl Pts',(0.662930453897055,0.341762921281637,
-5.26300629651195));
#70264=CARTESIAN_POINT('Ctrl Pts',(0.198265258367223,0.775351830664549,
-5.23652863235464));
#70265=CARTESIAN_POINT('Ctrl Pts',(-0.546507260958737,0.58545968961291,
-5.20475543536584));
#70266=CARTESIAN_POINT('Ctrl Pts',(-0.745568705556984,-0.0196551817061931,
-5.17827777120853));
#70267=CARTESIAN_POINT('Ctrl Pts',(-0.549172285849032,-0.440047552208631,
-5.15709563988267));
#70268=CARTESIAN_POINT('Ctrl Pts',(-0.179687362077751,-0.724485261766983,
-5.1359135085568));
#70269=CARTESIAN_POINT('Ctrl Pts',(0.324385456870523,-0.67205881440986,
-5.11473137723096));
#70270=CARTESIAN_POINT('Ctrl Pts',(0.628721139150488,-0.317709969564103,
-5.09354924590509));
#70271=CARTESIAN_POINT('Ctrl Pts',(0.705631348411274,0.0210279449736901,
-5.0776626474107));
#70272=CARTESIAN_POINT('Ctrl Pts',(0.608322795378933,0.355208830188862,
-5.0617760489163));
#70273=CARTESIAN_POINT('Ctrl Pts',(0.284038448676206,0.689638195560499,
-5.04059391759044));
#70274=CARTESIAN_POINT('Ctrl Pts',(-0.350809927077043,0.719313540142401,
-5.01411625343312));
#70275=CARTESIAN_POINT('Ctrl Pts',(-0.795541563970066,0.0924491992412632,
-4.98234305644434));
#70276=CARTESIAN_POINT('Ctrl Pts',(-0.555541790830451,-0.497626706998958,
-4.95586539228701));
#70277=CARTESIAN_POINT('Ctrl Pts',(-0.133708223738798,-0.690908212899286,
-4.93468326096116));
#70278=CARTESIAN_POINT('Ctrl Pts',(0.332041232394348,-0.668517062310377,
-4.91350112963529));
#70279=CARTESIAN_POINT('Ctrl Pts',(0.682302518044435,-0.302245344918345,
-4.89231899830944));
#70280=CARTESIAN_POINT('Ctrl Pts',(0.684875796890799,0.164848531713828,
-4.87113686698358));
#70281=CARTESIAN_POINT('Ctrl Pts',(0.524213242357612,0.472819469636789,
-4.85525026848919));
#70282=CARTESIAN_POINT('Ctrl Pts',(0.23371275114266,0.664536143768718,-4.83936366999479));
#70283=CARTESIAN_POINT('Ctrl Pts',(-0.229947459772284,0.709508877214857,
-4.81818153866894));
#70284=CARTESIAN_POINT('Ctrl Pts',(-0.733033467760661,0.321156518088531,
-4.79170387451161));
#70285=CARTESIAN_POINT('Ctrl Pts',(-0.666201687207296,-0.444531828339013,
-4.75993067752283));
#70286=CARTESIAN_POINT('Ctrl Pts',(-0.101288996576348,-0.738917830377844,
-4.7334530133655));
#70287=CARTESIAN_POINT('Ctrl Pts',(0.345349925440383,-0.613160237413833,
-4.71227088203965));
#70288=CARTESIAN_POINT('Ctrl Pts',(0.685844918037705,-0.294589869160345,
-4.69108875071378));
#70289=CARTESIAN_POINT('Ctrl Pts',(0.715703969576795,0.211321562048467,
-4.66990661938793));
#70290=CARTESIAN_POINT('Ctrl Pts',(0.415290946306725,0.569002043485502,
-4.64872448806207));
#70291=CARTESIAN_POINT('Ctrl Pts',(0.0934696898535255,0.699729370120608,
-4.63283788956767));
#70292=CARTESIAN_POINT('Ctrl Pts',(-0.252055370210626,0.657797861633536,
-4.61695129107328));
#70293=CARTESIAN_POINT('Ctrl Pts',(-0.634566132837756,0.391924105099125,
-4.59576915974741));
#70294=CARTESIAN_POINT('Ctrl Pts',(-0.766612827327275,-0.229748442748258,
-4.56929149559011));
#70295=CARTESIAN_POINT('Ctrl Pts',(-0.220004051678502,-0.770085353509153,
-4.5375182986013));
#70296=CARTESIAN_POINT('Ctrl Pts',(0.401138704855467,-0.628766061699122,
-4.51104063444399));
#70297=CARTESIAN_POINT('Ctrl Pts',(0.660153306932357,-0.243781990912655,
-4.48985850311813));
#70298=CARTESIAN_POINT('Ctrl Pts',(0.713448163538854,0.21944967658462,-4.46867637179228));
#70299=CARTESIAN_POINT('Ctrl Pts',(0.408703467624615,0.624380052697233,
-4.44749424046641));
#70300=CARTESIAN_POINT('Ctrl Pts',(-0.0518139061167167,0.702527732340824,
-4.42631210914056));
#70301=CARTESIAN_POINT('Ctrl Pts',(-0.381729763931295,0.593835130031606,
-4.41042551064616));
#70302=CARTESIAN_POINT('Ctrl Pts',(-0.617941327913625,0.338198834530834,
-4.39453891215177));
#70303=CARTESIAN_POINT('Ctrl Pts',(-0.737373497855252,-0.11206696999172,
-4.37335678082591));
#70304=CARTESIAN_POINT('Ctrl Pts',(-0.435577045604655,-0.671380824354025,
-4.34687911666859));
#70305=CARTESIAN_POINT('Ctrl Pts',(0.33083155171032,-0.729372140157004,
-4.3151059196798));
#70306=CARTESIAN_POINT('Ctrl Pts',(0.712777470420673,-0.219561605337653,
-4.28862825552248));
#70307=CARTESIAN_POINT('Ctrl Pts',(0.660975650409514,0.241543448084987,
-4.26744612419662));
#70308=CARTESIAN_POINT('Ctrl Pts',(0.401722358340205,0.629114925446567,
-4.24626399287076));
#70309=CARTESIAN_POINT('Ctrl Pts',(-0.0926839103114625,0.74047192210371,
-4.2250818615449));
#70310=CARTESIAN_POINT('Ctrl Pts',(-0.494275113109166,0.50191832815303,
-4.20389973021904));
#70311=CARTESIAN_POINT('Ctrl Pts',(-0.675371530643,0.205501994948046,-4.18801313172465));
#70312=CARTESIAN_POINT('Ctrl Pts',(-0.689923040143449,-0.142253770076197,
-4.17212653323026));
#70313=CARTESIAN_POINT('Ctrl Pts',(-0.489472483728134,-0.562756935786156,
-4.1509444019044));
#70314=CARTESIAN_POINT('Ctrl Pts',(0.1026271793844,-0.793692154439977,-4.12446673774708));
#70315=CARTESIAN_POINT('Ctrl Pts',(0.72431759262137,-0.341756140344921,
-4.09269354075829));
#70316=CARTESIAN_POINT('Ctrl Pts',(0.685406179251917,0.294070383277605,
-4.06621587660097));
#70317=CARTESIAN_POINT('Ctrl Pts',(0.347425834209877,0.611986386671006,
-4.0450337452751));
#70318=CARTESIAN_POINT('Ctrl Pts',(-0.10106997904254,0.739561560619801,
-4.02385161394925));
#70319=CARTESIAN_POINT('Ctrl Pts',(-0.549989118149691,0.504381744883291,
-4.00266948262338));
#70320=CARTESIAN_POINT('Ctrl Pts',(-0.701649997804666,0.0625873482081273,
-3.98148735129754));
#70321=CARTESIAN_POINT('Ctrl Pts',(-0.647794192625342,-0.28057166345084,
-3.96560075280313));
#70322=CARTESIAN_POINT('Ctrl Pts',(-0.433764682453468,-0.555047868816476,
-3.94971415430875));
#70323=CARTESIAN_POINT('Ctrl Pts',(-0.00876936604903183,-0.745789366591879,
-3.92853202298289));
#70324=CARTESIAN_POINT('Ctrl Pts',(0.592020032873446,-0.538508917887617,
-3.90205435882556));
#70325=CARTESIAN_POINT('Ctrl Pts',(0.773304882718845,0.208405356954825,
-3.87028116183678));
#70326=CARTESIAN_POINT('Ctrl Pts',(0.332043120165925,0.667837096325308,
-3.84380349767945));
#70327=CARTESIAN_POINT('Ctrl Pts',(-0.13136609001657,0.691357359215059,
-3.82262136635359));
#70328=CARTESIAN_POINT('Ctrl Pts',(-0.555791578009408,0.498259133808778,
-3.80143923502774));
#70329=CARTESIAN_POINT('Ctrl Pts',(-0.745709399577484,0.0283983456625421,
-3.78025710370188));
#70330=CARTESIAN_POINT('Ctrl Pts',(-0.575307256124054,-0.40651132410552,
-3.75907497237602));
#70331=CARTESIAN_POINT('Ctrl Pts',(-0.312114038360918,-0.633200285366913,
-3.74318837388162));
#70332=CARTESIAN_POINT('Ctrl Pts',(0.0287001253000533,-0.703851006413595,
-3.72730177538723));
#70333=CARTESIAN_POINT('Ctrl Pts',(0.476104623192633,-0.574110676504985,
-3.70611964406137));
#70334=CARTESIAN_POINT('Ctrl Pts',(0.79983728491478,-0.0272009490298287,
-3.67964197990405));
#70335=CARTESIAN_POINT('Ctrl Pts',(0.454494167067824,0.659445438641893,
-3.64786878291526));
#70336=CARTESIAN_POINT('Ctrl Pts',(-0.179245745608589,0.723968219992404,
-3.62139111875794));
#70337=CARTESIAN_POINT('Ctrl Pts',(-0.547677888989984,0.441906073344255,
-3.60020898743208));
#70338=CARTESIAN_POINT('Ctrl Pts',(-0.746168494081024,0.0199755112803014,
-3.57902685610622));
#70339=CARTESIAN_POINT('Ctrl Pts',(-0.586756593893505,-0.461091828356436,
-3.55784472478036));
#70340=CARTESIAN_POINT('Ctrl Pts',(-0.175337816586413,-0.682265744156719,
-3.53666259345451));
#70341=CARTESIAN_POINT('Ctrl Pts',(0.172013285242014,-0.684667221379072,
-3.52077599496011));
#70342=CARTESIAN_POINT('Ctrl Pts',(0.477514626316864,-0.517889677513596,
-3.50488939646572));
#70343=CARTESIAN_POINT('Ctrl Pts',(0.734534508884567,-0.129374403805866,
-3.48370726513986));
#70344=CARTESIAN_POINT('Ctrl Pts',(0.627237233394482,0.497044290794701,
-3.45722960098254));
#70345=CARTESIAN_POINT('Ctrl Pts',(-0.0804823222740962,0.796841157474714,
-3.42545640399375));
#70346=CARTESIAN_POINT('Ctrl Pts',(-0.605282042510176,0.43576676088528,
-3.39897873983643));
#70347=CARTESIAN_POINT('Ctrl Pts',(-0.703504024592373,-0.0177238576331333,
-3.37779660851057));
#70348=CARTESIAN_POINT('Ctrl Pts',(-0.581653969262653,-0.467808831309393,
-3.35661447718471));
#70349=CARTESIAN_POINT('Ctrl Pts',(-0.148731575015875,-0.731278259794368,
-3.33543234585885));
#70350=CARTESIAN_POINT('Ctrl Pts',(0.308025509003036,-0.633522044903279,
-3.314250214533));
#70351=CARTESIAN_POINT('Ctrl Pts',(0.5743279309632,-0.410493851410992,-3.2983636160386));
#70352=CARTESIAN_POINT('Ctrl Pts',(0.699214400400128,-0.0856105057499347,
-3.2824770175442));
#70353=CARTESIAN_POINT('Ctrl Pts',(0.643606290730907,0.376894711602609,
-3.26129488621835));
#70354=CARTESIAN_POINT('Ctrl Pts',(0.156311633013567,0.784886136552685,
-3.23481722206102));
#70355=CARTESIAN_POINT('Ctrl Pts',(-0.577179940899014,0.555244585987189,
-3.20304402507224));
#70356=CARTESIAN_POINT('Ctrl Pts',(-0.743435082593453,-0.0596933735603376,
-3.17656636091491));
#70357=CARTESIAN_POINT('Ctrl Pts',(-0.524730724624935,-0.468923996380709,
-3.15538422958906));
#70358=CARTESIAN_POINT('Ctrl Pts',(-0.140494133246507,-0.733094701340396,
-3.1342020982632));
#70359=CARTESIAN_POINT('Ctrl Pts',(0.360032912737676,-0.653655319262541,
-3.11301996693734));
#70360=CARTESIAN_POINT('Ctrl Pts',(0.644886244911881,-0.283463625000574,
-3.09183783561148));
#70361=CARTESIAN_POINT('Ctrl Pts',(0.703481663861427,0.0589179339543426,
-3.07595123711709));
#70362=CARTESIAN_POINT('Ctrl Pts',(0.588354962968238,0.38738659498273,-3.06006463862269));
#70363=CARTESIAN_POINT('Ctrl Pts',(0.246567099391958,0.703905779632369,
-3.03888250729684));
#70364=CARTESIAN_POINT('Ctrl Pts',(-0.388958651052195,0.699421719522368,
-3.01240484313951));
#70365=CARTESIAN_POINT('Ctrl Pts',(-0.799360178391769,0.0495634910569404,
-2.98063164615074));
#70366=CARTESIAN_POINT('Ctrl Pts',(-0.527996742495623,-0.526762243134179,
-2.95415398199339));
#70367=CARTESIAN_POINT('Ctrl Pts',(-0.0963858541361063,-0.697095269579071,
-2.93297185066755));
#70368=CARTESIAN_POINT('Ctrl Pts',(0.367487293040394,-0.649707266439206,
-2.91178971934168));
#70369=CARTESIAN_POINT('Ctrl Pts',(0.697559134358486,-0.265141903002185,
-2.89060758801583));
#70370=CARTESIAN_POINT('Ctrl Pts',(0.675027237917631,0.201415301415524,
-2.86942545668997));
#70371=CARTESIAN_POINT('Ctrl Pts',(0.498046596364184,0.500307267767271,
-2.85353885819557));
#70372=CARTESIAN_POINT('Ctrl Pts',(0.197663098653,0.676135515893496,-2.83765225970118));
#70373=CARTESIAN_POINT('Ctrl Pts',(-0.267743933191193,0.696126330016126,
-2.81647012837532));
#70374=CARTESIAN_POINT('Ctrl Pts',(-0.749233056554967,0.281299486194467,
-2.78999246421801));
#70375=CARTESIAN_POINT('Ctrl Pts',(-0.641350032948401,-0.47969091056778,
-2.75821926722921));
#70376=CARTESIAN_POINT('Ctrl Pts',(-0.0614334537891717,-0.743293314670101,
-2.7317416030719));
#70377=CARTESIAN_POINT('Ctrl Pts',(0.377801898928307,-0.593715228803531,
-2.71055947174603));
#70378=CARTESIAN_POINT('Ctrl Pts',(0.70068501300572,-0.257307122247392,
-2.68937734042018));
#70379=CARTESIAN_POINT('Ctrl Pts',(0.703313419396356,0.249477872268438,
-2.66819520909431));
#70380=CARTESIAN_POINT('Ctrl Pts',(0.384112878137958,0.590497411021916,
-2.64701307776846));
#70381=CARTESIAN_POINT('Ctrl Pts',(0.0557314198619299,0.703741275733401,
-2.63112647927406));
#70382=CARTESIAN_POINT('Ctrl Pts',(-0.287040965920177,0.643301966657401,
-2.61523988077967));
#70383=CARTESIAN_POINT('Ctrl Pts',(-0.654711033413828,0.357256411878932,
-2.59405774945381));
#70384=CARTESIAN_POINT('Ctrl Pts',(-0.753158458967396,-0.270613949481221,
-2.56758008529649));
#70385=CARTESIAN_POINT('Ctrl Pts',(-0.178302031962507,-0.780795504496738,
-2.53580688830771));
#70386=CARTESIAN_POINT('Ctrl Pts',(0.434348713906479,-0.606300433453199,
-2.50932922415038));
#70387=CARTESIAN_POINT('Ctrl Pts',(0.672300129659377,-0.207953320259739,
-2.48814709282452));
#70388=CARTESIAN_POINT('Ctrl Pts',(0.70062407108951,0.257473015323963,-2.46696496149866));
#70389=CARTESIAN_POINT('Ctrl Pts',(0.374558924196536,0.645441389251823,
-2.44578283017281));
#70390=CARTESIAN_POINT('Ctrl Pts',(-0.0894926216029255,0.698728106099681,
-2.42460069884695));
#70391=CARTESIAN_POINT('Ctrl Pts',(-0.413090643562724,0.572463007129391,
-2.40871410035255));
#70392=CARTESIAN_POINT('Ctrl Pts',(-0.635223074932496,0.304502186354999,
-2.39282750185816));
#70393=CARTESIAN_POINT('Ctrl Pts',(-0.730285540866999,-0.151531217585722,
-2.3716453705323));
#70394=CARTESIAN_POINT('Ctrl Pts',(-0.398867864803067,-0.693818420334465,
-2.34516770637498));
#70395=CARTESIAN_POINT('Ctrl Pts',(0.369549690352763,-0.710539415377113,
-2.31339450938619));
#70396=CARTESIAN_POINT('Ctrl Pts',(0.723546655452461,-0.180939929980367,
-2.28691684522887));
#70397=CARTESIAN_POINT('Ctrl Pts',(0.647040070382234,0.276715006941831,
-2.26573471390301));
#70398=CARTESIAN_POINT('Ctrl Pts',(0.36733345238644,0.649794257721565,-2.24455258257715));
#70399=CARTESIAN_POINT('Ctrl Pts',(-0.132342674989519,0.734421126487522,
-2.22337045125129));
#70400=CARTESIAN_POINT('Ctrl Pts',(-0.520533786771069,0.474630880163505,
-2.20218831992543));
#70401=CARTESIAN_POINT('Ctrl Pts',(-0.685439209546698,0.168910817731426,
-2.18630172143104));
#70402=CARTESIAN_POINT('Ctrl Pts',(-0.681281422170332,-0.179124426662695,
-2.17041512293665));
#70403=CARTESIAN_POINT('Ctrl Pts',(-0.458522831705819,-0.588247816746384,
-2.14923299161079));
#70404=CARTESIAN_POINT('Ctrl Pts',(0.145131611989728,-0.787030106901402,
-2.12275532745347));
#70405=CARTESIAN_POINT('Ctrl Pts',(0.741636792304015,-0.302337729609267,
-2.09098213046468));
#70406=CARTESIAN_POINT('Ctrl Pts',(0.668612518062437,0.330478927570208,
-2.06450446630736));
#70407=CARTESIAN_POINT('Ctrl Pts',(0.314035869248326,0.629772594332678,
-2.0433223349815));
#70408=CARTESIAN_POINT('Ctrl Pts',(-0.14066770319757,0.733061416176826,
-2.02214020365564));
#70409=CARTESIAN_POINT('Ctrl Pts',(-0.57629966717217,0.474096686628197,
-2.00095807232978));
#70410=CARTESIAN_POINT('Ctrl Pts',(-0.703999522147564,0.0247904899309355,
-1.97977594100392));
#70411=CARTESIAN_POINT('Ctrl Pts',(-0.631780297798543,-0.314978459016283,
-1.96388934250953));
#70412=CARTESIAN_POINT('Ctrl Pts',(-0.403309811719612,-0.577556172326435,
-1.94800274401514));
#70413=CARTESIAN_POINT('Ctrl Pts',(0.0313217580437868,-0.745182949734803,
-1.92682061268927));
#70414=CARTESIAN_POINT('Ctrl Pts',(0.620103828443481,-0.505915819003228,
-1.90034294853195));
#70415=CARTESIAN_POINT('Ctrl Pts',(0.760987813965571,0.249661333490343,
-1.86856975154317));
#70416=CARTESIAN_POINT('Ctrl Pts',(0.295673986471208,0.684715937160779,
-1.84209208738584));
#70417=CARTESIAN_POINT('Ctrl Pts',(-0.168329559292972,0.683298768632944,
-1.82090995605999));
#70418=CARTESIAN_POINT('Ctrl Pts',(-0.581764715454044,0.467671100735052,
-1.79972782473413));
#70419=CARTESIAN_POINT('Ctrl Pts',(-0.746157952575386,-0.0117168452704052,
-1.77854569340826));
#70420=CARTESIAN_POINT('Ctrl Pts',(-0.552630154216026,-0.436840712647278,
-1.75736356208241));
#70421=CARTESIAN_POINT('Ctrl Pts',(-0.277635072315359,-0.649058195350113,
-1.74147696358801));
#70422=CARTESIAN_POINT('Ctrl Pts',(0.0664833528996994,-0.701291594280784,
-1.72559036509362));
#70423=CARTESIAN_POINT('Ctrl Pts',(0.506269144371473,-0.54769538482608,
-1.70440823376776));
#70424=CARTESIAN_POINT('Ctrl Pts',(0.800143274452744,0.0158213247235393,
-1.67793056961044));
#70425=CARTESIAN_POINT('Ctrl Pts',(0.418399054009061,0.682916880775836,
-1.64615737262165));
#70426=CARTESIAN_POINT('Ctrl Pts',(-0.217892523820332,0.713289470650559,
-1.61967970846433));
#70427=CARTESIAN_POINT('Ctrl Pts',(-0.570634357674029,0.411835498213804,
-1.59849757713847));
#70428=CARTESIAN_POINT('Ctrl Pts',(-0.746163743590037,-0.0201521800745495,
-1.57731544581261));
#70429=CARTESIAN_POINT('Ctrl Pts',(-0.561129810822313,-0.49195763035154,
-1.55613331448675));
#70430=CARTESIAN_POINT('Ctrl Pts',(-0.138419734612189,-0.690702448703422,
-1.5349511831609));
#70431=CARTESIAN_POINT('Ctrl Pts',(0.208558492969346,-0.674433932524933,
-1.5190645846665));
#70432=CARTESIAN_POINT('Ctrl Pts',(0.504655813759805,-0.491479853157888,
-1.50317798617211));
#70433=CARTESIAN_POINT('Ctrl Pts',(0.740425626835783,-0.0897138352053628,
-1.48199585484625));
#70434=CARTESIAN_POINT('Ctrl Pts',(0.599619882655918,0.530033555816679,
-1.45551819068893));
#70435=CARTESIAN_POINT('Ctrl Pts',(-0.123187980897615,0.79136461622102,
-1.42374499370014));
#70436=CARTESIAN_POINT('Ctrl Pts',(-0.627825347684238,0.402609430692957,
-1.39726732954282));
#70437=CARTESIAN_POINT('Ctrl Pts',(-0.701534974529444,-0.055504299464422,
-1.37608519821696));
#70438=CARTESIAN_POINT('Ctrl Pts',(-0.555673590256809,-0.498390713899415,
-1.3549030668911));
#70439=CARTESIAN_POINT('Ctrl Pts',(-0.109218024599217,-0.738214330501128,
-1.33372093556524));
#70440=CARTESIAN_POINT('Ctrl Pts',(0.341625653170807,-0.616053413812982,
-1.31253880423938));
#70441=CARTESIAN_POINT('Ctrl Pts',(0.595557808340173,-0.37903650385649,
-1.29665220574499));
#70442=CARTESIAN_POINT('Ctrl Pts',(0.702804700428006,-0.0479112667122281,
-1.2807656072506));
#70443=CARTESIAN_POINT('Ctrl Pts',(0.622422081552932,0.410937262240509,
-1.25958347592474));
#70444=CARTESIAN_POINT('Ctrl Pts',(0.113906261266067,0.792152092474895,
-1.23310581176742));
#70445=CARTESIAN_POINT('Ctrl Pts',(-0.606184549458043,0.523424804955423,
-1.20133261477863));
#70446=CARTESIAN_POINT('Ctrl Pts',(-0.739152904729264,-0.099559049352841,
-1.17485495062131));
#70447=CARTESIAN_POINT('Ctrl Pts',(-0.498772672191106,-0.496445232852937,
-1.15367281929545));
#70448=CARTESIAN_POINT('Ctrl Pts',(-0.100894871170555,-0.739585470098981,
-1.13249068796959));
#70449=CARTESIAN_POINT('Ctrl Pts',(0.394639860164164,-0.633362736055885,
-1.11130855664373));
#70450=CARTESIAN_POINT('Ctrl Pts',(0.659187605562879,-0.248398060071516,
-1.09012642531787));
#70451=CARTESIAN_POINT('Ctrl Pts',(0.699298891271897,0.0966376479255593,
-1.07423982682348));
#70452=CARTESIAN_POINT('Ctrl Pts',(0.566686762943658,0.418444798182639,
-1.05835322832909));
#70453=CARTESIAN_POINT('Ctrl Pts',(0.208383162066687,0.716139049954344,
-1.03717109700323));
#70454=CARTESIAN_POINT('Ctrl Pts',(-0.425983270133073,0.677508544252163,
-1.0106934328459));
#70455=CARTESIAN_POINT('Ctrl Pts',(-0.800868612319126,0.00653454254947985,
-0.978920235857118));
#70456=CARTESIAN_POINT('Ctrl Pts',(-0.498925764037445,-0.554375416894904,
-0.952442571699792));
#70457=CARTESIAN_POINT('Ctrl Pts',(-0.0587849258484244,-0.701267695135047,
-0.931260440373935));
#70458=CARTESIAN_POINT('Ctrl Pts',(0.401871301811429,-0.629019792526908,
-0.910078309048076));
#70459=CARTESIAN_POINT('Ctrl Pts',(0.710799778962247,-0.227272191175134,
-0.888896177722219));
#70460=CARTESIAN_POINT('Ctrl Pts',(0.663227825248934,0.237399973442935,
-0.867714046396359));
#70461=CARTESIAN_POINT('Ctrl Pts',(0.470440577277662,0.526349159381354,
-0.851827447901968));
#70462=CARTESIAN_POINT('Ctrl Pts',(0.16104219249472,0.685780831357495,-0.83594084940757));
#70463=CARTESIAN_POINT('Ctrl Pts',(-0.304766616737118,0.680731951966365,
-0.814758718081714));
#70464=CARTESIAN_POINT('Ctrl Pts',(-0.763267334089122,0.240629488373161,
-0.788281053924392));
#70465=CARTESIAN_POINT('Ctrl Pts',(-0.614644853367136,-0.513463668309351,
-0.756507856935603));
#70466=CARTESIAN_POINT('Ctrl Pts',(-0.0214003660392715,-0.745520653788183,
-0.730030192778282));
#70467=CARTESIAN_POINT('Ctrl Pts',(0.409162010937815,-0.572554361200174,
-0.708848061452424));
#70468=CARTESIAN_POINT('Ctrl Pts',(0.713500102386157,-0.219280748262106,
-0.687665930126567));
#70469=CARTESIAN_POINT('Ctrl Pts',(0.688890267353093,0.286913182271502,
-0.666483798800706));
#70470=CARTESIAN_POINT('Ctrl Pts',(0.351824709607146,0.610286219109459,
-0.64530166747485));
#70471=CARTESIAN_POINT('Ctrl Pts',(0.0178320838607445,0.70571934318682,
-0.629415068980454));
#70472=CARTESIAN_POINT('Ctrl Pts',(-0.321197002354292,0.626946904886804,
-0.613528470486061));
#70473=CARTESIAN_POINT('Ctrl Pts',(-0.672963795444224,0.321556235071336,
-0.592346339160204));
#70474=CARTESIAN_POINT('Ctrl Pts',(-0.737527433618484,-0.310697373257205,
-0.56586867500288));
#70475=CARTESIAN_POINT('Ctrl Pts',(-0.136084714826095,-0.789249125190363,
-0.534095478014092));
#70476=CARTESIAN_POINT('Ctrl Pts',(0.466303442539805,-0.582082578534946,
-0.50761781385677));
#70477=CARTESIAN_POINT('Ctrl Pts',(0.682503975557423,-0.171523651470232,
-0.486435682530911));
#70478=CARTESIAN_POINT('Ctrl Pts',(0.685775160935683,0.294752233755149,
-0.465253551205053));
#70479=CARTESIAN_POINT('Ctrl Pts',(0.339331867652397,0.664637404300089,
-0.444071419879196));
#70480=CARTESIAN_POINT('Ctrl Pts',(-0.126912670487204,0.692909095187001,
-0.422889288553336));
#70481=CARTESIAN_POINT('Ctrl Pts',(-0.443257737571659,0.549436516930662,
-0.407002690058943));
#70482=CARTESIAN_POINT('Ctrl Pts',(-0.650668891360673,0.269925384308696,
-0.391116091564549));
#70483=CARTESIAN_POINT('Ctrl Pts',(-0.721087274494807,-0.190557250697438,
-0.36993396023869));
#70484=CARTESIAN_POINT('Ctrl Pts',(-0.361005438736672,-0.714251442192837,
-0.343456296081368));
#70485=CARTESIAN_POINT('Ctrl Pts',(0.407198939161548,-0.689652180392618,
-0.311683099092581));
#70486=CARTESIAN_POINT('Ctrl Pts',(0.732226235701414,-0.141797050653159,
-0.285205434935257));
#70487=CARTESIAN_POINT('Ctrl Pts',(0.631232561002846,0.311089138051407,
-0.264023303609399));
#70488=CARTESIAN_POINT('Ctrl Pts',(0.331887985278457,0.668589766575936,
-0.242841172283542));
#70489=CARTESIAN_POINT('Ctrl Pts',(-0.17162922483904,0.726259811006413,
-0.221659040957683));
#70490=CARTESIAN_POINT('Ctrl Pts',(-0.545275419699615,0.445956922224332,
-0.200476909631823));
#70491=CARTESIAN_POINT('Ctrl Pts',(-0.69355232685328,0.131862298003188,
-0.184590311137431));
#70492=CARTESIAN_POINT('Ctrl Pts',(-0.670622753288826,-0.215533614975662,
-0.168703712643036));
#70493=CARTESIAN_POINT('Ctrl Pts',(-0.426352009365769,-0.611917192034414,
-0.147521581317179));
#70494=CARTESIAN_POINT('Ctrl Pts',(0.187431739085884,-0.778344785456901,
-0.121043917159855));
#70495=CARTESIAN_POINT('Ctrl Pts',(0.756436645482091,-0.261606416380455,
-0.0892707201710683));
#70496=CARTESIAN_POINT('Ctrl Pts',(0.650518462326474,0.365194457230119,
-0.0627930560137451));
#70497=CARTESIAN_POINT('Ctrl Pts',(0.278887226280858,0.64673161704124,-0.0416109246878868));
#70498=CARTESIAN_POINT('Ctrl Pts',(-0.0633939700665578,0.702956002425801,
-0.0257243261934916));
#70499=CARTESIAN_POINT('Ctrl Pts',(-0.392875925177587,0.585943088661304,
-0.00983772769910082));
#70500=CARTESIAN_POINT('Ctrl Pts',(-0.54753912821223,0.413276816066991,
0.000753337963830376));
#70501=CARTESIAN_POINT('Ctrl Pts',(-0.599695759644924,0.3135089884898,0.00604887079529526));
#70502=CARTESIAN_POINT('Origin',(0.,0.,-0.0599999999999996));
#70503=CARTESIAN_POINT('',(0.8511,-1.04229689075431E-16,0.));
#70504=CARTESIAN_POINT('Origin',(0.,0.,0.));
#70505=CARTESIAN_POINT('Origin',(0.8511,-1.04229689075431E-16,-0.0599999999999996));
#70506=CARTESIAN_POINT('Origin',(0.,0.,-0.0599999999999996));
#70507=CARTESIAN_POINT('Origin',(0.,0.,0.));
#70508=CARTESIAN_POINT('',(1.2,-0.692820323027552,0.));
#70509=CARTESIAN_POINT('',(1.2,0.692820323027551,0.));
#70510=CARTESIAN_POINT('',(1.2,-0.692820323027552,0.));
#70511=CARTESIAN_POINT('',(-2.54538057293978E-16,-1.3856406460551,0.));
#70512=CARTESIAN_POINT('',(-2.54538057293978E-16,-1.3856406460551,0.));
#70513=CARTESIAN_POINT('',(-1.2,-0.692820323027551,0.));
#70514=CARTESIAN_POINT('',(-1.2,-0.692820323027551,0.));
#70515=CARTESIAN_POINT('',(-1.2,0.692820323027551,0.));
#70516=CARTESIAN_POINT('',(-1.2,0.692820323027551,0.));
#70517=CARTESIAN_POINT('',(8.48460190979926E-17,1.3856406460551,0.));
#70518=CARTESIAN_POINT('',(8.48460190979926E-17,1.3856406460551,0.));
#70519=CARTESIAN_POINT('',(1.2,0.692820323027551,0.));
#70520=CARTESIAN_POINT('Origin',(0.,0.,-5.925));
#70521=CARTESIAN_POINT('Origin',(0.,0.,0.914655896708346));
#70522=CARTESIAN_POINT('',(1.2,-0.692820323027552,0.858179306876173));
#70523=CARTESIAN_POINT('',(-2.54538057293978E-16,-1.3856406460551,0.858179306876173));
#70524=CARTESIAN_POINT('Ctrl Pts',(1.2,-0.692820323027552,0.858179306876173));
#70525=CARTESIAN_POINT('Ctrl Pts',(0.599999999999999,-1.03923048454133,
1.05817930687617));
#70526=CARTESIAN_POINT('Ctrl Pts',(-2.54538057293978E-16,-1.3856406460551,
0.858179306876173));
#70527=CARTESIAN_POINT('',(1.2,0.692820323027551,0.858179306876173));
#70528=CARTESIAN_POINT('Ctrl Pts',(1.2,0.692820323027551,0.858179306876173));
#70529=CARTESIAN_POINT('Ctrl Pts',(1.2,-6.66133814775094E-16,1.05817930687617));
#70530=CARTESIAN_POINT('Ctrl Pts',(1.2,-0.692820323027552,0.858179306876173));
#70531=CARTESIAN_POINT('',(8.48460190979925E-17,1.3856406460551,0.858179306876173));
#70532=CARTESIAN_POINT('Ctrl Pts',(8.48460190979925E-17,1.3856406460551,
0.858179306876173));
#70533=CARTESIAN_POINT('Ctrl Pts',(0.6,1.03923048454133,1.05817930687617));
#70534=CARTESIAN_POINT('Ctrl Pts',(1.2,0.692820323027551,0.858179306876173));
#70535=CARTESIAN_POINT('',(-1.2,0.692820323027551,0.858179306876173));
#70536=CARTESIAN_POINT('Ctrl Pts',(-1.2,0.692820323027551,0.858179306876173));
#70537=CARTESIAN_POINT('Ctrl Pts',(-0.600000000000001,1.03923048454133,
1.05817930687617));
#70538=CARTESIAN_POINT('Ctrl Pts',(8.48460190979925E-17,1.3856406460551,
0.858179306876173));
#70539=CARTESIAN_POINT('',(-1.2,-1.11389921653139E-16,0.965358983848622));
#70540=CARTESIAN_POINT('Ctrl Pts',(-1.2,-7.58222274085957E-17,0.965358983848622));
#70541=CARTESIAN_POINT('Ctrl Pts',(-1.2,0.321539030917347,0.965358983848622));
#70542=CARTESIAN_POINT('Ctrl Pts',(-1.2,0.692820323027551,0.858179306876173));
#70543=CARTESIAN_POINT('',(-1.14,-1.39609735102798E-16,1.));
#70544=CARTESIAN_POINT('',(-1.28782032302755,-1.5771250364726E-16,0.914655896708346));
#70545=CARTESIAN_POINT('Origin',(0.,0.,1.));
#70546=CARTESIAN_POINT('',(-1.2,-0.692820323027551,0.858179306876173));
#70547=CARTESIAN_POINT('Ctrl Pts',(-1.2,-0.692820323027551,0.858179306876173));
#70548=CARTESIAN_POINT('Ctrl Pts',(-1.2,-0.321539030917347,0.965358983848622));
#70549=CARTESIAN_POINT('Ctrl Pts',(-1.2,-7.58222274085957E-17,0.965358983848622));
#70550=CARTESIAN_POINT('Ctrl Pts',(-2.54538057293978E-16,-1.3856406460551,
0.858179306876173));
#70551=CARTESIAN_POINT('Ctrl Pts',(-0.599999999999999,-1.03923048454133,
1.05817930687617));
#70552=CARTESIAN_POINT('Ctrl Pts',(-1.2,-0.692820323027551,0.858179306876173));
#70553=CARTESIAN_POINT('Origin',(8.48460190979926E-17,1.3856406460551,0.));
#70554=CARTESIAN_POINT('',(8.48460190979926E-17,1.3856406460551,0.));
#70555=CARTESIAN_POINT('',(-1.2,0.692820323027551,0.));
#70556=CARTESIAN_POINT('Origin',(1.2,0.692820323027551,0.));
#70557=CARTESIAN_POINT('',(1.2,0.692820323027551,0.));
#70558=CARTESIAN_POINT('Origin',(1.2,-0.692820323027552,0.));
#70559=CARTESIAN_POINT('',(1.2,-0.692820323027552,0.));
#70560=CARTESIAN_POINT('Origin',(-2.54538057293978E-16,-1.3856406460551,
0.));
#70561=CARTESIAN_POINT('',(-2.54538057293978E-16,-1.3856406460551,0.));
#70562=CARTESIAN_POINT('Origin',(-1.2,-0.692820323027551,0.));
#70563=CARTESIAN_POINT('',(-1.2,-0.692820323027551,0.));
#70564=CARTESIAN_POINT('Origin',(-1.2,0.692820323027551,0.));
#70565=CARTESIAN_POINT('Origin',(0.,0.,1.));
#70566=CARTESIAN_POINT('Origin',(0.7,0.,-12.));
#70567=CARTESIAN_POINT('',(-0.7,-8.57252759403147E-17,-12.));
#70568=CARTESIAN_POINT('Origin',(0.,0.,-12.));
#70569=CARTESIAN_POINT('Origin',(0.,0.,-11.95));
#70570=CARTESIAN_POINT('',(-0.75,-9.18485099360515E-17,-11.95));
#70571=CARTESIAN_POINT('',(0.,0.,0.));
#70572=CARTESIAN_POINT('Origin',(0.,0.,0.04));
#70573=CARTESIAN_POINT('',(-0.805,-9.85840673313619E-17,0.08));
#70574=CARTESIAN_POINT('Origin',(0.,0.,0.08));
#70575=CARTESIAN_POINT('',(-0.885,1.08381241724541E-16,0.));
#70576=CARTESIAN_POINT('',(-0.845,-1.03482654527951E-16,0.04));
#70577=CARTESIAN_POINT('Origin',(0.,0.,0.));
#70578=CARTESIAN_POINT('Origin',(0.,0.,0.));
#70579=CARTESIAN_POINT('',(-0.805,9.85840673313619E-17,1.4));
#70580=CARTESIAN_POINT('Origin',(0.,0.,1.4));
#70581=CARTESIAN_POINT('',(-0.805,-9.85840673313619E-17,0.));
#70582=CARTESIAN_POINT('Origin',(0.,0.,0.));
#70583=CARTESIAN_POINT('',(-1.14,-1.39609735102798E-16,-8.32667268468867E-17));
#70584=CARTESIAN_POINT('Origin',(0.,0.,0.));
#70585=CARTESIAN_POINT('Origin',(0.,0.,1.44));
#70586=CARTESIAN_POINT('',(-0.885,-1.08381241724541E-16,1.48));
#70587=CARTESIAN_POINT('Origin',(0.,0.,1.48));
#70588=CARTESIAN_POINT('',(-0.845,-1.03482654527951E-16,1.44));
#70589=CARTESIAN_POINT('Origin',(0.,0.,1.48));
#70590=CARTESIAN_POINT('',(-1.14,-1.39609735102798E-16,1.48));
#70591=CARTESIAN_POINT('Origin',(0.,0.,1.48));
#70592=CARTESIAN_POINT('Origin',(0.,0.,0.085344103291654));
#70593=CARTESIAN_POINT('',(-1.2,-1.36663997456004E-16,0.0346410161513778));
#70594=CARTESIAN_POINT('',(-1.28782032302755,-1.5771250364726E-16,0.085344103291654));
#70595=CARTESIAN_POINT('',(-1.2,0.692820323027551,0.141820693123827));
#70596=CARTESIAN_POINT('Ctrl Pts',(-1.2,0.692820323027551,0.141820693123827));
#70597=CARTESIAN_POINT('Ctrl Pts',(-1.2,0.321539030917347,0.0346410161513777));
#70598=CARTESIAN_POINT('Ctrl Pts',(-1.2,-1.26370379014326E-16,0.0346410161513778));
#70599=CARTESIAN_POINT('',(8.48460190979925E-17,1.3856406460551,0.141820693123827));
#70600=CARTESIAN_POINT('Ctrl Pts',(8.48460190979925E-17,1.3856406460551,
0.141820693123827));
#70601=CARTESIAN_POINT('Ctrl Pts',(-0.599999999999999,1.03923048454133,
-0.0581793068761738));
#70602=CARTESIAN_POINT('Ctrl Pts',(-1.2,0.692820323027551,0.141820693123827));
#70603=CARTESIAN_POINT('',(1.2,0.692820323027551,0.141820693123827));
#70604=CARTESIAN_POINT('Ctrl Pts',(1.2,0.692820323027551,0.141820693123827));
#70605=CARTESIAN_POINT('Ctrl Pts',(0.6,1.03923048454133,-0.0581793068761734));
#70606=CARTESIAN_POINT('Ctrl Pts',(8.48460190979925E-17,1.3856406460551,
0.141820693123827));
#70607=CARTESIAN_POINT('',(1.2,-0.692820323027552,0.141820693123827));
#70608=CARTESIAN_POINT('Ctrl Pts',(1.2,-0.692820323027552,0.141820693123827));
#70609=CARTESIAN_POINT('Ctrl Pts',(1.2,-9.99200722162641E-16,-0.0581793068761738));
#70610=CARTESIAN_POINT('Ctrl Pts',(1.2,0.692820323027551,0.141820693123827));
#70611=CARTESIAN_POINT('',(-2.54538057293978E-16,-1.3856406460551,0.141820693123827));
#70612=CARTESIAN_POINT('Ctrl Pts',(-2.54538057293978E-16,-1.3856406460551,
0.141820693123827));
#70613=CARTESIAN_POINT('Ctrl Pts',(0.6,-1.03923048454133,-0.0581793068761735));
#70614=CARTESIAN_POINT('Ctrl Pts',(1.2,-0.692820323027551,0.141820693123827));
#70615=CARTESIAN_POINT('',(-1.2,-0.692820323027551,0.141820693123827));
#70616=CARTESIAN_POINT('Ctrl Pts',(-1.2,-0.692820323027551,0.141820693123827));
#70617=CARTESIAN_POINT('Ctrl Pts',(-0.6,-1.03923048454133,-0.0581793068761732));
#70618=CARTESIAN_POINT('Ctrl Pts',(-2.54538057293978E-16,-1.3856406460551,
0.141820693123827));
#70619=CARTESIAN_POINT('Ctrl Pts',(-1.2,-1.26370379014326E-16,0.0346410161513778));
#70620=CARTESIAN_POINT('Ctrl Pts',(-1.2,-0.321539030917348,0.0346410161513778));
#70621=CARTESIAN_POINT('Ctrl Pts',(-1.2,-0.692820323027551,0.141820693123827));
#70622=CARTESIAN_POINT('Origin',(-2.54538057293978E-16,-1.3856406460551,
0.));
#70623=CARTESIAN_POINT('',(1.2,-0.692820323027552,1.33817930687617));
#70624=CARTESIAN_POINT('',(1.2,-0.692820323027552,0.));
#70625=CARTESIAN_POINT('',(-2.54538057293978E-16,-1.3856406460551,1.33817930687617));
#70626=CARTESIAN_POINT('Ctrl Pts',(1.2,-0.692820323027552,1.33817930687617));
#70627=CARTESIAN_POINT('Ctrl Pts',(0.6,-1.03923048454133,1.53817930687617));
#70628=CARTESIAN_POINT('Ctrl Pts',(-2.54538057293978E-16,-1.3856406460551,
1.33817930687617));
#70629=CARTESIAN_POINT('',(-2.54538057293978E-16,-1.3856406460551,0.));
#70630=CARTESIAN_POINT('Origin',(1.2,-0.692820323027552,0.));
#70631=CARTESIAN_POINT('',(1.2,0.692820323027551,1.33817930687617));
#70632=CARTESIAN_POINT('',(1.2,0.692820323027551,0.));
#70633=CARTESIAN_POINT('Ctrl Pts',(1.2,0.692820323027551,1.33817930687617));
#70634=CARTESIAN_POINT('Ctrl Pts',(1.2,0.,1.53817930687617));
#70635=CARTESIAN_POINT('Ctrl Pts',(1.2,-0.692820323027552,1.33817930687617));
#70636=CARTESIAN_POINT('Origin',(1.2,0.692820323027551,0.));
#70637=CARTESIAN_POINT('',(8.48460190979925E-17,1.3856406460551,1.33817930687617));
#70638=CARTESIAN_POINT('',(8.48460190979926E-17,1.3856406460551,0.));
#70639=CARTESIAN_POINT('Ctrl Pts',(8.48460190979925E-17,1.3856406460551,
1.33817930687617));
#70640=CARTESIAN_POINT('Ctrl Pts',(0.6,1.03923048454133,1.53817930687617));
#70641=CARTESIAN_POINT('Ctrl Pts',(1.2,0.692820323027551,1.33817930687617));
#70642=CARTESIAN_POINT('Origin',(0.,0.,1.39465589670835));
#70643=CARTESIAN_POINT('',(-1.2,0.692820323027551,1.33817930687617));
#70644=CARTESIAN_POINT('Ctrl Pts',(-1.2,0.692820323027551,1.33817930687617));
#70645=CARTESIAN_POINT('Ctrl Pts',(-0.6,1.03923048454133,1.53817930687617));
#70646=CARTESIAN_POINT('Ctrl Pts',(8.48460190979925E-17,1.3856406460551,
1.33817930687617));
#70647=CARTESIAN_POINT('',(-1.2,-1.36663997456004E-16,1.44535898384862));
#70648=CARTESIAN_POINT('Ctrl Pts',(-1.2,-1.26370379014326E-16,1.44535898384862));
#70649=CARTESIAN_POINT('Ctrl Pts',(-1.2,0.321539030917347,1.44535898384862));
#70650=CARTESIAN_POINT('Ctrl Pts',(-1.2,0.692820323027551,1.33817930687617));
#70651=CARTESIAN_POINT('',(-1.28782032302755,-1.5771250364726E-16,1.39465589670835));
#70652=CARTESIAN_POINT('',(-1.2,-0.692820323027551,1.33817930687617));
#70653=CARTESIAN_POINT('Ctrl Pts',(-1.2,-0.692820323027551,1.33817930687617));
#70654=CARTESIAN_POINT('Ctrl Pts',(-1.2,-0.321539030917348,1.44535898384862));
#70655=CARTESIAN_POINT('Ctrl Pts',(-1.2,-1.26370379014326E-16,1.44535898384862));
#70656=CARTESIAN_POINT('Ctrl Pts',(-2.54538057293978E-16,-1.3856406460551,
1.33817930687617));
#70657=CARTESIAN_POINT('Ctrl Pts',(-0.6,-1.03923048454133,1.53817930687617));
#70658=CARTESIAN_POINT('Ctrl Pts',(-1.2,-0.692820323027551,1.33817930687617));
#70659=CARTESIAN_POINT('Origin',(8.48460190979926E-17,1.3856406460551,0.));
#70660=CARTESIAN_POINT('',(-1.2,0.692820323027551,0.));
#70661=CARTESIAN_POINT('Origin',(-1.2,-0.692820323027551,0.));
#70662=CARTESIAN_POINT('',(-1.2,-0.692820323027551,0.));
#70663=CARTESIAN_POINT('Origin',(-1.2,0.692820323027551,0.));
#70664=CARTESIAN_POINT('',(0.,0.,0.));
#70665=CARTESIAN_POINT('Origin',(0.,0.,0.13));
#70666=CARTESIAN_POINT('',(-0.85,-1.04094977927525E-16,0.26));
#70667=CARTESIAN_POINT('Origin',(0.,0.,0.26));
#70668=CARTESIAN_POINT('',(-0.85,-1.04094977927525E-16,0.));
#70669=CARTESIAN_POINT('',(-0.85,-1.04094977927525E-16,0.13));
#70670=CARTESIAN_POINT('Origin',(0.,0.,0.));
#70671=CARTESIAN_POINT('Origin',(1.5,0.,0.));
#70672=CARTESIAN_POINT('',(-1.5,-1.83697019872103E-16,0.));
#70673=CARTESIAN_POINT('Origin',(0.,0.,0.));
#70674=CARTESIAN_POINT('Origin',(0.,0.,0.13));
#70675=CARTESIAN_POINT('',(-1.5,-1.83697019872103E-16,0.26));
#70676=CARTESIAN_POINT('Origin',(0.,0.,0.26));
#70677=CARTESIAN_POINT('',(-1.5,-1.83697019872103E-16,0.13));
#70678=CARTESIAN_POINT('Origin',(0.,0.,0.28));
#70679=CARTESIAN_POINT('',(-1.46,-1.78798432675514E-16,0.3));
#70680=CARTESIAN_POINT('Origin',(0.,0.,0.3));
#70681=CARTESIAN_POINT('',(-1.48,-1.81247726273808E-16,0.28));
#70682=CARTESIAN_POINT('Origin',(0.89,0.,0.3));
#70683=CARTESIAN_POINT('',(-0.89,-1.08993565124114E-16,0.3));
#70684=CARTESIAN_POINT('Origin',(0.,0.,0.3));
#70685=CARTESIAN_POINT('Origin',(0.,0.,0.28));
#70686=CARTESIAN_POINT('',(-0.87,-1.0654427152582E-16,0.28));
#70687=CARTESIAN_POINT('',(0.,0.,0.));
#70688=CARTESIAN_POINT('Origin',(-24.3512401121419,-7.2,116.813364586238));
#70689=CARTESIAN_POINT('',(-24.7247837315525,-7.2,117.848601353551));
#70690=CARTESIAN_POINT('Origin',(-24.3848650377401,-7.2,116.802439185627));
#70691=CARTESIAN_POINT('',(-24.7102863810161,-7.2,118.0328076576));
#70692=CARTESIAN_POINT('',(-24.7175350562843,-7.2,117.940704505576));
#70693=CARTESIAN_POINT('',(-23.9249439920713,-7.2,115.615772316099));
#70694=CARTESIAN_POINT('Origin',(-24.3176151865437,-7.2,116.824289986849));
#70695=CARTESIAN_POINT('Origin',(-24.3176151865437,-7.2,116.824289986849));
#70696=CARTESIAN_POINT('Origin',(-24.2897593861105,-7.2,116.833340885064));
#70697=CARTESIAN_POINT('',(-23.8511305947749,-7.2,115.578162511662));
#70698=CARTESIAN_POINT('',(-23.8880372934231,-7.2,115.596967413881));
#70699=CARTESIAN_POINT('',(-24.6726765765799,-7.2,118.106621054896));
#70700=CARTESIAN_POINT('Origin',(-24.2619035856774,-7.2,116.842391783279));
#70701=CARTESIAN_POINT('Origin',(-24.2619035856774,-7.2,116.842391783279));
#70702=CARTESIAN_POINT('Origin',(-24.3848650377401,-7.2,116.802439185627));
#70703=CARTESIAN_POINT('Origin',(-24.1807258342645,-7.2,116.868768033609));
#70704=CARTESIAN_POINT('',(-24.5321718749764,-7.2,118.226623406752));
#70705=CARTESIAN_POINT('',(-24.6024242257782,-7.2,118.166622230824));
#70706=CARTESIAN_POINT('',(-23.6669242907266,-7.2,115.563665161126));
#70707=CARTESIAN_POINT('Origin',(-24.0995480828515,-7.2,116.895144283939));
#70708=CARTESIAN_POINT('Origin',(-24.0995480828515,-7.2,116.895144283939));
#70709=CARTESIAN_POINT('Origin',(-22.8631746116678,-7.2,117.296866376627));
#70710=CARTESIAN_POINT('',(-23.381607335838,-7.2,115.656370259438));
#70711=CARTESIAN_POINT('',(-22.4305508195429,-7.2,115.965387253813));
#70712=CARTESIAN_POINT('Origin',(-23.814231127963,-7.2,116.987849382252));
#70713=CARTESIAN_POINT('Origin',(7.,-6.45,127.));
#70714=CARTESIAN_POINT('',(6.38,-6.4,127.));
#70715=CARTESIAN_POINT('Origin',(7.,-6.4,127.));
#70716=CARTESIAN_POINT('',(6.48,-6.5,127.));
#70717=CARTESIAN_POINT('',(6.43,-6.45,127.));
#70718=CARTESIAN_POINT('Origin',(7.,-6.5,127.));
#70719=CARTESIAN_POINT('Origin',(7.,-8.1,127.));
#70720=CARTESIAN_POINT('',(6.48,-7.9,127.));
#70721=CARTESIAN_POINT('Origin',(7.,-7.9,127.));
#70722=CARTESIAN_POINT('',(6.48,-8.1,127.));
#70723=CARTESIAN_POINT('Origin',(5.51247677078473,-6.4,126.411332101473));
#70724=CARTESIAN_POINT('',(4.48674914492698,-6.4,125.02678684895));
#70725=CARTESIAN_POINT('',(3.8069117573021,-6.4,127.1191111848));
#70726=CARTESIAN_POINT('',(3.93054736833321,-6.4,126.738599900121));
#70727=CARTESIAN_POINT('',(6.66008130618755,-6.4,128.046162167925));
#70728=CARTESIAN_POINT('',(3.99872699598973,-6.4,127.181435733887));
#70729=CARTESIAN_POINT('',(7.33991869381246,-6.4,125.953837832075));
#70730=CARTESIAN_POINT('Origin',(7.00000000000001,-6.4,127.));
#70731=CARTESIAN_POINT('',(6.58067741620492,-6.4,125.707145386788));
#70732=CARTESIAN_POINT('Origin',(7.,-7.95,127.));
#70733=CARTESIAN_POINT('',(6.38,-8.,127.));
#70734=CARTESIAN_POINT('Origin',(7.,-8.,127.));
#70735=CARTESIAN_POINT('',(6.43,-7.95,127.));
#70736=CARTESIAN_POINT('Origin',(5.51247677078473,-8.,126.411332101473));
#70737=CARTESIAN_POINT('',(3.8069117573021,-8.,127.1191111848));
#70738=CARTESIAN_POINT('',(4.48674914492698,-8.,125.02678684895));
#70739=CARTESIAN_POINT('',(3.93054736833321,-8.,126.738599900121));
#70740=CARTESIAN_POINT('',(7.33991869381247,-8.,125.953837832075));
#70741=CARTESIAN_POINT('',(6.58067741620492,-8.,125.707145386788));
#70742=CARTESIAN_POINT('',(6.66008130618756,-8.,128.046162167925));
#70743=CARTESIAN_POINT('Origin',(7.00000000000001,-8.,127.));
#70744=CARTESIAN_POINT('',(3.99872699598973,-8.,127.181435733887));
#70745=CARTESIAN_POINT('Origin',(-21.5792483146694,-7.2,117.714039319033));
#70746=CARTESIAN_POINT('',(-22.059424932609,-7.2,119.030067592127));
#70747=CARTESIAN_POINT('',(-21.1941773483592,-7.2,116.367109346501));
#70748=CARTESIAN_POINT('Origin',(-21.6268011404841,-7.2,117.698588469314));
#70749=CARTESIAN_POINT('Origin',(-21.6268011404841,-7.2,117.698588469314));
#70750=CARTESIAN_POINT('',(-21.933417581542,-7.2,118.965863639935));
#70751=CARTESIAN_POINT('',(-21.9964212570755,-7.2,118.997965616031));
#70752=CARTESIAN_POINT('Origin',(-21.5316954888546,-7.2,117.729490168752));
#70753=CARTESIAN_POINT('Origin',(-22.8631746116678,-7.2,117.296866376627));
#70754=CARTESIAN_POINT('',(-21.6697056065068,-7.2,116.212600849313));
#70755=CARTESIAN_POINT('Origin',(-22.1023293986317,-7.2,117.544079972127));
#70756=CARTESIAN_POINT('',(-22.4305508195429,-7.2,115.965387253813));
#70757=CARTESIAN_POINT('Origin',(-21.9643192809795,-7.2,119.060969291565));
#70758=CARTESIAN_POINT('',(-21.2226784944797,-7.2,116.778433652456));
#70759=CARTESIAN_POINT('Origin',(-21.5316954888546,-7.2,117.729490168752));
#70760=CARTESIAN_POINT('Origin',(-24.2159532206504,-7.2,118.224222853435));
#70761=CARTESIAN_POINT('',(-23.4125090352755,-7.2,115.751475911068));
#70762=CARTESIAN_POINT('Origin',(-23.814231127963,-7.2,116.987849382252));
#70763=CARTESIAN_POINT('Origin',(-23.7191254763334,-7.2,117.018751081689));
#70764=CARTESIAN_POINT('',(-23.2222977320165,-7.2,115.813279309943));
#70765=CARTESIAN_POINT('Origin',(-23.6240198247039,-7.2,117.049652781127));
#70766=CARTESIAN_POINT('',(-23.317403383646,-7.2,115.782377610505));
#70767=CARTESIAN_POINT('Origin',(-24.0720944665476,-7.2,118.428684729755));
#70768=CARTESIAN_POINT('',(-23.191396032579,-7.2,115.718173658313));
#70769=CARTESIAN_POINT('Origin',(-23.6240198247039,-7.2,117.049652781127));
#70770=CARTESIAN_POINT('Origin',(-22.8631746116678,-7.2,117.296866376627));
#70771=CARTESIAN_POINT('',(-22.6207621228019,-7.2,115.903583854938));
#70772=CARTESIAN_POINT('',(-22.4305508195429,-7.2,115.965387253813));
#70773=CARTESIAN_POINT('Origin',(-23.0533859149268,-7.2,117.235062977752));
#70774=CARTESIAN_POINT('Origin',(-23.4551080076143,-7.2,118.471436448935));
#70775=CARTESIAN_POINT('',(-22.6516638222394,-7.2,115.998689506568));
#70776=CARTESIAN_POINT('Origin',(-23.0533859149268,-7.2,117.235062977752));
#70777=CARTESIAN_POINT('Origin',(-22.9582802632973,-7.2,117.265964677189));
#70778=CARTESIAN_POINT('',(-22.4614525189804,-7.2,116.060492905443));
#70779=CARTESIAN_POINT('Origin',(-22.8631746116678,-7.2,117.296866376627));
#70780=CARTESIAN_POINT('',(-22.5565581706099,-7.2,116.029591206005));
#70781=CARTESIAN_POINT('Origin',(-23.3112492535115,-7.2,118.675898325255));
#70782=CARTESIAN_POINT('',(-22.4305508195429,-7.2,115.965387253813));
#70783=CARTESIAN_POINT('Origin',(-22.8631746116678,-7.2,117.296866376627));
#70784=CARTESIAN_POINT('Origin',(-22.8631746116678,-7.2,117.296866376627));
#70785=CARTESIAN_POINT('',(-21.8599169097658,-7.2,116.150797450438));
#70786=CARTESIAN_POINT('',(-22.4305508195429,-7.2,115.965387253813));
#70787=CARTESIAN_POINT('Origin',(-22.2925407018907,-7.2,117.482276573252));
#70788=CARTESIAN_POINT('Origin',(-22.6942627945782,-7.2,118.718650044435));
#70789=CARTESIAN_POINT('',(-21.8908186092033,-7.2,116.245903102068));
#70790=CARTESIAN_POINT('Origin',(-22.2925407018907,-7.2,117.482276573252));
#70791=CARTESIAN_POINT('Origin',(-22.1974350502612,-7.2,117.513178272689));
#70792=CARTESIAN_POINT('',(-21.7006073059442,-7.2,116.307706500943));
#70793=CARTESIAN_POINT('Origin',(-22.1023293986317,-7.2,117.544079972127));
#70794=CARTESIAN_POINT('',(-21.7957129575738,-7.2,116.276804801505));
#70795=CARTESIAN_POINT('Origin',(-22.5504040404754,-7.2,118.923111920755));
#70796=CARTESIAN_POINT('Origin',(3.68330495955212,-7.2,127.499533791318));
#70797=CARTESIAN_POINT('',(4.61035594267696,-7.2,124.646364242432));
#70798=CARTESIAN_POINT('Origin',(4.14683045111454,-7.2,126.072949016875));
#70799=CARTESIAN_POINT('',(4.51765084436447,-7.9,124.931681197321));
#70800=CARTESIAN_POINT('',(4.35541692231764,-8.42499999999998,125.430985868376));
#70801=CARTESIAN_POINT('',(3.7760100578646,-7.9,127.214216836429));
#70802=CARTESIAN_POINT('',(3.70648123413024,-7.67499999999999,127.428204552596));
#70803=CARTESIAN_POINT('',(3.7760100578646,-6.5,127.214216836429));
#70804=CARTESIAN_POINT('',(3.77601005786461,-7.6,127.214216836429));
#70805=CARTESIAN_POINT('',(3.70648123413024,-6.72500000000001,127.428204552596));
#70806=CARTESIAN_POINT('',(4.51765084436447,-6.5,124.931681197321));
#70807=CARTESIAN_POINT('',(4.35541692231764,-5.97500000000002,125.430985868376));
#70808=CARTESIAN_POINT('',(4.51765084436447,-7.6,124.931681197321));
#70809=CARTESIAN_POINT('Origin',(4.09927762529978,-7.2,126.057498167156));
#70810=CARTESIAN_POINT('',(4.54615199048493,-7.2,124.520356891365));
#70811=CARTESIAN_POINT('Origin',(4.05172479948503,-7.2,126.042047317438));
#70812=CARTESIAN_POINT('',(4.57825396658095,-7.2,124.583360566899));
#70813=CARTESIAN_POINT('Origin',(0.342604385933935,-7.2,124.836881039375));
#70814=CARTESIAN_POINT('',(-2.87208883661725,-7.2,122.110024335241));
#70815=CARTESIAN_POINT('Origin',(-3.36651602761717,-7.2,123.631714761313));
#70816=CARTESIAN_POINT('',(0.837031576933849,-7.2,123.315190613303));
#70817=CARTESIAN_POINT('Origin',(-3.41406885343193,-7.2,123.616263911594));
#70818=CARTESIAN_POINT('',(-2.99809618768428,-7.2,122.174228287433));
#70819=CARTESIAN_POINT('Origin',(-3.46162167924668,-7.2,123.600813061876));
#70820=CARTESIAN_POINT('',(-2.93509251215077,-7.2,122.142126311337));
#70821=CARTESIAN_POINT('Origin',(-3.77063867362164,-7.2,124.551869578171));
#70822=CARTESIAN_POINT('',(-3.15260468487175,-7.2,122.64975654558));
#70823=CARTESIAN_POINT('Origin',(-3.46162167924669,-7.2,123.600813061876));
#70824=CARTESIAN_POINT('Origin',(-12.4966585840506,-7.2,120.665151615314));
#70825=CARTESIAN_POINT('',(-12.1876415896757,-7.2,119.714095099018));
#70826=CARTESIAN_POINT('Origin',(3.98327614627098,-6.45,127.228988559702));
#70827=CARTESIAN_POINT('',(6.62917960675006,-6.5,128.141267819554));
#70828=CARTESIAN_POINT('',(3.96782529655224,-6.5,127.276541385517));
#70829=CARTESIAN_POINT('',(6.62917960675006,-6.5,128.141267819554));
#70830=CARTESIAN_POINT('Origin',(2.82495354156945,-8.,126.905199842054));
#70831=CARTESIAN_POINT('',(6.62917960675006,-7.9,128.141267819554));
#70832=CARTESIAN_POINT('',(3.96782529655224,-7.9,127.276541385517));
#70833=CARTESIAN_POINT('',(6.62917960675006,-8.,128.141267819554));
#70834=CARTESIAN_POINT('Origin',(3.98327614627098,-7.95,127.228988559702));
#70835=CARTESIAN_POINT('',(6.62917960675006,-7.9,128.141267819554));
#70836=CARTESIAN_POINT('Origin',(7.00000000000001,-6.45,127.));
#70837=CARTESIAN_POINT('',(7.37082039324996,-6.5,125.858732180446));
#70838=CARTESIAN_POINT('',(7.37082039324996,-6.5,125.858732180446));
#70839=CARTESIAN_POINT('Origin',(7.00000000000001,-6.5,127.));
#70840=CARTESIAN_POINT('Origin',(6.59612826592367,-6.45,125.659592560973));
#70841=CARTESIAN_POINT('',(6.61157911564241,-6.5,125.612039735158));
#70842=CARTESIAN_POINT('Origin',(7.00000000000001,-8.,127.));
#70843=CARTESIAN_POINT('',(7.37082039324996,-7.9,125.858732180446));
#70844=CARTESIAN_POINT('Origin',(7.00000000000001,-7.9,127.));
#70845=CARTESIAN_POINT('',(7.37082039324996,-8.,125.858732180446));
#70846=CARTESIAN_POINT('Origin',(6.59612826592367,-7.95,125.659592560973));
#70847=CARTESIAN_POINT('',(6.61157911564241,-7.9,125.612039735158));
#70848=CARTESIAN_POINT('',(7.37082039324996,-7.9,125.858732180446));
#70849=CARTESIAN_POINT('Origin',(7.00000000000001,-7.95,127.));
#70850=CARTESIAN_POINT('Origin',(7.37082039324994,-8.,125.858732180446));
#70851=CARTESIAN_POINT('',(0.,0.,0.));
#70852=CARTESIAN_POINT('Origin',(30.,3.55,17.));
#70853=CARTESIAN_POINT('',(29.025,3.5,17.));
#70854=CARTESIAN_POINT('Origin',(30.,3.5,17.));
#70855=CARTESIAN_POINT('',(29.125,3.6,17.));
#70856=CARTESIAN_POINT('',(29.075,3.55,17.));
#70857=CARTESIAN_POINT('Origin',(30.,3.6,17.));
#70858=CARTESIAN_POINT('Origin',(26.5,3.5,1.));
#70859=CARTESIAN_POINT('',(33.2,3.5,1.1));
#70860=CARTESIAN_POINT('',(26.8,3.5,1.1));
#70861=CARTESIAN_POINT('',(28.25,3.5,1.1));
#70862=CARTESIAN_POINT('',(33.2,3.5,144.9));
#70863=CARTESIAN_POINT('',(33.2,3.5,1.));
#70864=CARTESIAN_POINT('',(26.8,3.5,144.9));
#70865=CARTESIAN_POINT('',(28.25,3.5,144.9));
#70866=CARTESIAN_POINT('',(26.8,3.5,1.));
#70867=CARTESIAN_POINT('',(29.025,3.5,6.));
#70868=CARTESIAN_POINT('Origin',(30.,3.5,6.));
#70869=CARTESIAN_POINT('',(29.025,3.5,137.5));
#70870=CARTESIAN_POINT('Origin',(30.,3.5,137.5));
#70871=CARTESIAN_POINT('',(28.6,3.5,83.75));
#70872=CARTESIAN_POINT('Origin',(30.,3.5,83.75));
#70873=CARTESIAN_POINT('',(28.6,3.5,74.75));
#70874=CARTESIAN_POINT('Origin',(30.,3.5,74.75));
#70875=CARTESIAN_POINT('',(28.6,3.5,56.75));
#70876=CARTESIAN_POINT('Origin',(30.,3.5,56.75));
#70877=CARTESIAN_POINT('',(28.6,3.5,38.75));
#70878=CARTESIAN_POINT('Origin',(30.,3.5,38.75));
#70879=CARTESIAN_POINT('',(28.6,3.5,65.75));
#70880=CARTESIAN_POINT('Origin',(30.,3.5,65.75));
#70881=CARTESIAN_POINT('',(28.6,3.5,47.75));
#70882=CARTESIAN_POINT('Origin',(30.,3.5,47.75));
#70883=CARTESIAN_POINT('',(29.025,3.5,33.5));
#70884=CARTESIAN_POINT('Origin',(30.,3.5,33.5));
#70885=CARTESIAN_POINT('',(29.025,3.5,142.5));
#70886=CARTESIAN_POINT('Origin',(30.,3.5,142.5));
#70887=CARTESIAN_POINT('Origin',(30.,0.,17.));
#70888=CARTESIAN_POINT('',(29.125,3.9,17.));
#70889=CARTESIAN_POINT('',(29.125,0.,17.));
#70890=CARTESIAN_POINT('Origin',(30.,3.9,17.));
#70891=CARTESIAN_POINT('Origin',(30.,3.55,6.));
#70892=CARTESIAN_POINT('',(29.125,3.6,6.));
#70893=CARTESIAN_POINT('',(29.075,3.55,6.));
#70894=CARTESIAN_POINT('Origin',(30.,3.6,6.));
#70895=CARTESIAN_POINT('Origin',(30.,0.,6.));
#70896=CARTESIAN_POINT('',(29.125,3.9,6.));
#70897=CARTESIAN_POINT('',(29.125,0.,6.));
#70898=CARTESIAN_POINT('Origin',(30.,3.9,6.));
#70899=CARTESIAN_POINT('Origin',(30.,3.55,142.5));
#70900=CARTESIAN_POINT('',(29.125,3.6,142.5));
#70901=CARTESIAN_POINT('',(29.075,3.55,142.5));
#70902=CARTESIAN_POINT('Origin',(30.,3.6,142.5));
#70903=CARTESIAN_POINT('Origin',(30.,0.,142.5));
#70904=CARTESIAN_POINT('',(29.125,3.9,142.5));
#70905=CARTESIAN_POINT('',(29.125,0.,142.5));
#70906=CARTESIAN_POINT('Origin',(30.,3.9,142.5));
#70907=CARTESIAN_POINT('Origin',(30.,3.55,137.5));
#70908=CARTESIAN_POINT('',(29.125,3.6,137.5));
#70909=CARTESIAN_POINT('',(29.075,3.55,137.5));
#70910=CARTESIAN_POINT('Origin',(30.,3.6,137.5));
#70911=CARTESIAN_POINT('Origin',(30.,0.,137.5));
#70912=CARTESIAN_POINT('',(29.125,3.9,137.5));
#70913=CARTESIAN_POINT('',(29.125,0.,137.5));
#70914=CARTESIAN_POINT('Origin',(30.,3.9,137.5));
#70915=CARTESIAN_POINT('Origin',(30.,3.55,33.5));
#70916=CARTESIAN_POINT('',(29.125,3.6,33.5));
#70917=CARTESIAN_POINT('',(29.075,3.55,33.5));
#70918=CARTESIAN_POINT('Origin',(30.,3.6,33.5));
#70919=CARTESIAN_POINT('Origin',(30.,0.,33.5));
#70920=CARTESIAN_POINT('',(29.125,3.9,33.5));
#70921=CARTESIAN_POINT('',(29.125,0.,33.5));
#70922=CARTESIAN_POINT('Origin',(30.,3.9,33.5));
#70923=CARTESIAN_POINT('Origin',(30.,3.55,83.75));
#70924=CARTESIAN_POINT('',(28.7,3.6,83.75));
#70925=CARTESIAN_POINT('',(28.65,3.55,83.75));
#70926=CARTESIAN_POINT('Origin',(30.,3.6,83.75));
#70927=CARTESIAN_POINT('Origin',(30.,0.,83.75));
#70928=CARTESIAN_POINT('',(28.7,3.9,83.75));
#70929=CARTESIAN_POINT('',(28.7,0.,83.75));
#70930=CARTESIAN_POINT('Origin',(30.,3.9,83.75));
#70931=CARTESIAN_POINT('Origin',(30.,3.55,47.75));
#70932=CARTESIAN_POINT('',(28.7,3.6,47.75));
#70933=CARTESIAN_POINT('',(28.65,3.55,47.75));
#70934=CARTESIAN_POINT('Origin',(30.,3.6,47.75));
#70935=CARTESIAN_POINT('Origin',(30.,0.,47.75));
#70936=CARTESIAN_POINT('',(28.7,3.9,47.75));
#70937=CARTESIAN_POINT('',(28.7,0.,47.75));
#70938=CARTESIAN_POINT('Origin',(30.,3.9,47.75));
#70939=CARTESIAN_POINT('Origin',(30.,-3.55,17.));
#70940=CARTESIAN_POINT('',(29.025,-3.5,17.));
#70941=CARTESIAN_POINT('Origin',(30.,-3.5,17.));
#70942=CARTESIAN_POINT('',(29.125,-3.6,17.));
#70943=CARTESIAN_POINT('',(29.075,-3.55,17.));
#70944=CARTESIAN_POINT('Origin',(30.,-3.6,17.));
#70945=CARTESIAN_POINT('Origin',(33.5,-3.5,1.));
#70946=CARTESIAN_POINT('',(26.8,-3.5,1.1));
#70947=CARTESIAN_POINT('',(33.2,-3.5,1.1));
#70948=CARTESIAN_POINT('',(31.75,-3.5,1.1));
#70949=CARTESIAN_POINT('',(26.8,-3.5,144.9));
#70950=CARTESIAN_POINT('',(26.8,-3.5,1.));
#70951=CARTESIAN_POINT('',(33.2,-3.5,144.9));
#70952=CARTESIAN_POINT('',(31.75,-3.5,144.9));
#70953=CARTESIAN_POINT('',(33.2,-3.5,1.));
#70954=CARTESIAN_POINT('',(29.025,-3.5,6.));
#70955=CARTESIAN_POINT('Origin',(30.,-3.5,6.));
#70956=CARTESIAN_POINT('',(29.025,-3.5,137.5));
#70957=CARTESIAN_POINT('Origin',(30.,-3.5,137.5));
#70958=CARTESIAN_POINT('',(28.6,-3.5,47.75));
#70959=CARTESIAN_POINT('Origin',(30.,-3.5,47.75));
#70960=CARTESIAN_POINT('',(28.6,-3.5,65.75));
#70961=CARTESIAN_POINT('Origin',(30.,-3.5,65.75));
#70962=CARTESIAN_POINT('',(28.6,-3.5,38.75));
#70963=CARTESIAN_POINT('Origin',(30.,-3.5,38.75));
#70964=CARTESIAN_POINT('',(28.6,-3.5,56.75));
#70965=CARTESIAN_POINT('Origin',(30.,-3.5,56.75));
#70966=CARTESIAN_POINT('',(28.6,-3.5,74.75));
#70967=CARTESIAN_POINT('Origin',(30.,-3.5,74.75));
#70968=CARTESIAN_POINT('',(28.6,-3.5,83.75));
#70969=CARTESIAN_POINT('Origin',(30.,-3.5,83.75));
#70970=CARTESIAN_POINT('',(29.025,-3.5,33.5));
#70971=CARTESIAN_POINT('Origin',(30.,-3.5,33.5));
#70972=CARTESIAN_POINT('',(29.025,-3.5,142.5));
#70973=CARTESIAN_POINT('Origin',(30.,-3.5,142.5));
#70974=CARTESIAN_POINT('Origin',(30.,0.,17.));
#70975=CARTESIAN_POINT('',(29.125,-3.9,17.));
#70976=CARTESIAN_POINT('Origin',(30.,-3.9,17.));
#70977=CARTESIAN_POINT('',(29.125,0.,17.));
#70978=CARTESIAN_POINT('Origin',(30.,-3.55,6.));
#70979=CARTESIAN_POINT('',(29.125,-3.6,6.));
#70980=CARTESIAN_POINT('',(29.075,-3.55,6.));
#70981=CARTESIAN_POINT('Origin',(30.,-3.6,6.));
#70982=CARTESIAN_POINT('Origin',(30.,0.,6.));
#70983=CARTESIAN_POINT('',(29.125,-3.9,6.));
#70984=CARTESIAN_POINT('Origin',(30.,-3.9,6.));
#70985=CARTESIAN_POINT('',(29.125,0.,6.));
#70986=CARTESIAN_POINT('Origin',(30.,-3.55,142.5));
#70987=CARTESIAN_POINT('',(29.125,-3.6,142.5));
#70988=CARTESIAN_POINT('',(29.075,-3.55,142.5));
#70989=CARTESIAN_POINT('Origin',(30.,-3.6,142.5));
#70990=CARTESIAN_POINT('Origin',(30.,0.,142.5));
#70991=CARTESIAN_POINT('',(29.125,-3.9,142.5));
#70992=CARTESIAN_POINT('Origin',(30.,-3.9,142.5));
#70993=CARTESIAN_POINT('',(29.125,0.,142.5));
#70994=CARTESIAN_POINT('Origin',(30.,-3.55,137.5));
#70995=CARTESIAN_POINT('',(29.125,-3.6,137.5));
#70996=CARTESIAN_POINT('',(29.075,-3.55,137.5));
#70997=CARTESIAN_POINT('Origin',(30.,-3.6,137.5));
#70998=CARTESIAN_POINT('Origin',(30.,0.,137.5));
#70999=CARTESIAN_POINT('',(29.125,-3.9,137.5));
#71000=CARTESIAN_POINT('Origin',(30.,-3.9,137.5));
#71001=CARTESIAN_POINT('',(29.125,0.,137.5));
#71002=CARTESIAN_POINT('Origin',(30.,-3.55,33.5));
#71003=CARTESIAN_POINT('',(29.125,-3.6,33.5));
#71004=CARTESIAN_POINT('',(29.075,-3.55,33.5));
#71005=CARTESIAN_POINT('Origin',(30.,-3.6,33.5));
#71006=CARTESIAN_POINT('Origin',(30.,0.,33.5));
#71007=CARTESIAN_POINT('',(29.125,-3.9,33.5));
#71008=CARTESIAN_POINT('Origin',(30.,-3.9,33.5));
#71009=CARTESIAN_POINT('',(29.125,0.,33.5));
#71010=CARTESIAN_POINT('Origin',(31.75,-3.55,1.05));
#71011=CARTESIAN_POINT('',(26.8,-3.6,1.));
#71012=CARTESIAN_POINT('',(26.8,-3.6,1.));
#71013=CARTESIAN_POINT('',(33.2,-3.6,1.));
#71014=CARTESIAN_POINT('',(33.2,-3.5,1.1));
#71015=CARTESIAN_POINT('',(31.75,-3.6,1.));
#71016=CARTESIAN_POINT('Origin',(26.8,-3.2,1.05));
#71017=CARTESIAN_POINT('',(26.4,-3.2,1.));
#71018=CARTESIAN_POINT('',(26.5,-3.2,1.1));
#71019=CARTESIAN_POINT('',(26.4,-3.2,1.));
#71020=CARTESIAN_POINT('Origin',(26.8,-3.2,1.1));
#71021=CARTESIAN_POINT('Origin',(26.8,-3.2,1.));
#71022=CARTESIAN_POINT('Origin',(26.45,-1.75,1.05));
#71023=CARTESIAN_POINT('',(26.4,3.2,1.));
#71024=CARTESIAN_POINT('',(26.5,3.2,1.1));
#71025=CARTESIAN_POINT('',(26.4,3.2,1.));
#71026=CARTESIAN_POINT('',(26.5,-1.75,1.1));
#71027=CARTESIAN_POINT('',(26.4,-1.75,1.));
#71028=CARTESIAN_POINT('Origin',(26.8,3.2,1.05));
#71029=CARTESIAN_POINT('',(26.8,3.6,1.));
#71030=CARTESIAN_POINT('',(26.8,3.6,1.));
#71031=CARTESIAN_POINT('Origin',(26.8,3.2,1.1));
#71032=CARTESIAN_POINT('Origin',(26.8,3.2,1.));
#71033=CARTESIAN_POINT('Origin',(28.25,3.55,1.05));
#71034=CARTESIAN_POINT('',(33.2,3.6,1.));
#71035=CARTESIAN_POINT('',(33.2,3.6,1.));
#71036=CARTESIAN_POINT('',(28.25,3.6,1.));
#71037=CARTESIAN_POINT('Origin',(33.2,3.2,1.05));
#71038=CARTESIAN_POINT('',(33.6,3.2,1.));
#71039=CARTESIAN_POINT('',(33.5,3.2,1.1));
#71040=CARTESIAN_POINT('',(33.6,3.2,1.));
#71041=CARTESIAN_POINT('Origin',(33.2,3.2,1.1));
#71042=CARTESIAN_POINT('Origin',(33.2,3.2,1.));
#71043=CARTESIAN_POINT('Origin',(33.55,1.75,1.05));
#71044=CARTESIAN_POINT('',(33.6,-3.2,1.));
#71045=CARTESIAN_POINT('',(33.5,-3.2,1.1));
#71046=CARTESIAN_POINT('',(33.6,-3.2,1.));
#71047=CARTESIAN_POINT('',(33.5,1.75,1.1));
#71048=CARTESIAN_POINT('',(33.6,1.75,1.));
#71049=CARTESIAN_POINT('Origin',(33.2,-3.2,1.05));
#71050=CARTESIAN_POINT('Origin',(33.2,-3.2,1.1));
#71051=CARTESIAN_POINT('Origin',(33.2,-3.2,1.));
#71052=CARTESIAN_POINT('Origin',(33.2,3.2,1.));
#71053=CARTESIAN_POINT('',(33.5,3.2,144.9));
#71054=CARTESIAN_POINT('',(33.5,3.2,1.));
#71055=CARTESIAN_POINT('Origin',(33.2,3.2,144.9));
#71056=CARTESIAN_POINT('Origin',(33.5,3.5,1.));
#71057=CARTESIAN_POINT('',(33.5,-3.2,144.9));
#71058=CARTESIAN_POINT('',(33.5,-3.2,1.));
#71059=CARTESIAN_POINT('',(33.5,1.75,144.9));
#71060=CARTESIAN_POINT('Origin',(33.2,-3.2,1.));
#71061=CARTESIAN_POINT('Origin',(33.2,-3.2,144.9));
#71062=CARTESIAN_POINT('Origin',(30.,0.,1.));
#71063=CARTESIAN_POINT('',(33.2,3.9,1.));
#71064=CARTESIAN_POINT('',(26.8,3.9,1.));
#71065=CARTESIAN_POINT('',(32.,3.9,1.));
#71066=CARTESIAN_POINT('',(33.9,3.2,1.));
#71067=CARTESIAN_POINT('Origin',(33.2,3.2,1.));
#71068=CARTESIAN_POINT('',(33.9,-3.2,1.));
#71069=CARTESIAN_POINT('',(33.9,-2.,1.));
#71070=CARTESIAN_POINT('',(33.2,-3.9,1.));
#71071=CARTESIAN_POINT('Origin',(33.2,-3.2,1.));
#71072=CARTESIAN_POINT('',(26.8,-3.9,1.));
#71073=CARTESIAN_POINT('',(28.,-3.9,1.));
#71074=CARTESIAN_POINT('',(26.1,-3.2,1.));
#71075=CARTESIAN_POINT('Origin',(26.8,-3.2,1.));
#71076=CARTESIAN_POINT('',(26.1,3.2,1.));
#71077=CARTESIAN_POINT('',(26.1,2.,1.));
#71078=CARTESIAN_POINT('Origin',(26.8,3.2,1.));
#71079=CARTESIAN_POINT('Origin',(30.,-3.55,83.75));
#71080=CARTESIAN_POINT('',(28.7,-3.6,83.75));
#71081=CARTESIAN_POINT('',(28.65,-3.55,83.75));
#71082=CARTESIAN_POINT('Origin',(30.,-3.6,83.75));
#71083=CARTESIAN_POINT('Origin',(30.,0.,83.75));
#71084=CARTESIAN_POINT('',(28.7,-3.9,83.75));
#71085=CARTESIAN_POINT('Origin',(30.,-3.9,83.75));
#71086=CARTESIAN_POINT('',(28.7,0.,83.75));
#71087=CARTESIAN_POINT('Origin',(30.,-3.55,47.75));
#71088=CARTESIAN_POINT('',(28.7,-3.6,47.75));
#71089=CARTESIAN_POINT('',(28.65,-3.55,47.75));
#71090=CARTESIAN_POINT('Origin',(30.,-3.6,47.75));
#71091=CARTESIAN_POINT('Origin',(30.,0.,47.75));
#71092=CARTESIAN_POINT('',(28.7,-3.9,47.75));
#71093=CARTESIAN_POINT('Origin',(30.,-3.9,47.75));
#71094=CARTESIAN_POINT('',(28.7,0.,47.75));
#71095=CARTESIAN_POINT('Origin',(30.,-3.55,74.75));
#71096=CARTESIAN_POINT('',(28.7,-3.6,74.75));
#71097=CARTESIAN_POINT('',(28.65,-3.55,74.75));
#71098=CARTESIAN_POINT('Origin',(30.,-3.6,74.75));
#71099=CARTESIAN_POINT('Origin',(30.,0.,74.75));
#71100=CARTESIAN_POINT('',(28.7,-3.9,74.75));
#71101=CARTESIAN_POINT('Origin',(30.,-3.9,74.75));
#71102=CARTESIAN_POINT('',(28.7,0.,74.75));
#71103=CARTESIAN_POINT('Origin',(30.,3.55,74.75));
#71104=CARTESIAN_POINT('',(28.7,3.6,74.75));
#71105=CARTESIAN_POINT('',(28.65,3.55,74.75));
#71106=CARTESIAN_POINT('Origin',(30.,3.6,74.75));
#71107=CARTESIAN_POINT('Origin',(30.,0.,74.75));
#71108=CARTESIAN_POINT('',(28.7,3.9,74.75));
#71109=CARTESIAN_POINT('',(28.7,0.,74.75));
#71110=CARTESIAN_POINT('Origin',(30.,3.9,74.75));
#71111=CARTESIAN_POINT('Origin',(30.,-3.55,65.75));
#71112=CARTESIAN_POINT('',(28.7,-3.6,65.75));
#71113=CARTESIAN_POINT('',(28.65,-3.55,65.75));
#71114=CARTESIAN_POINT('Origin',(30.,-3.6,65.75));
#71115=CARTESIAN_POINT('Origin',(30.,0.,65.75));
#71116=CARTESIAN_POINT('',(28.7,-3.9,65.75));
#71117=CARTESIAN_POINT('Origin',(30.,-3.9,65.75));
#71118=CARTESIAN_POINT('',(28.7,0.,65.75));
#71119=CARTESIAN_POINT('Origin',(30.,3.55,65.75));
#71120=CARTESIAN_POINT('',(28.7,3.6,65.75));
#71121=CARTESIAN_POINT('',(28.65,3.55,65.75));
#71122=CARTESIAN_POINT('Origin',(30.,3.6,65.75));
#71123=CARTESIAN_POINT('Origin',(30.,0.,65.75));
#71124=CARTESIAN_POINT('',(28.7,3.9,65.75));
#71125=CARTESIAN_POINT('',(28.7,0.,65.75));
#71126=CARTESIAN_POINT('Origin',(30.,3.9,65.75));
#71127=CARTESIAN_POINT('Origin',(30.,-3.55,56.75));
#71128=CARTESIAN_POINT('',(28.7,-3.6,56.75));
#71129=CARTESIAN_POINT('',(28.65,-3.55,56.75));
#71130=CARTESIAN_POINT('Origin',(30.,-3.6,56.75));
#71131=CARTESIAN_POINT('Origin',(30.,0.,56.75));
#71132=CARTESIAN_POINT('',(28.7,-3.9,56.75));
#71133=CARTESIAN_POINT('Origin',(30.,-3.9,56.75));
#71134=CARTESIAN_POINT('',(28.7,0.,56.75));
#71135=CARTESIAN_POINT('Origin',(30.,3.55,56.75));
#71136=CARTESIAN_POINT('',(28.7,3.6,56.75));
#71137=CARTESIAN_POINT('',(28.65,3.55,56.75));
#71138=CARTESIAN_POINT('Origin',(30.,3.6,56.75));
#71139=CARTESIAN_POINT('Origin',(30.,0.,56.75));
#71140=CARTESIAN_POINT('',(28.7,3.9,56.75));
#71141=CARTESIAN_POINT('',(28.7,0.,56.75));
#71142=CARTESIAN_POINT('Origin',(30.,3.9,56.75));
#71143=CARTESIAN_POINT('Origin',(30.,-3.55,38.75));
#71144=CARTESIAN_POINT('',(28.7,-3.6,38.75));
#71145=CARTESIAN_POINT('',(28.65,-3.55,38.75));
#71146=CARTESIAN_POINT('Origin',(30.,-3.6,38.75));
#71147=CARTESIAN_POINT('Origin',(30.,0.,38.75));
#71148=CARTESIAN_POINT('',(28.7,-3.9,38.75));
#71149=CARTESIAN_POINT('Origin',(30.,-3.9,38.75));
#71150=CARTESIAN_POINT('',(28.7,0.,38.75));
#71151=CARTESIAN_POINT('Origin',(30.,-3.95,17.));
#71152=CARTESIAN_POINT('',(29.025,-4.,17.));
#71153=CARTESIAN_POINT('Origin',(30.,-4.,17.));
#71154=CARTESIAN_POINT('',(29.075,-3.95,17.));
#71155=CARTESIAN_POINT('Origin',(26.,-4.,1.));
#71156=CARTESIAN_POINT('',(33.2,-4.,1.1));
#71157=CARTESIAN_POINT('',(26.8,-4.,1.1));
#71158=CARTESIAN_POINT('',(28.,-4.,1.1));
#71159=CARTESIAN_POINT('',(33.2,-4.,144.9));
#71160=CARTESIAN_POINT('',(33.2,-4.,1.));
#71161=CARTESIAN_POINT('',(26.8,-4.,144.9));
#71162=CARTESIAN_POINT('',(28.,-4.,144.9));
#71163=CARTESIAN_POINT('',(26.8,-4.,1.));
#71164=CARTESIAN_POINT('',(29.025,-4.,6.));
#71165=CARTESIAN_POINT('Origin',(30.,-4.,6.));
#71166=CARTESIAN_POINT('',(29.025,-4.,137.5));
#71167=CARTESIAN_POINT('Origin',(30.,-4.,137.5));
#71168=CARTESIAN_POINT('',(28.6,-4.,38.75));
#71169=CARTESIAN_POINT('Origin',(30.,-4.,38.75));
#71170=CARTESIAN_POINT('',(28.6,-4.,65.75));
#71171=CARTESIAN_POINT('Origin',(30.,-4.,65.75));
#71172=CARTESIAN_POINT('',(28.6,-4.,83.75));
#71173=CARTESIAN_POINT('Origin',(30.,-4.,83.75));
#71174=CARTESIAN_POINT('',(28.6,-4.,47.75));
#71175=CARTESIAN_POINT('Origin',(30.,-4.,47.75));
#71176=CARTESIAN_POINT('',(28.6,-4.,74.75));
#71177=CARTESIAN_POINT('Origin',(30.,-4.,74.75));
#71178=CARTESIAN_POINT('',(28.6,-4.,56.75));
#71179=CARTESIAN_POINT('Origin',(30.,-4.,56.75));
#71180=CARTESIAN_POINT('',(29.025,-4.,33.5));
#71181=CARTESIAN_POINT('Origin',(30.,-4.,33.5));
#71182=CARTESIAN_POINT('',(29.025,-4.,142.5));
#71183=CARTESIAN_POINT('Origin',(30.,-4.,142.5));
#71184=CARTESIAN_POINT('Origin',(30.,-3.95,6.));
#71185=CARTESIAN_POINT('',(29.075,-3.95,6.));
#71186=CARTESIAN_POINT('Origin',(30.,-3.95,142.5));
#71187=CARTESIAN_POINT('',(29.075,-3.95,142.5));
#71188=CARTESIAN_POINT('Origin',(30.,-3.95,137.5));
#71189=CARTESIAN_POINT('',(29.075,-3.95,137.5));
#71190=CARTESIAN_POINT('Origin',(30.,-3.95,33.5));
#71191=CARTESIAN_POINT('',(29.075,-3.95,33.5));
#71192=CARTESIAN_POINT('Origin',(30.,3.55,38.75));
#71193=CARTESIAN_POINT('',(28.7,3.6,38.75));
#71194=CARTESIAN_POINT('',(28.65,3.55,38.75));
#71195=CARTESIAN_POINT('Origin',(30.,3.6,38.75));
#71196=CARTESIAN_POINT('Origin',(30.,0.,38.75));
#71197=CARTESIAN_POINT('',(28.7,3.9,38.75));
#71198=CARTESIAN_POINT('',(28.7,0.,38.75));
#71199=CARTESIAN_POINT('Origin',(30.,3.9,38.75));
#71200=CARTESIAN_POINT('Origin',(30.,3.95,17.));
#71201=CARTESIAN_POINT('',(29.025,4.,17.));
#71202=CARTESIAN_POINT('Origin',(30.,4.,17.));
#71203=CARTESIAN_POINT('',(29.075,3.95,17.));
#71204=CARTESIAN_POINT('Origin',(34.,4.,1.));
#71205=CARTESIAN_POINT('',(26.8,4.,1.1));
#71206=CARTESIAN_POINT('',(33.2,4.,1.1));
#71207=CARTESIAN_POINT('',(32.,4.,1.1));
#71208=CARTESIAN_POINT('',(26.8,4.,144.9));
#71209=CARTESIAN_POINT('',(26.8,4.,1.));
#71210=CARTESIAN_POINT('',(33.2,4.,144.9));
#71211=CARTESIAN_POINT('',(32.,4.,144.9));
#71212=CARTESIAN_POINT('',(33.2,4.,1.));
#71213=CARTESIAN_POINT('',(29.025,4.,6.));
#71214=CARTESIAN_POINT('Origin',(30.,4.,6.));
#71215=CARTESIAN_POINT('',(29.025,4.,137.5));
#71216=CARTESIAN_POINT('Origin',(30.,4.,137.5));
#71217=CARTESIAN_POINT('',(28.6,4.,56.75));
#71218=CARTESIAN_POINT('Origin',(30.,4.,56.75));
#71219=CARTESIAN_POINT('',(28.6,4.,74.75));
#71220=CARTESIAN_POINT('Origin',(30.,4.,74.75));
#71221=CARTESIAN_POINT('',(28.6,4.,47.75));
#71222=CARTESIAN_POINT('Origin',(30.,4.,47.75));
#71223=CARTESIAN_POINT('',(28.6,4.,83.75));
#71224=CARTESIAN_POINT('Origin',(30.,4.,83.75));
#71225=CARTESIAN_POINT('',(28.6,4.,65.75));
#71226=CARTESIAN_POINT('Origin',(30.,4.,65.75));
#71227=CARTESIAN_POINT('',(28.6,4.,38.75));
#71228=CARTESIAN_POINT('Origin',(30.,4.,38.75));
#71229=CARTESIAN_POINT('',(29.025,4.,33.5));
#71230=CARTESIAN_POINT('Origin',(30.,4.,33.5));
#71231=CARTESIAN_POINT('',(29.025,4.,142.5));
#71232=CARTESIAN_POINT('Origin',(30.,4.,142.5));
#71233=CARTESIAN_POINT('Origin',(30.,3.95,6.));
#71234=CARTESIAN_POINT('',(29.075,3.95,6.));
#71235=CARTESIAN_POINT('Origin',(30.,3.95,142.5));
#71236=CARTESIAN_POINT('',(29.075,3.95,142.5));
#71237=CARTESIAN_POINT('Origin',(30.,3.95,137.5));
#71238=CARTESIAN_POINT('',(29.075,3.95,137.5));
#71239=CARTESIAN_POINT('Origin',(30.,3.95,33.5));
#71240=CARTESIAN_POINT('',(29.075,3.95,33.5));
#71241=CARTESIAN_POINT('Origin',(32.,3.95,1.05));
#71242=CARTESIAN_POINT('',(26.8,3.9,1.));
#71243=CARTESIAN_POINT('',(33.2,4.,1.1));
#71244=CARTESIAN_POINT('Origin',(26.8,3.2,1.05));
#71245=CARTESIAN_POINT('',(26.,3.2,1.1));
#71246=CARTESIAN_POINT('',(26.1,3.2,1.));
#71247=CARTESIAN_POINT('Origin',(26.8,3.2,1.1));
#71248=CARTESIAN_POINT('Origin',(26.05,2.,1.05));
#71249=CARTESIAN_POINT('',(26.,-3.2,1.1));
#71250=CARTESIAN_POINT('',(26.1,-3.2,1.));
#71251=CARTESIAN_POINT('',(26.,2.,1.1));
#71252=CARTESIAN_POINT('Origin',(26.8,-3.2,1.05));
#71253=CARTESIAN_POINT('',(26.8,-3.9,1.));
#71254=CARTESIAN_POINT('Origin',(26.8,-3.2,1.1));
#71255=CARTESIAN_POINT('Origin',(28.,-3.95,1.05));
#71256=CARTESIAN_POINT('',(33.2,-3.9,1.));
#71257=CARTESIAN_POINT('Origin',(33.2,-3.2,1.05));
#71258=CARTESIAN_POINT('',(34.,-3.2,1.1));
#71259=CARTESIAN_POINT('',(33.9,-3.2,1.));
#71260=CARTESIAN_POINT('Origin',(33.2,-3.2,1.1));
#71261=CARTESIAN_POINT('Origin',(33.95,-2.,1.05));
#71262=CARTESIAN_POINT('',(34.,3.2,1.1));
#71263=CARTESIAN_POINT('',(33.9,3.2,1.));
#71264=CARTESIAN_POINT('',(34.,-2.,1.1));
#71265=CARTESIAN_POINT('Origin',(33.2,3.2,1.05));
#71266=CARTESIAN_POINT('Origin',(33.2,3.2,1.1));
#71267=CARTESIAN_POINT('Origin',(33.2,-3.2,1.));
#71268=CARTESIAN_POINT('',(34.,-3.2,144.9));
#71269=CARTESIAN_POINT('',(34.,-3.2,1.));
#71270=CARTESIAN_POINT('Origin',(33.2,-3.2,144.9));
#71271=CARTESIAN_POINT('Origin',(34.,-4.,1.));
#71272=CARTESIAN_POINT('',(34.,3.2,144.9));
#71273=CARTESIAN_POINT('',(34.,3.2,1.));
#71274=CARTESIAN_POINT('',(34.,-2.,144.9));
#71275=CARTESIAN_POINT('Origin',(33.2,3.2,1.));
#71276=CARTESIAN_POINT('Origin',(33.2,3.2,144.9));
#71277=CARTESIAN_POINT('Origin',(30.,3.95,38.75));
#71278=CARTESIAN_POINT('',(28.65,3.95,38.75));
#71279=CARTESIAN_POINT('Origin',(30.,-3.95,38.75));
#71280=CARTESIAN_POINT('',(28.65,-3.95,38.75));
#71281=CARTESIAN_POINT('Origin',(30.,3.95,56.75));
#71282=CARTESIAN_POINT('',(28.65,3.95,56.75));
#71283=CARTESIAN_POINT('Origin',(30.,-3.95,56.75));
#71284=CARTESIAN_POINT('',(28.65,-3.95,56.75));
#71285=CARTESIAN_POINT('Origin',(30.,3.95,65.75));
#71286=CARTESIAN_POINT('',(28.65,3.95,65.75));
#71287=CARTESIAN_POINT('Origin',(30.,-3.95,65.75));
#71288=CARTESIAN_POINT('',(28.65,-3.95,65.75));
#71289=CARTESIAN_POINT('Origin',(30.,3.95,74.75));
#71290=CARTESIAN_POINT('',(28.65,3.95,74.75));
#71291=CARTESIAN_POINT('Origin',(30.,-3.95,74.75));
#71292=CARTESIAN_POINT('',(28.65,-3.95,74.75));
#71293=CARTESIAN_POINT('Origin',(30.,3.95,83.75));
#71294=CARTESIAN_POINT('',(28.65,3.95,83.75));
#71295=CARTESIAN_POINT('Origin',(30.,-3.95,83.75));
#71296=CARTESIAN_POINT('',(28.65,-3.95,83.75));
#71297=CARTESIAN_POINT('Origin',(30.,3.95,47.75));
#71298=CARTESIAN_POINT('',(28.65,3.95,47.75));
#71299=CARTESIAN_POINT('Origin',(30.,-3.95,47.75));
#71300=CARTESIAN_POINT('',(28.65,-3.95,47.75));
#71301=CARTESIAN_POINT('Origin',(26.8,-3.2,144.95));
#71302=CARTESIAN_POINT('',(26.1,-3.2,145.));
#71303=CARTESIAN_POINT('',(26.,-3.2,144.9));
#71304=CARTESIAN_POINT('',(26.1,-3.2,145.));
#71305=CARTESIAN_POINT('Origin',(26.8,-3.2,144.9));
#71306=CARTESIAN_POINT('',(26.8,-3.9,145.));
#71307=CARTESIAN_POINT('',(26.8,-4.,144.9));
#71308=CARTESIAN_POINT('Origin',(26.8,-3.2,145.));
#71309=CARTESIAN_POINT('Origin',(26.05,2.,144.95));
#71310=CARTESIAN_POINT('',(26.1,3.2,145.));
#71311=CARTESIAN_POINT('',(26.1,2.,145.));
#71312=CARTESIAN_POINT('',(26.,3.2,144.9));
#71313=CARTESIAN_POINT('',(26.1,3.2,145.));
#71314=CARTESIAN_POINT('',(26.,2.,144.9));
#71315=CARTESIAN_POINT('Origin',(26.8,3.2,144.95));
#71316=CARTESIAN_POINT('',(26.8,3.9,145.));
#71317=CARTESIAN_POINT('',(26.8,3.9,145.));
#71318=CARTESIAN_POINT('Origin',(26.8,3.2,144.9));
#71319=CARTESIAN_POINT('Origin',(26.8,3.2,145.));
#71320=CARTESIAN_POINT('Origin',(32.,3.95,144.95));
#71321=CARTESIAN_POINT('',(33.2,3.9,145.));
#71322=CARTESIAN_POINT('',(32.,3.9,145.));
#71323=CARTESIAN_POINT('',(33.2,3.9,145.));
#71324=CARTESIAN_POINT('Origin',(33.2,3.2,144.95));
#71325=CARTESIAN_POINT('',(33.9,3.2,145.));
#71326=CARTESIAN_POINT('',(33.9,3.2,145.));
#71327=CARTESIAN_POINT('Origin',(33.2,3.2,145.));
#71328=CARTESIAN_POINT('Origin',(33.95,-2.,144.95));
#71329=CARTESIAN_POINT('',(33.9,-3.2,145.));
#71330=CARTESIAN_POINT('',(33.9,-2.,145.));
#71331=CARTESIAN_POINT('',(33.9,-3.2,145.));
#71332=CARTESIAN_POINT('Origin',(33.2,-3.2,144.95));
#71333=CARTESIAN_POINT('',(33.2,-3.9,145.));
#71334=CARTESIAN_POINT('',(33.2,-3.9,145.));
#71335=CARTESIAN_POINT('Origin',(33.2,-3.2,145.));
#71336=CARTESIAN_POINT('Origin',(28.,-3.95,144.95));
#71337=CARTESIAN_POINT('',(28.,-3.9,145.));
#71338=CARTESIAN_POINT('Origin',(26.8,-3.2,1.));
#71339=CARTESIAN_POINT('',(26.,-3.2,1.));
#71340=CARTESIAN_POINT('Origin',(30.,0.,145.));
#71341=CARTESIAN_POINT('',(26.8,3.6,145.));
#71342=CARTESIAN_POINT('',(26.4,3.2,145.));
#71343=CARTESIAN_POINT('Origin',(26.8,3.2,145.));
#71344=CARTESIAN_POINT('',(33.2,3.6,145.));
#71345=CARTESIAN_POINT('',(28.25,3.6,145.));
#71346=CARTESIAN_POINT('',(33.6,3.2,145.));
#71347=CARTESIAN_POINT('Origin',(33.2,3.2,145.));
#71348=CARTESIAN_POINT('',(33.6,-3.2,145.));
#71349=CARTESIAN_POINT('',(33.6,1.75,145.));
#71350=CARTESIAN_POINT('',(33.2,-3.6,145.));
#71351=CARTESIAN_POINT('Origin',(33.2,-3.2,145.));
#71352=CARTESIAN_POINT('',(26.8,-3.6,145.));
#71353=CARTESIAN_POINT('',(31.75,-3.6,145.));
#71354=CARTESIAN_POINT('',(26.4,-3.2,145.));
#71355=CARTESIAN_POINT('Origin',(26.8,-3.2,145.));
#71356=CARTESIAN_POINT('',(26.4,-1.75,145.));
#71357=CARTESIAN_POINT('Origin',(26.8,3.2,144.95));
#71358=CARTESIAN_POINT('',(26.5,3.2,144.9));
#71359=CARTESIAN_POINT('',(26.4,3.2,145.));
#71360=CARTESIAN_POINT('Origin',(26.8,3.2,144.9));
#71361=CARTESIAN_POINT('',(26.8,3.5,144.9));
#71362=CARTESIAN_POINT('Origin',(26.45,-1.75,144.95));
#71363=CARTESIAN_POINT('',(26.5,-3.2,144.9));
#71364=CARTESIAN_POINT('',(26.4,-3.2,145.));
#71365=CARTESIAN_POINT('',(26.5,-1.75,144.9));
#71366=CARTESIAN_POINT('Origin',(26.8,-3.2,144.95));
#71367=CARTESIAN_POINT('',(26.8,-3.6,145.));
#71368=CARTESIAN_POINT('Origin',(26.8,-3.2,144.9));
#71369=CARTESIAN_POINT('Origin',(31.75,-3.55,144.95));
#71370=CARTESIAN_POINT('',(33.2,-3.6,145.));
#71371=CARTESIAN_POINT('Origin',(33.2,-3.2,144.95));
#71372=CARTESIAN_POINT('',(33.6,-3.2,145.));
#71373=CARTESIAN_POINT('Origin',(33.55,1.75,144.95));
#71374=CARTESIAN_POINT('',(33.6,3.2,145.));
#71375=CARTESIAN_POINT('Origin',(33.2,3.2,144.95));
#71376=CARTESIAN_POINT('',(33.2,3.6,145.));
#71377=CARTESIAN_POINT('Origin',(28.25,3.55,144.95));
#71378=CARTESIAN_POINT('Origin',(26.8,3.2,1.));
#71379=CARTESIAN_POINT('',(26.5,3.2,1.));
#71380=CARTESIAN_POINT('Origin',(26.8,-3.2,1.));
#71381=CARTESIAN_POINT('',(26.5,-3.2,1.));
#71382=CARTESIAN_POINT('Origin',(26.5,-3.5,1.));
#71383=CARTESIAN_POINT('Origin',(26.,4.,1.));
#71384=CARTESIAN_POINT('',(26.,3.2,1.));
#71385=CARTESIAN_POINT('Origin',(26.8,3.2,1.));
#71386=CARTESIAN_POINT('',(0.,0.,0.));
#71387=CARTESIAN_POINT('',(0.,0.,0.));
#71388=CARTESIAN_POINT('',(0.,0.,0.));
#71389=CARTESIAN_POINT('',(0.,0.,0.));
#71390=CARTESIAN_POINT('',(0.,0.,0.));
#71391=CARTESIAN_POINT('',(0.,0.,0.));
#71392=CARTESIAN_POINT('',(0.,0.,0.));
#71393=CARTESIAN_POINT('',(0.,0.,0.));
#71394=CARTESIAN_POINT('',(0.,0.,0.));
#71395=CARTESIAN_POINT('',(0.,0.,0.));
#71396=CARTESIAN_POINT('',(0.,0.,0.));
#71397=CARTESIAN_POINT('',(0.,0.,0.));
#71398=CARTESIAN_POINT('',(0.,0.,0.));
#71399=CARTESIAN_POINT('',(18.5,0.,134.));
#71400=CARTESIAN_POINT('',(0.,0.,0.));
#71401=CARTESIAN_POINT('',(30.,-4.9,137.5));
#71402=CARTESIAN_POINT('',(30.,4.9,137.5));
#71403=CARTESIAN_POINT('',(30.,-4.6,137.5));
#71404=CARTESIAN_POINT('',(-60.,0.,0.));
#71405=CARTESIAN_POINT('',(-60.,0.,0.));
#71406=CARTESIAN_POINT('',(0.,0.,0.));
#71407=CARTESIAN_POINT('',(-37.,0.,0.));
#71408=CARTESIAN_POINT('',(-18.5,0.,134.));
#71409=CARTESIAN_POINT('',(18.5,0.,107.));
#71410=CARTESIAN_POINT('',(-18.5,0.,107.));
#71411=CARTESIAN_POINT('',(0.,0.,0.));
#71412=CARTESIAN_POINT('',(30.,-4.9,142.5));
#71413=CARTESIAN_POINT('',(-30.,-4.9,137.5));
#71414=CARTESIAN_POINT('',(-30.,-4.9,142.5));
#71415=CARTESIAN_POINT('',(30.,-5.1,6.));
#71416=CARTESIAN_POINT('',(30.,-5.1,17.));
#71417=CARTESIAN_POINT('',(-30.,-5.1,6.));
#71418=CARTESIAN_POINT('',(-30.,-5.1,17.));
#71419=CARTESIAN_POINT('',(30.,-4.3,33.5));
#71420=CARTESIAN_POINT('',(-30.,-4.3,33.5));
#71421=CARTESIAN_POINT('',(30.,4.9,142.5));
#71422=CARTESIAN_POINT('',(-30.,4.9,137.5));
#71423=CARTESIAN_POINT('',(-30.,4.9,142.5));
#71424=CARTESIAN_POINT('',(30.,5.1,6.));
#71425=CARTESIAN_POINT('',(30.,5.1,17.));
#71426=CARTESIAN_POINT('',(-30.,5.1,6.));
#71427=CARTESIAN_POINT('',(-30.,5.1,17.));
#71428=CARTESIAN_POINT('',(30.,4.8,33.5));
#71429=CARTESIAN_POINT('',(-30.,4.8,33.5));
#71430=CARTESIAN_POINT('',(30.,-4.6,142.5));
#71431=CARTESIAN_POINT('',(-30.,-4.6,137.5));
#71432=CARTESIAN_POINT('',(-30.,-4.6,142.5));
#71433=CARTESIAN_POINT('',(30.,-4.8,6.));
#71434=CARTESIAN_POINT('',(30.,-4.8,17.));
#71435=CARTESIAN_POINT('',(-30.,-4.8,6.));
#71436=CARTESIAN_POINT('',(-30.,-4.8,17.));
#71437=CARTESIAN_POINT('',(30.,-4.,33.5));
#71438=CARTESIAN_POINT('',(-30.,-4.,33.5));
#71439=CARTESIAN_POINT('',(30.,4.6,137.5));
#71440=CARTESIAN_POINT('',(30.,4.6,142.5));
#71441=CARTESIAN_POINT('',(-30.,4.6,137.5));
#71442=CARTESIAN_POINT('',(-30.,4.6,142.5));
#71443=CARTESIAN_POINT('',(30.,4.8,6.));
#71444=CARTESIAN_POINT('',(30.,4.8,17.));
#71445=CARTESIAN_POINT('',(-30.,4.8,6.));
#71446=CARTESIAN_POINT('',(-30.,4.8,17.));
#71447=CARTESIAN_POINT('',(30.,4.5,33.5));
#71448=CARTESIAN_POINT('',(-30.,4.5,33.5));
#71449=CARTESIAN_POINT('',(0.,0.,0.));
#71450=CARTESIAN_POINT('',(-60.,0.,0.));
#71451=UNCERTAINTY_MEASURE_WITH_UNIT(LENGTH_MEASURE(0.001),#71493,
'DISTANCE_ACCURACY_VALUE',
'Maximum model space distance between geometric entities at asserted c
onnectivities');
#71452=UNCERTAINTY_MEASURE_WITH_UNIT(LENGTH_MEASURE(0.001),#71493,
'DISTANCE_ACCURACY_VALUE',
'Maximum model space distance between geometric entities at asserted c
onnectivities');
#71453=UNCERTAINTY_MEASURE_WITH_UNIT(LENGTH_MEASURE(0.001),#71493,
'DISTANCE_ACCURACY_VALUE',
'Maximum model space distance between geometric entities at asserted c
onnectivities');
#71454=UNCERTAINTY_MEASURE_WITH_UNIT(LENGTH_MEASURE(0.001),#71493,
'DISTANCE_ACCURACY_VALUE',
'Maximum model space distance between geometric entities at asserted c
onnectivities');
#71455=UNCERTAINTY_MEASURE_WITH_UNIT(LENGTH_MEASURE(0.001),#71493,
'DISTANCE_ACCURACY_VALUE',
'Maximum model space distance between geometric entities at asserted c
onnectivities');
#71456=UNCERTAINTY_MEASURE_WITH_UNIT(LENGTH_MEASURE(0.001),#71493,
'DISTANCE_ACCURACY_VALUE',
'Maximum model space distance between geometric entities at asserted c
onnectivities');
#71457=UNCERTAINTY_MEASURE_WITH_UNIT(LENGTH_MEASURE(0.001),#71493,
'DISTANCE_ACCURACY_VALUE',
'Maximum model space distance between geometric entities at asserted c
onnectivities');
#71458=UNCERTAINTY_MEASURE_WITH_UNIT(LENGTH_MEASURE(0.001),#71493,
'DISTANCE_ACCURACY_VALUE',
'Maximum model space distance between geometric entities at asserted c
onnectivities');
#71459=UNCERTAINTY_MEASURE_WITH_UNIT(LENGTH_MEASURE(0.001),#71493,
'DISTANCE_ACCURACY_VALUE',
'Maximum model space distance between geometric entities at asserted c
onnectivities');
#71460=UNCERTAINTY_MEASURE_WITH_UNIT(LENGTH_MEASURE(0.001),#71493,
'DISTANCE_ACCURACY_VALUE',
'Maximum model space distance between geometric entities at asserted c
onnectivities');
#71461=UNCERTAINTY_MEASURE_WITH_UNIT(LENGTH_MEASURE(0.001),#71493,
'DISTANCE_ACCURACY_VALUE',
'Maximum model space distance between geometric entities at asserted c
onnectivities');
#71462=UNCERTAINTY_MEASURE_WITH_UNIT(LENGTH_MEASURE(0.001),#71493,
'DISTANCE_ACCURACY_VALUE',
'Maximum model space distance between geometric entities at asserted c
onnectivities');
#71463=UNCERTAINTY_MEASURE_WITH_UNIT(LENGTH_MEASURE(0.001),#71493,
'DISTANCE_ACCURACY_VALUE',
'Maximum model space distance between geometric entities at asserted c
onnectivities');
#71464=UNCERTAINTY_MEASURE_WITH_UNIT(LENGTH_MEASURE(0.001),#71493,
'DISTANCE_ACCURACY_VALUE',
'Maximum model space distance between geometric entities at asserted c
onnectivities');
#71465=UNCERTAINTY_MEASURE_WITH_UNIT(LENGTH_MEASURE(0.001),#71493,
'DISTANCE_ACCURACY_VALUE',
'Maximum model space distance between geometric entities at asserted c
onnectivities');
#71466=UNCERTAINTY_MEASURE_WITH_UNIT(LENGTH_MEASURE(0.001),#71493,
'DISTANCE_ACCURACY_VALUE',
'Maximum model space distance between geometric entities at asserted c
onnectivities');
#71467=UNCERTAINTY_MEASURE_WITH_UNIT(LENGTH_MEASURE(0.001),#71493,
'DISTANCE_ACCURACY_VALUE',
'Maximum model space distance between geometric entities at asserted c
onnectivities');
#71468=UNCERTAINTY_MEASURE_WITH_UNIT(LENGTH_MEASURE(0.001),#71493,
'DISTANCE_ACCURACY_VALUE',
'Maximum model space distance between geometric entities at asserted c
onnectivities');
#71469=UNCERTAINTY_MEASURE_WITH_UNIT(LENGTH_MEASURE(0.001),#71493,
'DISTANCE_ACCURACY_VALUE',
'Maximum model space distance between geometric entities at asserted c
onnectivities');
#71470=UNCERTAINTY_MEASURE_WITH_UNIT(LENGTH_MEASURE(0.001),#71493,
'DISTANCE_ACCURACY_VALUE',
'Maximum model space distance between geometric entities at asserted c
onnectivities');
#71471=UNCERTAINTY_MEASURE_WITH_UNIT(LENGTH_MEASURE(0.001),#71493,
'DISTANCE_ACCURACY_VALUE',
'Maximum model space distance between geometric entities at asserted c
onnectivities');
#71472=(
GEOMETRIC_REPRESENTATION_CONTEXT(3)
GLOBAL_UNCERTAINTY_ASSIGNED_CONTEXT((#71451))
GLOBAL_UNIT_ASSIGNED_CONTEXT((#71493,#71495,#71496))
REPRESENTATION_CONTEXT('','3D')
);
#71473=(
GEOMETRIC_REPRESENTATION_CONTEXT(3)
GLOBAL_UNCERTAINTY_ASSIGNED_CONTEXT((#71452))
GLOBAL_UNIT_ASSIGNED_CONTEXT((#71493,#71495,#71496))
REPRESENTATION_CONTEXT('','3D')
);
#71474=(
GEOMETRIC_REPRESENTATION_CONTEXT(3)
GLOBAL_UNCERTAINTY_ASSIGNED_CONTEXT((#71453))
GLOBAL_UNIT_ASSIGNED_CONTEXT((#71493,#71495,#71496))
REPRESENTATION_CONTEXT('','3D')
);
#71475=(
GEOMETRIC_REPRESENTATION_CONTEXT(3)
GLOBAL_UNCERTAINTY_ASSIGNED_CONTEXT((#71454))
GLOBAL_UNIT_ASSIGNED_CONTEXT((#71493,#71495,#71496))
REPRESENTATION_CONTEXT('','3D')
);
#71476=(
GEOMETRIC_REPRESENTATION_CONTEXT(3)
GLOBAL_UNCERTAINTY_ASSIGNED_CONTEXT((#71455))
GLOBAL_UNIT_ASSIGNED_CONTEXT((#71493,#71495,#71496))
REPRESENTATION_CONTEXT('','3D')
);
#71477=(
GEOMETRIC_REPRESENTATION_CONTEXT(3)
GLOBAL_UNCERTAINTY_ASSIGNED_CONTEXT((#71456))
GLOBAL_UNIT_ASSIGNED_CONTEXT((#71493,#71495,#71496))
REPRESENTATION_CONTEXT('','3D')
);
#71478=(
GEOMETRIC_REPRESENTATION_CONTEXT(3)
GLOBAL_UNCERTAINTY_ASSIGNED_CONTEXT((#71457))
GLOBAL_UNIT_ASSIGNED_CONTEXT((#71493,#71495,#71496))
REPRESENTATION_CONTEXT('','3D')
);
#71479=(
GEOMETRIC_REPRESENTATION_CONTEXT(3)
GLOBAL_UNCERTAINTY_ASSIGNED_CONTEXT((#71458))
GLOBAL_UNIT_ASSIGNED_CONTEXT((#71493,#71495,#71496))
REPRESENTATION_CONTEXT('','3D')
);
#71480=(
GEOMETRIC_REPRESENTATION_CONTEXT(3)
GLOBAL_UNCERTAINTY_ASSIGNED_CONTEXT((#71459))
GLOBAL_UNIT_ASSIGNED_CONTEXT((#71493,#71495,#71496))
REPRESENTATION_CONTEXT('','3D')
);
#71481=(
GEOMETRIC_REPRESENTATION_CONTEXT(3)
GLOBAL_UNCERTAINTY_ASSIGNED_CONTEXT((#71460))
GLOBAL_UNIT_ASSIGNED_CONTEXT((#71493,#71495,#71496))
REPRESENTATION_CONTEXT('','3D')
);
#71482=(
GEOMETRIC_REPRESENTATION_CONTEXT(3)
GLOBAL_UNCERTAINTY_ASSIGNED_CONTEXT((#71461))
GLOBAL_UNIT_ASSIGNED_CONTEXT((#71493,#71495,#71496))
REPRESENTATION_CONTEXT('','3D')
);
#71483=(
GEOMETRIC_REPRESENTATION_CONTEXT(3)
GLOBAL_UNCERTAINTY_ASSIGNED_CONTEXT((#71462))
GLOBAL_UNIT_ASSIGNED_CONTEXT((#71493,#71495,#71496))
REPRESENTATION_CONTEXT('','3D')
);
#71484=(
GEOMETRIC_REPRESENTATION_CONTEXT(3)
GLOBAL_UNCERTAINTY_ASSIGNED_CONTEXT((#71463))
GLOBAL_UNIT_ASSIGNED_CONTEXT((#71493,#71495,#71496))
REPRESENTATION_CONTEXT('','3D')
);
#71485=(
GEOMETRIC_REPRESENTATION_CONTEXT(3)
GLOBAL_UNCERTAINTY_ASSIGNED_CONTEXT((#71464))
GLOBAL_UNIT_ASSIGNED_CONTEXT((#71493,#71495,#71496))
REPRESENTATION_CONTEXT('','3D')
);
#71486=(
GEOMETRIC_REPRESENTATION_CONTEXT(3)
GLOBAL_UNCERTAINTY_ASSIGNED_CONTEXT((#71465))
GLOBAL_UNIT_ASSIGNED_CONTEXT((#71493,#71495,#71496))
REPRESENTATION_CONTEXT('','3D')
);
#71487=(
GEOMETRIC_REPRESENTATION_CONTEXT(3)
GLOBAL_UNCERTAINTY_ASSIGNED_CONTEXT((#71466))
GLOBAL_UNIT_ASSIGNED_CONTEXT((#71493,#71495,#71496))
REPRESENTATION_CONTEXT('','3D')
);
#71488=(
GEOMETRIC_REPRESENTATION_CONTEXT(3)
GLOBAL_UNCERTAINTY_ASSIGNED_CONTEXT((#71467))
GLOBAL_UNIT_ASSIGNED_CONTEXT((#71493,#71495,#71496))
REPRESENTATION_CONTEXT('','3D')
);
#71489=(
GEOMETRIC_REPRESENTATION_CONTEXT(3)
GLOBAL_UNCERTAINTY_ASSIGNED_CONTEXT((#71468))
GLOBAL_UNIT_ASSIGNED_CONTEXT((#71493,#71495,#71496))
REPRESENTATION_CONTEXT('','3D')
);
#71490=(
GEOMETRIC_REPRESENTATION_CONTEXT(3)
GLOBAL_UNCERTAINTY_ASSIGNED_CONTEXT((#71469))
GLOBAL_UNIT_ASSIGNED_CONTEXT((#71493,#71495,#71496))
REPRESENTATION_CONTEXT('','3D')
);
#71491=(
GEOMETRIC_REPRESENTATION_CONTEXT(3)
GLOBAL_UNCERTAINTY_ASSIGNED_CONTEXT((#71470))
GLOBAL_UNIT_ASSIGNED_CONTEXT((#71493,#71495,#71496))
REPRESENTATION_CONTEXT('','3D')
);
#71492=(
GEOMETRIC_REPRESENTATION_CONTEXT(3)
GLOBAL_UNCERTAINTY_ASSIGNED_CONTEXT((#71471))
GLOBAL_UNIT_ASSIGNED_CONTEXT((#71493,#71495,#71496))
REPRESENTATION_CONTEXT('','3D')
);
#71493=(
LENGTH_UNIT()
NAMED_UNIT(*)
SI_UNIT(.CENTI.,.METRE.)
);
#71494=(
LENGTH_UNIT()
NAMED_UNIT(*)
SI_UNIT($,.METRE.)
);
#71495=(
NAMED_UNIT(*)
PLANE_ANGLE_UNIT()
SI_UNIT($,.RADIAN.)
);
#71496=(
NAMED_UNIT(*)
SI_UNIT($,.STERADIAN.)
SOLID_ANGLE_UNIT()
);
#71497=SHAPE_DEFINITION_REPRESENTATION(#71517,#71602);
#71498=SHAPE_DEFINITION_REPRESENTATION(#71518,#71603);
#71499=SHAPE_DEFINITION_REPRESENTATION(#71519,#71604);
#71500=SHAPE_DEFINITION_REPRESENTATION(#71520,#71605);
#71501=SHAPE_DEFINITION_REPRESENTATION(#71521,#71606);
#71502=SHAPE_DEFINITION_REPRESENTATION(#71522,#71607);
#71503=SHAPE_DEFINITION_REPRESENTATION(#71523,#71608);
#71504=SHAPE_DEFINITION_REPRESENTATION(#71524,#71609);
#71505=SHAPE_DEFINITION_REPRESENTATION(#71525,#71610);
#71506=SHAPE_DEFINITION_REPRESENTATION(#71526,#71611);
#71507=SHAPE_DEFINITION_REPRESENTATION(#71527,#71612);
#71508=SHAPE_DEFINITION_REPRESENTATION(#71528,#71613);
#71509=SHAPE_DEFINITION_REPRESENTATION(#71529,#71614);
#71510=SHAPE_DEFINITION_REPRESENTATION(#71530,#71615);
#71511=SHAPE_DEFINITION_REPRESENTATION(#71531,#71616);
#71512=SHAPE_DEFINITION_REPRESENTATION(#71532,#71617);
#71513=SHAPE_DEFINITION_REPRESENTATION(#71533,#71618);
#71514=SHAPE_DEFINITION_REPRESENTATION(#71534,#71619);
#71515=SHAPE_DEFINITION_REPRESENTATION(#71535,#71620);
#71516=SHAPE_DEFINITION_REPRESENTATION(#71536,#71621);
#71517=PRODUCT_DEFINITION_SHAPE('',$,#71623);
#71518=PRODUCT_DEFINITION_SHAPE('',$,#71624);
#71519=PRODUCT_DEFINITION_SHAPE('',$,#71625);
#71520=PRODUCT_DEFINITION_SHAPE('',$,#71626);
#71521=PRODUCT_DEFINITION_SHAPE('',$,#71627);
#71522=PRODUCT_DEFINITION_SHAPE('',$,#71628);
#71523=PRODUCT_DEFINITION_SHAPE('',$,#71629);
#71524=PRODUCT_DEFINITION_SHAPE('',$,#71630);
#71525=PRODUCT_DEFINITION_SHAPE('',$,#71631);
#71526=PRODUCT_DEFINITION_SHAPE('',$,#71632);
#71527=PRODUCT_DEFINITION_SHAPE('',$,#71633);
#71528=PRODUCT_DEFINITION_SHAPE('',$,#71634);
#71529=PRODUCT_DEFINITION_SHAPE('',$,#71635);
#71530=PRODUCT_DEFINITION_SHAPE('',$,#71636);
#71531=PRODUCT_DEFINITION_SHAPE('',$,#71637);
#71532=PRODUCT_DEFINITION_SHAPE('',$,#71638);
#71533=PRODUCT_DEFINITION_SHAPE('',$,#71639);
#71534=PRODUCT_DEFINITION_SHAPE('',$,#71640);
#71535=PRODUCT_DEFINITION_SHAPE('',$,#71641);
#71536=PRODUCT_DEFINITION_SHAPE('',$,#71642);
#71537=PRODUCT_DEFINITION_SHAPE($,$,#206);
#71538=PRODUCT_DEFINITION_SHAPE($,$,#207);
#71539=PRODUCT_DEFINITION_SHAPE($,$,#208);
#71540=PRODUCT_DEFINITION_SHAPE($,$,#209);
#71541=PRODUCT_DEFINITION_SHAPE($,$,#210);
#71542=PRODUCT_DEFINITION_SHAPE($,$,#211);
#71543=PRODUCT_DEFINITION_SHAPE($,$,#212);
#71544=PRODUCT_DEFINITION_SHAPE($,$,#213);
#71545=PRODUCT_DEFINITION_SHAPE($,$,#214);
#71546=PRODUCT_DEFINITION_SHAPE($,$,#215);
#71547=PRODUCT_DEFINITION_SHAPE($,$,#216);
#71548=PRODUCT_DEFINITION_SHAPE($,$,#217);
#71549=PRODUCT_DEFINITION_SHAPE($,$,#218);
#71550=PRODUCT_DEFINITION_SHAPE($,$,#219);
#71551=PRODUCT_DEFINITION_SHAPE($,$,#220);
#71552=PRODUCT_DEFINITION_SHAPE($,$,#221);
#71553=PRODUCT_DEFINITION_SHAPE($,$,#222);
#71554=PRODUCT_DEFINITION_SHAPE($,$,#223);
#71555=PRODUCT_DEFINITION_SHAPE($,$,#224);
#71556=PRODUCT_DEFINITION_SHAPE($,$,#225);
#71557=PRODUCT_DEFINITION_SHAPE($,$,#226);
#71558=PRODUCT_DEFINITION_SHAPE($,$,#227);
#71559=PRODUCT_DEFINITION_SHAPE($,$,#228);
#71560=PRODUCT_DEFINITION_SHAPE($,$,#229);
#71561=PRODUCT_DEFINITION_SHAPE($,$,#230);
#71562=PRODUCT_DEFINITION_SHAPE($,$,#231);
#71563=PRODUCT_DEFINITION_SHAPE($,$,#232);
#71564=PRODUCT_DEFINITION_SHAPE($,$,#233);
#71565=PRODUCT_DEFINITION_SHAPE($,$,#234);
#71566=PRODUCT_DEFINITION_SHAPE($,$,#235);
#71567=PRODUCT_DEFINITION_SHAPE($,$,#236);
#71568=PRODUCT_DEFINITION_SHAPE($,$,#237);
#71569=PRODUCT_DEFINITION_SHAPE($,$,#238);
#71570=PRODUCT_DEFINITION_SHAPE($,$,#239);
#71571=PRODUCT_DEFINITION_SHAPE($,$,#240);
#71572=PRODUCT_DEFINITION_SHAPE($,$,#241);
#71573=PRODUCT_DEFINITION_SHAPE($,$,#242);
#71574=PRODUCT_DEFINITION_SHAPE($,$,#243);
#71575=PRODUCT_DEFINITION_SHAPE($,$,#244);
#71576=PRODUCT_DEFINITION_SHAPE($,$,#245);
#71577=PRODUCT_DEFINITION_SHAPE($,$,#246);
#71578=PRODUCT_DEFINITION_SHAPE($,$,#247);
#71579=PRODUCT_DEFINITION_SHAPE($,$,#248);
#71580=PRODUCT_DEFINITION_SHAPE($,$,#249);
#71581=PRODUCT_DEFINITION_SHAPE($,$,#250);
#71582=PRODUCT_DEFINITION_SHAPE($,$,#251);
#71583=PRODUCT_DEFINITION_SHAPE($,$,#252);
#71584=PRODUCT_DEFINITION_SHAPE($,$,#253);
#71585=PRODUCT_DEFINITION_SHAPE($,$,#254);
#71586=PRODUCT_DEFINITION_SHAPE($,$,#255);
#71587=PRODUCT_DEFINITION_SHAPE($,$,#256);
#71588=PRODUCT_DEFINITION_SHAPE($,$,#257);
#71589=PRODUCT_DEFINITION_SHAPE($,$,#258);
#71590=PRODUCT_DEFINITION_SHAPE($,$,#259);
#71591=PRODUCT_DEFINITION_SHAPE($,$,#260);
#71592=PRODUCT_DEFINITION_SHAPE($,$,#261);
#71593=PRODUCT_DEFINITION_SHAPE($,$,#262);
#71594=PRODUCT_DEFINITION_SHAPE($,$,#263);
#71595=PRODUCT_DEFINITION_SHAPE($,$,#264);
#71596=PRODUCT_DEFINITION_SHAPE($,$,#265);
#71597=PRODUCT_DEFINITION_SHAPE($,$,#266);
#71598=PRODUCT_DEFINITION_SHAPE($,$,#267);
#71599=PRODUCT_DEFINITION_SHAPE($,$,#268);
#71600=PRODUCT_DEFINITION_SHAPE($,$,#269);
#71601=PRODUCT_DEFINITION_SHAPE($,$,#270);
#71602=SHAPE_REPRESENTATION('',(#28688,#30790,#30791,#30792,#30793,#30794,
#30795,#30796,#30797,#30798,#30799,#30800,#30801,#30802,#30803,#30804,#30805,
#30806,#30807,#30808,#30809,#30810,#30811,#30812,#30813,#30814,#30815,#30816,
#30817,#30818,#30819,#30820,#30821,#30822,#30823,#30824,#30825,#30826,#30827,
#30828,#30829,#30830,#30831,#30832,#30833,#30834,#30835,#30836,#30837,#30838,
#30839,#30840,#30841,#30842,#30843,#30844,#30845,#30846,#30847,#30848,#30849,
#30850,#30851,#30852,#30853,#30854),#71472);
#71603=SHAPE_REPRESENTATION('',(#28689),#71473);
#71604=SHAPE_REPRESENTATION('',(#29045),#71474);
#71605=SHAPE_REPRESENTATION('',(#29181),#71475);
#71606=SHAPE_REPRESENTATION('',(#29306),#71476);
#71607=SHAPE_REPRESENTATION('',(#29346),#71477);
#71608=SHAPE_REPRESENTATION('',(#29535),#71478);
#71609=SHAPE_REPRESENTATION('',(#29736),#71479);
#71610=SHAPE_REPRESENTATION('',(#29878),#71480);
#71611=SHAPE_REPRESENTATION('',(#29982),#71481);
#71612=SHAPE_REPRESENTATION('',(#30008),#71482);
#71613=SHAPE_REPRESENTATION('',(#30013),#71483);
#71614=SHAPE_REPRESENTATION('',(#30164),#71484);
#71615=SHAPE_REPRESENTATION('',(#30184),#71485);
#71616=SHAPE_REPRESENTATION('',(#30238),#71486);
#71617=SHAPE_REPRESENTATION('',(#30284),#71487);
#71618=SHAPE_REPRESENTATION('',(#30444),#71488);
#71619=SHAPE_REPRESENTATION('',(#30464),#71489);
#71620=SHAPE_REPRESENTATION('',(#30477),#71490);
#71621=SHAPE_REPRESENTATION('',(#30553),#71491);
#71622=PRODUCT_DEFINITION_CONTEXT('part definition',#71684,'design');
#71623=PRODUCT_DEFINITION('2026-10-19-03-21-34-676','MAS-306',#71643,#71622);
#71624=PRODUCT_DEFINITION('2026-10-19-03-21-47-060',
'02_Top_Head_Beam_Twin_RHS100x50x6',#71644,#71622);
#71625=PRODUCT_DEFINITION('2026-10-19-03-21-49-945',
'03_Movable_Press_Platen_Twin_C80_Shaft_D50',#71645,#71622);
#71626=PRODUCT_DEFINITION('2026-10-19-03-21-51-757',
'04_Height-Adjustable_Bed_Twin_C100x50x6',#71646,#71622);
#71627=PRODUCT_DEFINITION('2026-10-19-03-21-58-368',
'08_Lower_Cross_Brace_L680_L50x50x5',#71647,#71622);
#71628=PRODUCT_DEFINITION('2026-10-19-03-22-09-909',
'09_Bottle_Jack_Body_20T_Hand_Pump',#71648,#71622);
#71629=PRODUCT_DEFINITION('2026-10-19-03-22-19-429',
'10_Jack_Ram_D53_Extension_Screw_M30',#71649,#71622);
#71630=PRODUCT_DEFINITION('2026-10-19-03-22-35-930',
'12_Hydraulic_Release_Valve_Knob_M8',#71650,#71622);
#71631=PRODUCT_DEFINITION('2026-10-19-03-22-43-799',
'13_Pressure_Gauge_D63_0-20T',#71651,#71622);
#71632=PRODUCT_DEFINITION('2026-10-19-03-21-53-578',
'05_Bed_Support_Pin_D25x255_Ring_Handle',#71652,#71622);
#71633=PRODUCT_DEFINITION('2026-10-19-03-21-54-863',
'06_R-Clip_D3_for_Pin_D25',#71653,#71622);
#71634=PRODUCT_DEFINITION('2026-10-19-03-21-55-709',
'07_Frame_Base_Anchor_Plate_600x175_Foot',#71654,#71622);
#71635=PRODUCT_DEFINITION('2026-10-19-03-22-52-363',
'14_Ram_Return_Extension_Spring_D30x4',#71655,#71622);
#71636=PRODUCT_DEFINITION('2026-10-19-03-23-06-453',
'15_DIN_580_M10_Eye_Bolt',#71656,#71622);
#71637=PRODUCT_DEFINITION('2026-10-19-03-23-09-453',
'16_Press_V-Block_200x90x40',#71657,#71622);
#71638=PRODUCT_DEFINITION('2026-10-19-03-23-11-739',
'17_ISO_4017_M16x120-8.8',#71658,#71622);
#71639=PRODUCT_DEFINITION('2026-10-19-03-23-16-216','18_ISO_4032_M16-8',
#71659,#71622);
#71640=PRODUCT_DEFINITION('2026-10-19-03-23-19-103',
'19_ISO_7089_16-200HV_Washer',#71660,#71622);
#71641=PRODUCT_DEFINITION('2026-10-19-03-30-44-438',
'11_Pump_Operating_Handle_Arm',#71661,#71622);
#71642=PRODUCT_DEFINITION('2026-10-19-03-21-44-299',
'01_Upright_Column_L1440_RHS80x80x5',#71662,#71622);
#71643=PRODUCT_DEFINITION_FORMATION('',$,#71686);
#71644=PRODUCT_DEFINITION_FORMATION('',$,#71687);
#71645=PRODUCT_DEFINITION_FORMATION('',$,#71688);
#71646=PRODUCT_DEFINITION_FORMATION('',$,#71689);
#71647=PRODUCT_DEFINITION_FORMATION('',$,#71690);
#71648=PRODUCT_DEFINITION_FORMATION('',$,#71691);
#71649=PRODUCT_DEFINITION_FORMATION('',$,#71692);
#71650=PRODUCT_DEFINITION_FORMATION('',$,#71693);
#71651=PRODUCT_DEFINITION_FORMATION('',$,#71694);
#71652=PRODUCT_DEFINITION_FORMATION('',$,#71695);
#71653=PRODUCT_DEFINITION_FORMATION('',$,#71696);
#71654=PRODUCT_DEFINITION_FORMATION('',$,#71697);
#71655=PRODUCT_DEFINITION_FORMATION('',$,#71698);
#71656=PRODUCT_DEFINITION_FORMATION('',$,#71699);
#71657=PRODUCT_DEFINITION_FORMATION('',$,#71700);
#71658=PRODUCT_DEFINITION_FORMATION('',$,#71701);
#71659=PRODUCT_DEFINITION_FORMATION('',$,#71702);
#71660=PRODUCT_DEFINITION_FORMATION('',$,#71703);
#71661=PRODUCT_DEFINITION_FORMATION('',$,#71704);
#71662=PRODUCT_DEFINITION_FORMATION('',$,#71705);
#71663=PRODUCT_RELATED_PRODUCT_CATEGORY('MAS-306','MAS-306',(#71686));
#71664=PRODUCT_RELATED_PRODUCT_CATEGORY(
'02_Top_Head_Beam_Twin_RHS100x50x6','02_Top_Head_Beam_Twin_RHS100x50x6',
(#71687));
#71665=PRODUCT_RELATED_PRODUCT_CATEGORY(
'03_Movable_Press_Platen_Twin_C80_Shaft_D50',
'03_Movable_Press_Platen_Twin_C80_Shaft_D50',(#71688));
#71666=PRODUCT_RELATED_PRODUCT_CATEGORY(
'04_Height-Adjustable_Bed_Twin_C100x50x6',
'04_Height-Adjustable_Bed_Twin_C100x50x6',(#71689));
#71667=PRODUCT_RELATED_PRODUCT_CATEGORY(
'08_Lower_Cross_Brace_L680_L50x50x5',
'08_Lower_Cross_Brace_L680_L50x50x5',(#71690));
#71668=PRODUCT_RELATED_PRODUCT_CATEGORY(
'09_Bottle_Jack_Body_20T_Hand_Pump','09_Bottle_Jack_Body_20T_Hand_Pump',
(#71691));
#71669=PRODUCT_RELATED_PRODUCT_CATEGORY(
'10_Jack_Ram_D53_Extension_Screw_M30',
'10_Jack_Ram_D53_Extension_Screw_M30',(#71692));
#71670=PRODUCT_RELATED_PRODUCT_CATEGORY(
'12_Hydraulic_Release_Valve_Knob_M8',
'12_Hydraulic_Release_Valve_Knob_M8',(#71693));
#71671=PRODUCT_RELATED_PRODUCT_CATEGORY('13_Pressure_Gauge_D63_0-20T',
'13_Pressure_Gauge_D63_0-20T',(#71694));
#71672=PRODUCT_RELATED_PRODUCT_CATEGORY(
'05_Bed_Support_Pin_D25x255_Ring_Handle',
'05_Bed_Support_Pin_D25x255_Ring_Handle',(#71695));
#71673=PRODUCT_RELATED_PRODUCT_CATEGORY('06_R-Clip_D3_for_Pin_D25',
'06_R-Clip_D3_for_Pin_D25',(#71696));
#71674=PRODUCT_RELATED_PRODUCT_CATEGORY(
'07_Frame_Base_Anchor_Plate_600x175_Foot',
'07_Frame_Base_Anchor_Plate_600x175_Foot',(#71697));
#71675=PRODUCT_RELATED_PRODUCT_CATEGORY(
'14_Ram_Return_Extension_Spring_D30x4',
'14_Ram_Return_Extension_Spring_D30x4',(#71698));
#71676=PRODUCT_RELATED_PRODUCT_CATEGORY('15_DIN_580_M10_Eye_Bolt',
'15_DIN_580_M10_Eye_Bolt',(#71699));
#71677=PRODUCT_RELATED_PRODUCT_CATEGORY('16_Press_V-Block_200x90x40',
'16_Press_V-Block_200x90x40',(#71700));
#71678=PRODUCT_RELATED_PRODUCT_CATEGORY('17_ISO_4017_M16x120-8.8',
'17_ISO_4017_M16x120-8.8',(#71701));
#71679=PRODUCT_RELATED_PRODUCT_CATEGORY('18_ISO_4032_M16-8',
'18_ISO_4032_M16-8',(#71702));
#71680=PRODUCT_RELATED_PRODUCT_CATEGORY('19_ISO_7089_16-200HV_Washer',
'19_ISO_7089_16-200HV_Washer',(#71703));
#71681=PRODUCT_RELATED_PRODUCT_CATEGORY('11_Pump_Operating_Handle_Arm',
'11_Pump_Operating_Handle_Arm',(#71704));
#71682=PRODUCT_RELATED_PRODUCT_CATEGORY(
'01_Upright_Column_L1440_RHS80x80x5',
'01_Upright_Column_L1440_RHS80x80x5',(#71705));
#71683=APPLICATION_PROTOCOL_DEFINITION('international standard',
'automotive_design',2009,#71684);
#71684=APPLICATION_CONTEXT(
'Core Data for Automotive Mechanical Design Process');
#71685=PRODUCT_CONTEXT('part definition',#71684,'mechanical');
#71686=PRODUCT('2026-10-19-03-21-34-676','MAS-306',$,(#71685));
#71687=PRODUCT('2026-10-19-03-21-47-060',
'02_Top_Head_Beam_Twin_RHS100x50x6',$,(#71685));
#71688=PRODUCT('2026-10-19-03-21-49-945',
'03_Movable_Press_Platen_Twin_C80_Shaft_D50',$,(#71685));
#71689=PRODUCT('2026-10-19-03-21-51-757',
'04_Height-Adjustable_Bed_Twin_C100x50x6',$,(#71685));
#71690=PRODUCT('2026-10-19-03-21-58-368',
'08_Lower_Cross_Brace_L680_L50x50x5',$,(#71685));
#71691=PRODUCT('2026-10-19-03-22-09-909',
'09_Bottle_Jack_Body_20T_Hand_Pump',$,(#71685));
#71692=PRODUCT('2026-10-19-03-22-19-429',
'10_Jack_Ram_D53_Extension_Screw_M30',$,(#71685));
#71693=PRODUCT('2026-10-19-03-22-35-930',
'12_Hydraulic_Release_Valve_Knob_M8',$,(#71685));
#71694=PRODUCT('2026-10-19-03-22-43-799','13_Pressure_Gauge_D63_0-20T',
$,(#71685));
#71695=PRODUCT('2026-10-19-03-21-53-578',
'05_Bed_Support_Pin_D25x255_Ring_Handle',$,(#71685));
#71696=PRODUCT('2026-10-19-03-21-54-863','06_R-Clip_D3_for_Pin_D25',$,(#71685));
#71697=PRODUCT('2026-10-19-03-21-55-709',
'07_Frame_Base_Anchor_Plate_600x175_Foot',$,(#71685));
#71698=PRODUCT('2026-10-19-03-22-52-363',
'14_Ram_Return_Extension_Spring_D30x4',$,(#71685));
#71699=PRODUCT('2026-10-19-03-23-06-453','15_DIN_580_M10_Eye_Bolt',$,(#71685));
#71700=PRODUCT('2026-10-19-03-23-09-453','16_Press_V-Block_200x90x40',$,
(#71685));
#71701=PRODUCT('2026-10-19-03-23-11-739','17_ISO_4017_M16x120-8.8',$,(#71685));
#71702=PRODUCT('2026-10-19-03-23-16-216','18_ISO_4032_M16-8',$,(#71685));
#71703=PRODUCT('2026-10-19-03-23-19-103','19_ISO_7089_16-200HV_Washer',
$,(#71685));
#71704=PRODUCT('2026-10-19-03-30-44-438','11_Pump_Operating_Handle_Arm',
$,(#71685));
#71705=PRODUCT('2026-10-19-03-21-44-299',
'01_Upright_Column_L1440_RHS80x80x5',$,(#71685));
#71706=PRESENTATION_STYLE_ASSIGNMENT((#71728));
#71707=PRESENTATION_STYLE_ASSIGNMENT((#71729));
#71708=PRESENTATION_STYLE_ASSIGNMENT((#71730));
#71709=PRESENTATION_STYLE_ASSIGNMENT((#71731));
#71710=PRESENTATION_STYLE_ASSIGNMENT((#71732));
#71711=PRESENTATION_STYLE_ASSIGNMENT((#71733));
#71712=PRESENTATION_STYLE_ASSIGNMENT((#71734));
#71713=PRESENTATION_STYLE_ASSIGNMENT((#71735));
#71714=PRESENTATION_STYLE_ASSIGNMENT((#71736));
#71715=PRESENTATION_STYLE_ASSIGNMENT((#71737));
#71716=PRESENTATION_STYLE_ASSIGNMENT((#71738));
#71717=PRESENTATION_STYLE_ASSIGNMENT((#71739));
#71718=PRESENTATION_STYLE_ASSIGNMENT((#71740));
#71719=PRESENTATION_STYLE_ASSIGNMENT((#71741));
#71720=PRESENTATION_STYLE_ASSIGNMENT((#71742));
#71721=PRESENTATION_STYLE_ASSIGNMENT((#71743));
#71722=PRESENTATION_STYLE_ASSIGNMENT((#71744));
#71723=PRESENTATION_STYLE_ASSIGNMENT((#71745));
#71724=PRESENTATION_STYLE_ASSIGNMENT((#71746));
#71725=PRESENTATION_STYLE_ASSIGNMENT((#71747));
#71726=PRESENTATION_STYLE_ASSIGNMENT((#71748));
#71727=PRESENTATION_STYLE_ASSIGNMENT((#71749));
#71728=SURFACE_STYLE_USAGE(.BOTH.,#71750);
#71729=SURFACE_STYLE_USAGE(.BOTH.,#71751);
#71730=SURFACE_STYLE_USAGE(.BOTH.,#71752);
#71731=SURFACE_STYLE_USAGE(.BOTH.,#71753);
#71732=SURFACE_STYLE_USAGE(.BOTH.,#71754);
#71733=SURFACE_STYLE_USAGE(.BOTH.,#71755);
#71734=SURFACE_STYLE_USAGE(.BOTH.,#71756);
#71735=SURFACE_STYLE_USAGE(.BOTH.,#71757);
#71736=SURFACE_STYLE_USAGE(.BOTH.,#71758);
#71737=SURFACE_STYLE_USAGE(.BOTH.,#71759);
#71738=SURFACE_STYLE_USAGE(.BOTH.,#71760);
#71739=SURFACE_STYLE_USAGE(.BOTH.,#71761);
#71740=SURFACE_STYLE_USAGE(.BOTH.,#71762);
#71741=SURFACE_STYLE_USAGE(.BOTH.,#71763);
#71742=SURFACE_STYLE_USAGE(.BOTH.,#71764);
#71743=SURFACE_STYLE_USAGE(.BOTH.,#71765);
#71744=SURFACE_STYLE_USAGE(.BOTH.,#71766);
#71745=SURFACE_STYLE_USAGE(.BOTH.,#71767);
#71746=SURFACE_STYLE_USAGE(.BOTH.,#71768);
#71747=SURFACE_STYLE_USAGE(.BOTH.,#71769);
#71748=SURFACE_STYLE_USAGE(.BOTH.,#71770);
#71749=SURFACE_STYLE_USAGE(.BOTH.,#71771);
#71750=SURFACE_SIDE_STYLE('',(#71772));
#71751=SURFACE_SIDE_STYLE('',(#71773));
#71752=SURFACE_SIDE_STYLE('',(#71774));
#71753=SURFACE_SIDE_STYLE('',(#71775));
#71754=SURFACE_SIDE_STYLE('',(#71776));
#71755=SURFACE_SIDE_STYLE('',(#71777));
#71756=SURFACE_SIDE_STYLE('',(#71778));
#71757=SURFACE_SIDE_STYLE('',(#71779));
#71758=SURFACE_SIDE_STYLE('',(#71780));
#71759=SURFACE_SIDE_STYLE('',(#71781));
#71760=SURFACE_SIDE_STYLE('',(#71782));
#71761=SURFACE_SIDE_STYLE('',(#71783));
#71762=SURFACE_SIDE_STYLE('',(#71784));
#71763=SURFACE_SIDE_STYLE('',(#71785));
#71764=SURFACE_SIDE_STYLE('',(#71786));
#71765=SURFACE_SIDE_STYLE('',(#71787));
#71766=SURFACE_SIDE_STYLE('',(#71788));
#71767=SURFACE_SIDE_STYLE('',(#71789));
#71768=SURFACE_SIDE_STYLE('',(#71790));
#71769=SURFACE_SIDE_STYLE('',(#71791));
#71770=SURFACE_SIDE_STYLE('',(#71792));
#71771=SURFACE_SIDE_STYLE('',(#71793));
#71772=SURFACE_STYLE_FILL_AREA(#71794);
#71773=SURFACE_STYLE_FILL_AREA(#71795);
#71774=SURFACE_STYLE_FILL_AREA(#71796);
#71775=SURFACE_STYLE_FILL_AREA(#71797);
#71776=SURFACE_STYLE_FILL_AREA(#71798);
#71777=SURFACE_STYLE_FILL_AREA(#71799);
#71778=SURFACE_STYLE_FILL_AREA(#71800);
#71779=SURFACE_STYLE_FILL_AREA(#71801);
#71780=SURFACE_STYLE_FILL_AREA(#71802);
#71781=SURFACE_STYLE_FILL_AREA(#71803);
#71782=SURFACE_STYLE_FILL_AREA(#71804);
#71783=SURFACE_STYLE_FILL_AREA(#71805);
#71784=SURFACE_STYLE_FILL_AREA(#71806);
#71785=SURFACE_STYLE_FILL_AREA(#71807);
#71786=SURFACE_STYLE_FILL_AREA(#71808);
#71787=SURFACE_STYLE_FILL_AREA(#71809);
#71788=SURFACE_STYLE_FILL_AREA(#71810);
#71789=SURFACE_STYLE_FILL_AREA(#71811);
#71790=SURFACE_STYLE_FILL_AREA(#71812);
#71791=SURFACE_STYLE_FILL_AREA(#71813);
#71792=SURFACE_STYLE_FILL_AREA(#71814);
#71793=SURFACE_STYLE_FILL_AREA(#71815);
#71794=FILL_AREA_STYLE('Steel - Satin',(#71816));
#71795=FILL_AREA_STYLE('MAS306_tb',(#71817));
#71796=FILL_AREA_STYLE('MAS306_white',(#71818));
#71797=FILL_AREA_STYLE('MAS306_pl',(#71819));
#71798=FILL_AREA_STYLE('MAS306_bed',(#71820));
#71799=FILL_AREA_STYLE('MAS306_brace',(#71821));
#71800=FILL_AREA_STYLE('MAS306_jack',(#71822));
#71801=FILL_AREA_STYLE('MAS306_ram',(#71823));
#71802=FILL_AREA_STYLE('MAS306_rel',(#71824));
#71803=FILL_AREA_STYLE('MAS306_gauge',(#71825));
#71804=FILL_AREA_STYLE('MAS306_pin',(#71826));
#71805=FILL_AREA_STYLE('MAS306_rclip',(#71827));
#71806=FILL_AREA_STYLE('MAS306_foot',(#71828));
#71807=FILL_AREA_STYLE('MAS306_spr',(#71829));
#71808=FILL_AREA_STYLE('MAS306_eye',(#71830));
#71809=FILL_AREA_STYLE('MAS306_vb',(#71831));
#71810=FILL_AREA_STYLE('MAS306_bolt',(#71832));
#71811=FILL_AREA_STYLE('MAS306_nut',(#71833));
#71812=FILL_AREA_STYLE('MAS306_wsh',(#71834));
#71813=FILL_AREA_STYLE('MAS306_hdl',(#71835));
#71814=FILL_AREA_STYLE('MAS306_grip',(#71836));
#71815=FILL_AREA_STYLE('MAS306_up',(#71837));
#71816=FILL_AREA_STYLE_COLOUR('Steel - Satin',#71838);
#71817=FILL_AREA_STYLE_COLOUR('MAS306_tb',#71839);
#71818=FILL_AREA_STYLE_COLOUR('MAS306_white',#71840);
#71819=FILL_AREA_STYLE_COLOUR('MAS306_pl',#71841);
#71820=FILL_AREA_STYLE_COLOUR('MAS306_bed',#71842);
#71821=FILL_AREA_STYLE_COLOUR('MAS306_brace',#71843);
#71822=FILL_AREA_STYLE_COLOUR('MAS306_jack',#71844);
#71823=FILL_AREA_STYLE_COLOUR('MAS306_ram',#71845);
#71824=FILL_AREA_STYLE_COLOUR('MAS306_rel',#71846);
#71825=FILL_AREA_STYLE_COLOUR('MAS306_gauge',#71847);
#71826=FILL_AREA_STYLE_COLOUR('MAS306_pin',#71848);
#71827=FILL_AREA_STYLE_COLOUR('MAS306_rclip',#71849);
#71828=FILL_AREA_STYLE_COLOUR('MAS306_foot',#71850);
#71829=FILL_AREA_STYLE_COLOUR('MAS306_spr',#71851);
#71830=FILL_AREA_STYLE_COLOUR('MAS306_eye',#71852);
#71831=FILL_AREA_STYLE_COLOUR('MAS306_vb',#71853);
#71832=FILL_AREA_STYLE_COLOUR('MAS306_bolt',#71854);
#71833=FILL_AREA_STYLE_COLOUR('MAS306_nut',#71855);
#71834=FILL_AREA_STYLE_COLOUR('MAS306_wsh',#71856);
#71835=FILL_AREA_STYLE_COLOUR('MAS306_hdl',#71857);
#71836=FILL_AREA_STYLE_COLOUR('MAS306_grip',#71858);
#71837=FILL_AREA_STYLE_COLOUR('MAS306_up',#71859);
#71838=COLOUR_RGB('Steel - Satin',0.627450980392157,0.627450980392157,0.627450980392157);
#71839=COLOUR_RGB('MAS306_tb',0.145098039215686,0.356862745098039,0.811764705882353);
#71840=COLOUR_RGB('MAS306_white',0.925490196078431,0.925490196078431,0.909803921568627);
#71841=COLOUR_RGB('MAS306_pl',0.12156862745098,0.333333333333333,0.788235294117647);
#71842=COLOUR_RGB('MAS306_bed',0.141176470588235,0.352941176470588,0.807843137254902);
#71843=COLOUR_RGB('MAS306_brace',0.137254901960784,0.349019607843137,0.803921568627451);
#71844=COLOUR_RGB('MAS306_jack',0.109803921568627,0.32156862745098,0.776470588235294);
#71845=COLOUR_RGB('MAS306_ram',0.83921568627451,0.850980392156863,0.870588235294118);
#71846=COLOUR_RGB('MAS306_rel',0.117647058823529,0.117647058823529,0.125490196078431);
#71847=COLOUR_RGB('MAS306_gauge',0.109803921568627,0.109803921568627,0.117647058823529);
#71848=COLOUR_RGB('MAS306_pin',0.807843137254902,0.819607843137255,0.83921568627451);
#71849=COLOUR_RGB('MAS306_rclip',0.831372549019608,0.843137254901961,0.862745098039216);
#71850=COLOUR_RGB('MAS306_foot',0.129411764705882,0.341176470588235,0.796078431372549);
#71851=COLOUR_RGB('MAS306_spr',0.156862745098039,0.156862745098039,0.164705882352941);
#71852=COLOUR_RGB('MAS306_eye',0.784313725490196,0.8,0.819607843137255);
#71853=COLOUR_RGB('MAS306_vb',0.125490196078431,0.125490196078431,0.133333333333333);
#71854=COLOUR_RGB('MAS306_bolt',0.776470588235294,0.792156862745098,0.815686274509804);
#71855=COLOUR_RGB('MAS306_nut',0.792156862745098,0.807843137254902,0.827450980392157);
#71856=COLOUR_RGB('MAS306_wsh',0.823529411764706,0.835294117647059,0.854901960784314);
#71857=COLOUR_RGB('MAS306_hdl',0.149019607843137,0.36078431372549,0.815686274509804);
#71858=COLOUR_RGB('MAS306_grip',0.101960784313725,0.101960784313725,0.109803921568627);
#71859=COLOUR_RGB('MAS306_up',0.133333333333333,0.345098039215686,0.8);
#71860=COLOUR_RGB('Dark Blue',0.08,0.2,0.34);
#71861=FILL_AREA_STYLE_COLOUR('',#71860);
#71862=FILL_AREA_STYLE('',(#71861));
#71863=SURFACE_STYLE_FILL_AREA(#71862);
#71864=SURFACE_SIDE_STYLE('',(#71863));
#71865=SURFACE_STYLE_USAGE(.BOTH.,#71864);
#71866=PRESENTATION_STYLE_ASSIGNMENT((#71865));
#71867=COLOUR_RGB('Light Blue',0.38,0.62,0.78);
#71868=FILL_AREA_STYLE_COLOUR('',#71867);
#71869=FILL_AREA_STYLE('',(#71868));
#71870=SURFACE_STYLE_FILL_AREA(#71869);
#71871=SURFACE_SIDE_STYLE('',(#71870));
#71872=SURFACE_STYLE_USAGE(.BOTH.,#71871);
#71873=PRESENTATION_STYLE_ASSIGNMENT((#71872));
#71874=COLOUR_RGB('Sky Blue',0.24,0.69,0.87);
#71875=FILL_AREA_STYLE_COLOUR('',#71874);
#71876=FILL_AREA_STYLE('',(#71875));
#71877=SURFACE_STYLE_FILL_AREA(#71876);
#71878=SURFACE_SIDE_STYLE('',(#71877));
#71879=SURFACE_STYLE_USAGE(.BOTH.,#71878);
#71880=PRESENTATION_STYLE_ASSIGNMENT((#71879));
#71881=COLOUR_RGB('Grey',0.48,0.52,0.57);
#71882=FILL_AREA_STYLE_COLOUR('',#71881);
#71883=FILL_AREA_STYLE('',(#71882));
#71884=SURFACE_STYLE_FILL_AREA(#71883);
#71885=SURFACE_SIDE_STYLE('',(#71884));
#71886=SURFACE_STYLE_USAGE(.BOTH.,#71885);
#71887=PRESENTATION_STYLE_ASSIGNMENT((#71886));
#71888=COLOUR_RGB('Black',0.12,0.14,0.17);
#71889=FILL_AREA_STYLE_COLOUR('',#71888);
#71890=FILL_AREA_STYLE('',(#71889));
#71891=SURFACE_STYLE_FILL_AREA(#71890);
#71892=SURFACE_SIDE_STYLE('',(#71891));
#71893=SURFACE_STYLE_USAGE(.BOTH.,#71892);
#71894=PRESENTATION_STYLE_ASSIGNMENT((#71893));
#71895=COLOUR_RGB('Off White',0.89,0.88,0.83);
#71896=FILL_AREA_STYLE_COLOUR('',#71895);
#71897=FILL_AREA_STYLE('',(#71896));
#71898=SURFACE_STYLE_FILL_AREA(#71897);
#71899=SURFACE_SIDE_STYLE('',(#71898));
#71900=SURFACE_STYLE_USAGE(.BOTH.,#71899);
#71901=PRESENTATION_STYLE_ASSIGNMENT((#71900));
ENDSEC;
END-ISO-10303-21;
